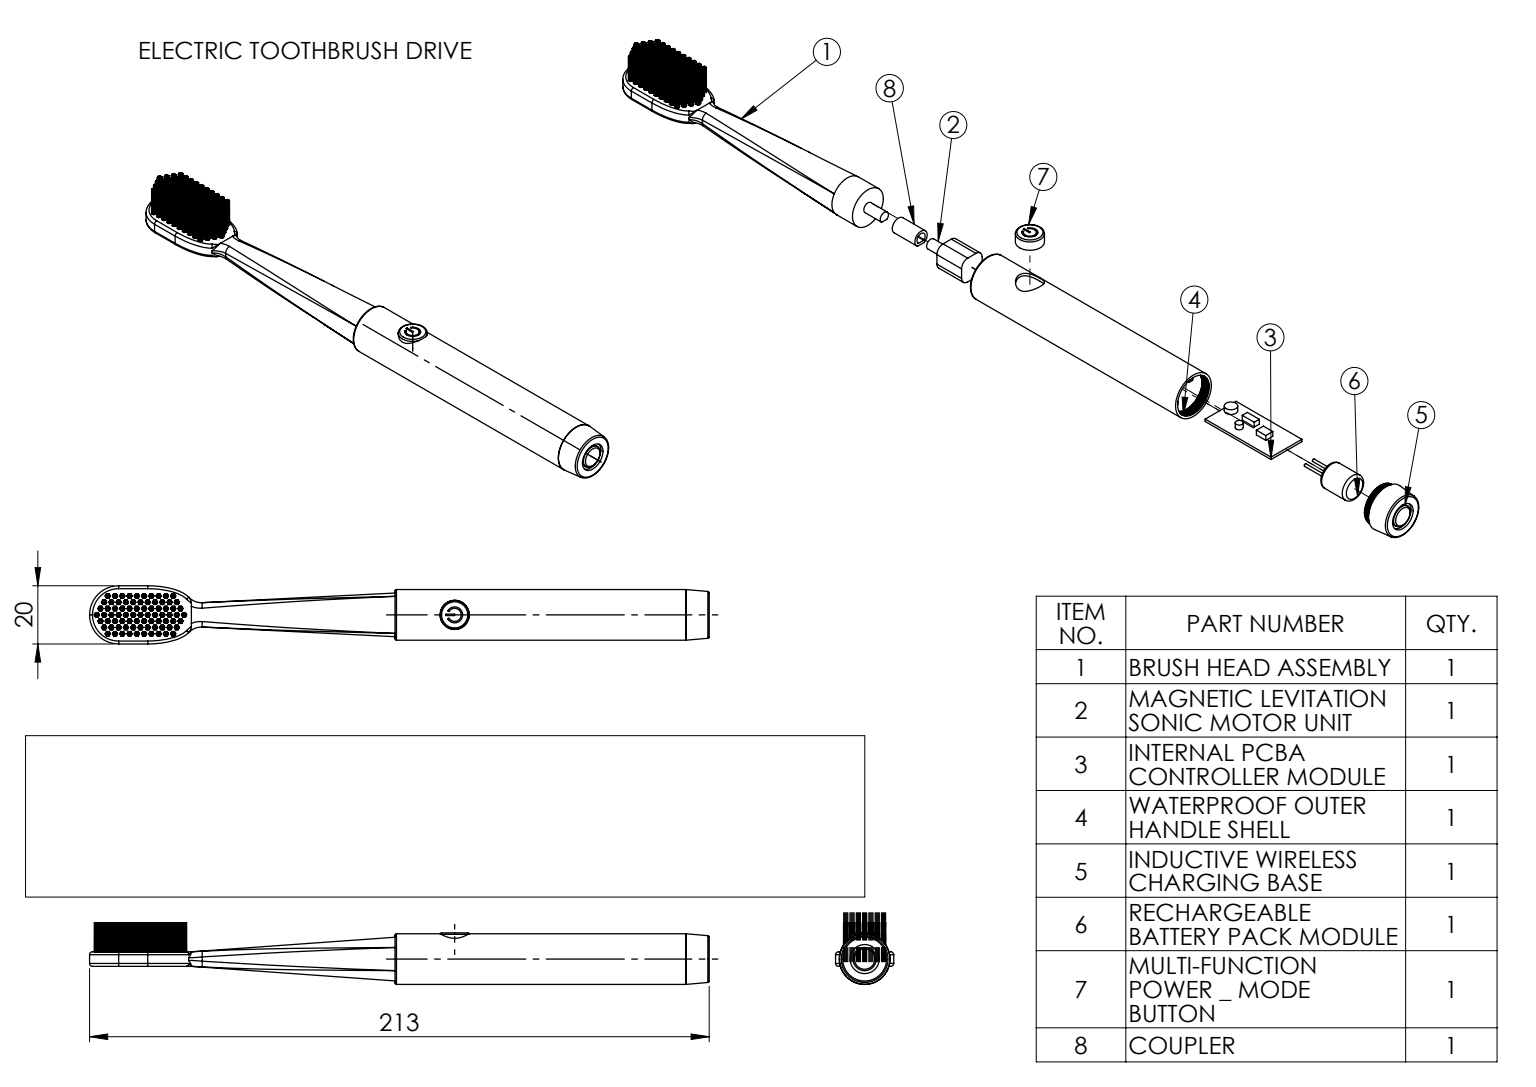
ISO-10303-21;
HEADER;
FILE_DESCRIPTION (('STEP AP214'),
    '1' );
FILE_NAME ('BR-831',
    '2026-10-02T09:26:43',
    ( '' ),
    ( '' ),
    'SwSTEP 2.0',
    'SolidWorks 2026',
    '' );
FILE_SCHEMA (( 'AUTOMOTIVE_DESIGN' ));
ENDSEC;

DATA;
#1 = ORIENTED_EDGE ( 'NONE', *, *, #111289, .F. ) ;
#2 = FACE_OUTER_BOUND ( 'NONE', #57861, .T. ) ;
#3 = DIRECTION ( 'NONE',  ( 0.000000000000000000, -0.000000000000000000, 1.000000000000000000 ) ) ;
#4 = EDGE_CURVE ( 'NONE', #10582, #102432, #129340, .T. ) ;
#5 = DIRECTION ( 'NONE',  ( -1.000000000000000000, -0.000000000000000000, -0.000000000000000000 ) ) ;
#6 = CIRCLE ( 'NONE', #73182, 0.09999999999999982514 ) ;
#7 = CARTESIAN_POINT ( 'NONE',  ( -5.200000000000025935, 12.50000000000000000, -3.983716857408426293 ) ) ;
#8 = ADVANCED_FACE ( 'NONE', ( #9369 ), #58491, .T. ) ;
#9 = ORIENTED_EDGE ( 'NONE', *, *, #43622, .T. ) ;
#10 = DIRECTION ( 'NONE',  ( -0.000000000000000000, 1.000000000000000000, -0.000000000000000000 ) ) ;
#12 = AXIS2_PLACEMENT_3D ( 'NONE', #43008, #33796, #72443 ) ;
#11 = AXIS2_PLACEMENT_3D ( 'NONE', #114880, #25207, #65127 ) ;
#13 = DIRECTION ( 'NONE',  ( 0.000000000000000000, 1.000000000000000000, 0.000000000000000000 ) ) ;
#14 = DIRECTION ( 'NONE',  ( 0.000000000000000000, 1.000000000000000000, 0.000000000000000000 ) ) ;
#15 = DIRECTION ( 'NONE',  ( 0.000000000000000000, 0.000000000000000000, 1.000000000000000000 ) ) ;
#16 = ORIENTED_EDGE ( 'NONE', *, *, #85327, .F. ) ;
#17 = ADVANCED_FACE ( 'NONE', ( #79412 ), #68276, .T. ) ;
#18 = ORIENTED_EDGE ( 'NONE', *, *, #72941, .T. ) ;
#19 = EDGE_CURVE ( 'NONE', #47255, #7520, #102130, .T. ) ;
#20 = LINE ( 'NONE', #41902, #103658 ) ;
#21 = ORIENTED_EDGE ( 'NONE', *, *, #108659, .T. ) ;
#22 = DIRECTION ( 'NONE',  ( 0.000000000000000000, -0.000000000000000000, 1.000000000000000000 ) ) ;
#25 = CARTESIAN_POINT ( 'NONE',  ( 17.50000000000000000, -2.499999999999999556, 2.333333333333337478 ) ) ;
#24 = CIRCLE ( 'NONE', #104488, 0.1000000000000002554 ) ;
#23 = AXIS2_PLACEMENT_3D ( 'NONE', #13282, #3477, #97012 ) ;
#26 = DIRECTION ( 'NONE',  ( -0.000000000000000000, -1.000000000000000000, -0.000000000000000000 ) ) ;
#27 = VERTEX_POINT ( 'NONE', #38865 ) ;
#28 = EDGE_CURVE ( 'NONE', #7615, #17965, #5955, .T. ) ;
#29 = CARTESIAN_POINT ( 'NONE',  ( -3.350000000000028511, 2.500000000000000000, -1.472243186433550122 ) ) ;
#30 = CARTESIAN_POINT ( 'NONE',  ( 4.549999999999939426, 2.500000000000000000, -6.495190528383302464 ) ) ;
#31 = DIRECTION ( 'NONE',  ( 0.000000000000000000, 0.000000000000000000, 1.000000000000000000 ) ) ;
#32 = DIRECTION ( 'NONE',  ( 0.000000000000000000, 0.000000000000000000, -1.000000000000000000 ) ) ;
#33 = DIRECTION ( 'NONE',  ( 0.000000000000000000, -0.000000000000000000, 1.000000000000000000 ) ) ;
#34 = EDGE_CURVE ( 'NONE', #123793, #101138, #123060, .T. ) ;
#35 = DIRECTION ( 'NONE',  ( 0.000000000000000000, 0.000000000000000000, 1.000000000000000000 ) ) ;
#36 = EDGE_LOOP ( 'NONE', ( #12557, #1627 ) ) ;
#37 = ORIENTED_EDGE ( 'NONE', *, *, #25424, .T. ) ;
#38 = CARTESIAN_POINT ( 'NONE',  ( -12.09999999999999609, 12.50000000000000000, -3.637306695894647390 ) ) ;
#39 = ORIENTED_EDGE ( 'NONE', *, *, #32172, .F. ) ;
#40 = DIRECTION ( 'NONE',  ( -0.000000000000000000, 1.000000000000000000, -0.000000000000000000 ) ) ;
#42 = ORIENTED_EDGE ( 'NONE', *, *, #56795, .T. ) ;
#41 = ORIENTED_EDGE ( 'NONE', *, *, #63489, .F. ) ;
#43 = ORIENTED_EDGE ( 'NONE', *, *, #113565, .F. ) ;
#44 = CARTESIAN_POINT ( 'NONE',  ( 87.49999999999998579, 2.781865847474100040, -7.000342182495692178 ) ) ;
#45 = CIRCLE ( 'NONE', #54416, 0.09999999999999982514 ) ;
#46 = CARTESIAN_POINT ( 'NONE',  ( -4.150000000000027889, 12.50000000000000000, -7.253104124594891289 ) ) ;
#47 = AXIS2_PLACEMENT_3D ( 'NONE', #50299, #49672, #91507 ) ;
#48 = CARTESIAN_POINT ( 'NONE',  ( 10.44999999999991047, 2.500000000000000000, 2.065063509461097624 ) ) ;
#49 = CARTESIAN_POINT ( 'NONE',  ( -7.300000000000018474, 12.50000000000000000, 0.3464101615137735735 ) ) ;
#50 = DIRECTION ( 'NONE',  ( 0.000000000000000000, -1.000000000000000000, 0.000000000000000000 ) ) ;
#51 = DIRECTION ( 'NONE',  ( 0.000000000000000000, 1.000000000000000000, 0.000000000000000000 ) ) ;
#52 = CARTESIAN_POINT ( 'NONE',  ( 5.649999999999932854, 2.500000000000000000, 1.918653347947321564 ) ) ;
#53 = DIRECTION ( 'NONE',  ( 0.000000000000000000, 0.000000000000000000, 1.000000000000000000 ) ) ;
#55 = AXIS2_PLACEMENT_3D ( 'NONE', #102666, #47947, #87846 ) ;
#54 = FACE_OUTER_BOUND ( 'NONE', #43393, .T. ) ;
#56 = ORIENTED_EDGE ( 'NONE', *, *, #30639, .F. ) ;
#57 = ORIENTED_EDGE ( 'NONE', *, *, #57612, .F. ) ;
#58 = DIRECTION ( 'NONE',  ( 0.000000000000000000, 0.000000000000000000, -1.000000000000000000 ) ) ;
#59 = EDGE_LOOP ( 'NONE', ( #8980, #73677, #9720, #73966 ) ) ;
#60 = EDGE_LOOP ( 'NONE', ( #125831, #14201 ) ) ;
#61 = CARTESIAN_POINT ( 'NONE',  ( 139.9358549477330200, 0.5000000000000000000, -1.098523788719517169 ) ) ;
#62 = CIRCLE ( 'NONE', #54353, 0.09999999999999982514 ) ;
#63 = EDGE_CURVE ( 'NONE', #31481, #67997, #18539, .T. ) ;
#64 = AXIS2_PLACEMENT_3D ( 'NONE', #6513, #46469, #75933 ) ;
#65 = DIRECTION ( 'NONE',  ( 1.000000000000000000, -0.000000000000000000, -0.000000000000000000 ) ) ;
#66 = CIRCLE ( 'NONE', #71172, 0.09999999999999982514 ) ;
#67 = DIRECTION ( 'NONE',  ( -4.274815082592931898E-19, -0.9999939076577903929, -0.003490651415223739937 ) ) ;
#68 = PLANE ( 'NONE',  #922 ) ;
#69 = ADVANCED_FACE ( 'NONE', ( #17890 ), #95870, .T. ) ;
#70 = DIRECTION ( 'NONE',  ( 0.000000000000000000, -0.9999939076577903929, 0.003490651415223739937 ) ) ;
#71 = ORIENTED_EDGE ( 'NONE', *, *, #16257, .F. ) ;
#72 = EDGE_CURVE ( 'NONE', #118132, #124753, #125105, .T. ) ;
#73 = EDGE_CURVE ( 'NONE', #114203, #127721, #49320, .T. ) ;
#75 = ADVANCED_FACE ( 'NONE', ( #29656 ), #54076, .T. ) ;
#74 = AXIS2_PLACEMENT_3D ( 'NONE', #92885, #52954, #31387 ) ;
#76 = VERTEX_POINT ( 'NONE', #89217 ) ;
#77 = PLANE ( 'NONE',  #104864 ) ;
#78 = EDGE_LOOP ( 'NONE', ( #93082, #10412 ) ) ;
#79 = CARTESIAN_POINT ( 'NONE',  ( 3.549999999999941203, 2.500000000000000000, 6.248780366869521430 ) ) ;
#80 = EDGE_CURVE ( 'NONE', #111625, #116591, #38188, .T. ) ;
#81 = AXIS2_PLACEMENT_3D ( 'NONE', #66786, #108010, #119130 ) ;
#82 = ORIENTED_EDGE ( 'NONE', *, *, #37576, .T. ) ;
#83 = ORIENTED_EDGE ( 'NONE', *, *, #49852, .F. ) ;
#84 = DIRECTION ( 'NONE',  ( -0.000000000000000000, 1.000000000000000000, -0.000000000000000000 ) ) ;
#85 = CARTESIAN_POINT ( 'NONE',  ( -7.100000000000017408, 2.500000000000000000, -4.922947341949753586 ) ) ;
#86 = EDGE_CURVE ( 'NONE', #7115, #38409, #127252, .T. ) ;
#87 = ADVANCED_FACE ( 'NONE', ( #57833 ), #118026, .T. ) ;
#88 = CARTESIAN_POINT ( 'NONE',  ( 13.34999999999990017, 2.500000000000000000, 1.572243186433545548 ) ) ;
#89 = DIRECTION ( 'NONE',  ( 0.000000000000000000, 0.000000000000000000, 1.000000000000000000 ) ) ;
#90 = CARTESIAN_POINT ( 'NONE',  ( 17.50000000000000000, -2.083333333333333925, 4.000000000000001776 ) ) ;
#91 = ORIENTED_EDGE ( 'NONE', *, *, #128566, .T. ) ;
#92 =( BOUNDED_CURVE ( )  B_SPLINE_CURVE ( 2, ( #80530, #51076, #39332, #70696, #90980, #28848, #108684 ),
 .UNSPECIFIED., .F., .F. ) 
 B_SPLINE_CURVE_WITH_KNOTS ( ( 3, 2, 2, 3 ),
 ( 0.7142857142857148567, 0.7380952380952386926, 0.7619047619047624176, 0.7857142857142862535 ),
 .UNSPECIFIED. ) 
 CURVE ( )  GEOMETRIC_REPRESENTATION_ITEM ( )  RATIONAL_B_SPLINE_CURVE ( ( 0.9999999999999968914, 0.8660254037844418162, 1.000000000000000000, 0.8660254037844387076, 1.000000000000000000, 0.8660254037844355990, 1.000000000000003109 ) ) 
 REPRESENTATION_ITEM ( '' )  );
#93 = DIRECTION ( 'NONE',  ( -0.000000000000000000, 1.000000000000000000, -0.000000000000000000 ) ) ;
#94 = DIRECTION ( 'NONE',  ( -4.274815082592931898E-19, -0.9999939076577903929, -0.003490651415223739937 ) ) ;
#95 = CARTESIAN_POINT ( 'NONE',  ( -2.050000000000033129, 2.500000000000000000, 2.165063509461097713 ) ) ;
#96 = CARTESIAN_POINT ( 'NONE',  ( -2.950000000000029932, 2.500000000000000000, -2.165063509461101710 ) ) ;
#97 = FACE_OUTER_BOUND ( 'NONE', #13668, .T. ) ;
#98 = EDGE_LOOP ( 'NONE', ( #5007, #26491, #107521, #16284 ) ) ;
#99 = ORIENTED_EDGE ( 'NONE', *, *, #48484, .T. ) ;
#100 = CIRCLE ( 'NONE', #16803, 0.06509327318403745899 ) ;
#101 = DIRECTION ( 'NONE',  ( 0.000000000000000000, -0.000000000000000000, 1.000000000000000000 ) ) ;
#102 = AXIS2_PLACEMENT_3D ( 'NONE', #59335, #77010, #59983 ) ;
#103 = ORIENTED_EDGE ( 'NONE', *, *, #8467, .T. ) ;
#104 = CARTESIAN_POINT ( 'NONE',  ( 17.41716098457700923, -1.872967139268051806, 4.643356076170615410 ) ) ;
#105 = LINE ( 'NONE', #118591, #98263 ) ;
#106 = AXIS2_PLACEMENT_3D ( 'NONE', #112814, #42811, #102353 ) ;
#107 = VERTEX_POINT ( 'NONE', #106909 ) ;
#108 = DIRECTION ( 'NONE',  ( 0.000000000000000000, 1.000000000000000000, 0.000000000000000000 ) ) ;
#109 = CARTESIAN_POINT ( 'NONE',  ( -6.650000000000019007, 2.500000000000000000, -5.802370205355749988 ) ) ;
#110 = CARTESIAN_POINT ( 'NONE',  ( 10.39999999999991509, 12.50000000000000000, -0.6928203230275542523 ) ) ;
#111 = CARTESIAN_POINT ( 'NONE',  ( 133.2169897921533845, 2.500000000000000000, -4.655597831175330548 ) ) ;
#112 = FACE_OUTER_BOUND ( 'NONE', #22375, .T. ) ;
#113 = VERTEX_POINT ( 'NONE', #17219 ) ;
#114 = DIRECTION ( 'NONE',  ( 0.000000000000000000, -0.9999939076577903929, 0.003490651415223739937 ) ) ;
#115 = DIRECTION ( 'NONE',  ( 0.000000000000000000, 0.000000000000000000, 1.000000000000000000 ) ) ;
#116 = CARTESIAN_POINT ( 'NONE',  ( -5.200000000000022382, 12.50000000000000000, 0.2813168883297361700 ) ) ;
#117 = ADVANCED_FACE ( 'NONE', ( #57173 ), #7419, .T. ) ;
#118 = VERTEX_POINT ( 'NONE', #50574 ) ;
#119 = DIRECTION ( 'NONE',  ( -0.000000000000000000, 1.000000000000000000, -0.000000000000000000 ) ) ;
#120 = EDGE_LOOP ( 'NONE', ( #58165, #15953, #18369, #114695 ) ) ;
#121 = CARTESIAN_POINT ( 'NONE',  ( -3.000000000000000000, 3.673940397442059868E-16, -5.000000000000004441 ) ) ;
#122 = DIRECTION ( 'NONE',  ( 0.000000000000000000, -0.000000000000000000, 1.000000000000000000 ) ) ;
#123 = DIRECTION ( 'NONE',  ( -4.274815082592931898E-19, -0.9999939076577903929, -0.003490651415223739937 ) ) ;
#124 = VERTEX_POINT ( 'NONE', #122556 ) ;
#125 = VECTOR ( 'NONE', #104094, 1000.000000000000000 ) ;
#126 = CARTESIAN_POINT ( 'NONE',  ( 2.099999999999950351, 12.50000000000000000, -5.022947341949754119 ) ) ;
#127 = CONICAL_SURFACE ( 'NONE', #108793, 0.1000000000000000472, 0.003490658503988666988 ) ;
#128 = CARTESIAN_POINT ( 'NONE',  ( 1.449999999999951328, 12.50000000000000000, -1.883746621131363597 ) ) ;
#129 = EDGE_LOOP ( 'NONE', ( #126937, #8373, #2231, #124616 ) ) ;
#130 = CARTESIAN_POINT ( 'NONE',  ( 8.749999999999957367, 2.500000000000000000, -6.595190528383302109 ) ) ;
#131 = EDGE_LOOP ( 'NONE', ( #50533, #103161, #4898, #53969 ) ) ;
#132 = CONICAL_SURFACE ( 'NONE', #108799, 0.1000000000000002554, 0.003490658503988666988 ) ;
#133 = FACE_OUTER_BOUND ( 'NONE', #40974, .T. ) ;
#134 = ORIENTED_EDGE ( 'NONE', *, *, #111458, .F. ) ;
#135 = DIRECTION ( 'NONE',  ( 0.000000000000000000, 0.000000000000000000, 1.000000000000000000 ) ) ;
#136 = CARTESIAN_POINT ( 'NONE',  ( -5.000000000000023093, 2.500000000000000000, 5.022947341949748790 ) ) ;
#137 = VERTEX_POINT ( 'NONE', #41429 ) ;
#138 = ORIENTED_EDGE ( 'NONE', *, *, #94725, .F. ) ;
#139 = DIRECTION ( 'NONE',  ( -0.000000000000000000, 1.000000000000000000, -0.000000000000000000 ) ) ;
#140 = FACE_OUTER_BOUND ( 'NONE', #29426, .T. ) ;
#141 = ORIENTED_EDGE ( 'NONE', *, *, #10108, .F. ) ;
#143 = FACE_OUTER_BOUND ( 'NONE', #8076, .T. ) ;
#142 = AXIS2_PLACEMENT_3D ( 'NONE', #9136, #110553, #47778 ) ;
#144 = CARTESIAN_POINT ( 'NONE',  ( 187.0677083336747160, -4.367472073101514418, -7.564683531250002702 ) ) ;
#145 = AXIS2_PLACEMENT_3D ( 'NONE', #45558, #95932, #15417 ) ;
#146 = DIRECTION ( 'NONE',  ( 0.000000000000000000, 0.000000000000000000, 1.000000000000000000 ) ) ;
#147 = CARTESIAN_POINT ( 'NONE',  ( -13.94999999999998685, 12.50000000000000000, -2.576566944158912964 ) ) ;
#148 = CARTESIAN_POINT ( 'NONE',  ( -8.300000000000009592, 12.50000000000000000, 4.395220292106234439 ) ) ;
#149 = DIRECTION ( 'NONE',  ( 0.000000000000000000, 0.000000000000000000, -1.000000000000000000 ) ) ;
#150 = CARTESIAN_POINT ( 'NONE',  ( -0.6500000000000394351, 2.500000000000000000, 6.941600689897073018 ) ) ;
#151 = CONICAL_SURFACE ( 'NONE', #75377, 0.09999999999999982514, 0.003490658503988666988 ) ;
#152 = EDGE_CURVE ( 'NONE', #35689, #125708, #77064, .T. ) ;
#153 = ORIENTED_EDGE ( 'NONE', *, *, #4789, .F. ) ;
#154 = ORIENTED_EDGE ( 'NONE', *, *, #109368, .T. ) ;
#155 = ORIENTED_EDGE ( 'NONE', *, *, #127999, .F. ) ;
#156 = AXIS2_PLACEMENT_3D ( 'NONE', #115565, #16713, #35116 ) ;
#157 = CARTESIAN_POINT ( 'NONE',  ( -6.249999999999981348, 12.50000000000000000, 2.165063509461097713 ) ) ;
#158 = DIRECTION ( 'NONE',  ( -0.000000000000000000, 1.000000000000000000, -0.000000000000000000 ) ) ;
#159 = DIRECTION ( 'NONE',  ( 0.000000000000000000, 0.000000000000000000, 1.000000000000000000 ) ) ;
#160 = EDGE_LOOP ( 'NONE', ( #92531, #41100 ) ) ;
#161 = EDGE_CURVE ( 'NONE', #53677, #62914, #60358, .T. ) ;
#162 = FACE_BOUND ( 'NONE', #99510, .T. ) ;
#163 = ORIENTED_EDGE ( 'NONE', *, *, #63007, .F. ) ;
#164 = EDGE_CURVE ( 'NONE', #64447, #41921, #37367, .T. ) ;
#165 = CARTESIAN_POINT ( 'NONE',  ( -7.900000000000014566, 12.50000000000000000, 0.6277270498435120194 ) ) ;
#166 = CARTESIAN_POINT ( 'NONE',  ( 7.899999999999924860, 2.500000000000000000, 5.022947341949748790 ) ) ;
#167 = LINE ( 'NONE', #110140, #49263 ) ;
#168 = FACE_OUTER_BOUND ( 'NONE', #42884, .T. ) ;
#169 = DIRECTION ( 'NONE',  ( -0.000000000000000000, 1.000000000000000000, -0.000000000000000000 ) ) ;
#170 = EDGE_CURVE ( 'NONE', #109777, #63696, #31113, .T. ) ;
#171 = DIRECTION ( 'NONE',  ( 0.000000000000000000, 1.000000000000000000, 0.000000000000000000 ) ) ;
#172 = EDGE_CURVE ( 'NONE', #110736, #16781, #3893, .T. ) ;
#173 = DIRECTION ( 'NONE',  ( 0.000000000000000000, 0.000000000000000000, -1.000000000000000000 ) ) ;
#174 = EDGE_CURVE ( 'NONE', #53227, #49994, #90490, .T. ) ;
#175 = CARTESIAN_POINT ( 'NONE',  ( 11.84999999999990727, 2.500000000000000000, 6.841600689897072485 ) ) ;
#176 = ADVANCED_FACE ( 'NONE', ( #101629 ), #14347, .T. ) ;
#177 = FACE_OUTER_BOUND ( 'NONE', #72478, .T. ) ;
#178 = ORIENTED_EDGE ( 'NONE', *, *, #7339, .F. ) ;
#179 = VERTEX_POINT ( 'NONE', #111417 ) ;
#180 = VERTEX_POINT ( 'NONE', #20488 ) ;
#181 = VERTEX_POINT ( 'NONE', #62977 ) ;
#182 = DIRECTION ( 'NONE',  ( 0.000000000000000000, 1.000000000000000000, 0.000000000000000000 ) ) ;
#183 = CIRCLE ( 'NONE', #48229, 0.06509327318403741736 ) ;
#184 = LINE ( 'NONE', #92445, #36085 ) ;
#185 = AXIS2_PLACEMENT_3D ( 'NONE', #74145, #15849, #15191 ) ;
#186 = AXIS2_PLACEMENT_3D ( 'NONE', #87460, #107759, #127405 ) ;
#188 = ORIENTED_EDGE ( 'NONE', *, *, #84597, .T. ) ;
#187 = EDGE_LOOP ( 'NONE', ( #105520, #67716, #77716, #43576 ) ) ;
#189 = EDGE_CURVE ( 'NONE', #19176, #5233, #120978, .T. ) ;
#190 = ORIENTED_EDGE ( 'NONE', *, *, #82832, .T. ) ;
#191 = AXIS2_PLACEMENT_3D ( 'NONE', #50501, #49243, #90414 ) ;
#192 = DIRECTION ( 'NONE',  ( -0.000000000000000000, -1.000000000000000000, -0.000000000000000000 ) ) ;
#193 = DIRECTION ( 'NONE',  ( 0.000000000000000000, -0.000000000000000000, 1.000000000000000000 ) ) ;
#194 = DIRECTION ( 'NONE',  ( -0.000000000000000000, -1.000000000000000000, -0.000000000000000000 ) ) ;
#195 = DIRECTION ( 'NONE',  ( 0.000000000000000000, 0.000000000000000000, -1.000000000000000000 ) ) ;
#196 = CARTESIAN_POINT ( 'NONE',  ( -8.950000000000004619, 12.50000000000000000, 6.148780366869520897 ) ) ;
#197 = CONICAL_SURFACE ( 'NONE', #119337, 0.1000000000000000056, 0.003490658503988666988 ) ;
#198 = DIRECTION ( 'NONE',  ( 0.000000000000000000, -0.000000000000000000, 1.000000000000000000 ) ) ;
#199 = ORIENTED_EDGE ( 'NONE', *, *, #119327, .F. ) ;
#200 = DIRECTION ( 'NONE',  ( 0.000000000000000000, -0.9999939076577903929, 0.003490651415223739937 ) ) ;
#201 = ORIENTED_EDGE ( 'NONE', *, *, #13341, .F. ) ;
#202 = ORIENTED_EDGE ( 'NONE', *, *, #70316, .F. ) ;
#203 = ORIENTED_EDGE ( 'NONE', *, *, #126845, .T. ) ;
#204 = DIRECTION ( 'NONE',  ( -0.000000000000000000, -1.000000000000000000, -0.000000000000000000 ) ) ;
#205 = EDGE_CURVE ( 'NONE', #70284, #50485, #21114, .T. ) ;
#206 = ORIENTED_EDGE ( 'NONE', *, *, #92160, .F. ) ;
#207 = ORIENTED_EDGE ( 'NONE', *, *, #83833, .F. ) ;
#208 = FILL_AREA_STYLE ('',( #102307 ) ) ;
#209 = AXIS2_PLACEMENT_3D ( 'NONE', #67296, #8398, #18868 ) ;
#210 = CARTESIAN_POINT ( 'NONE',  ( 9.399999999999915090, 2.500000000000000000, 3.983716857408420964 ) ) ;
#211 = CARTESIAN_POINT ( 'NONE',  ( 14.14999999999989377, 2.500000000000000000, -2.857883832488653741 ) ) ;
#212 = DIRECTION ( 'NONE',  ( -0.000000000000000000, 1.000000000000000000, -0.000000000000000000 ) ) ;
#213 = ADVANCED_FACE ( 'NONE', ( #70872 ), #100964, .T. ) ;
#214 = DIRECTION ( 'NONE',  ( -0.000000000000000000, 1.000000000000000000, -0.000000000000000000 ) ) ;
#215 = EDGE_CURVE ( 'NONE', #14404, #106677, #98609, .T. ) ;
#216 = ORIENTED_EDGE ( 'NONE', *, *, #25647, .T. ) ;
#217 = EDGE_CURVE ( 'NONE', #101886, #26135, #31742, .T. ) ;
#218 = DIRECTION ( 'NONE',  ( 0.000000000000000000, 1.000000000000000000, 0.000000000000000000 ) ) ;
#219 = CONICAL_SURFACE ( 'NONE', #115215, 0.1000000000000000472, 0.003490658503988666988 ) ;
#220 = CIRCLE ( 'NONE', #73386, 0.06509327318403745899 ) ;
#221 = ORIENTED_EDGE ( 'NONE', *, *, #31291, .F. ) ;
#223 = EDGE_CURVE ( 'NONE', #51195, #50358, #69379, .T. ) ;
#222 = DIRECTION ( 'NONE',  ( 0.000000000000000000, 0.000000000000000000, 1.000000000000000000 ) ) ;
#224 = VERTEX_POINT ( 'NONE', #112735 ) ;
#225 = DIRECTION ( 'NONE',  ( -0.000000000000000000, 1.000000000000000000, -0.000000000000000000 ) ) ;
#226 = CARTESIAN_POINT ( 'NONE',  ( 21.24754738303297330, 0.7337760880902002292, -4.182111650399407132 ) ) ;
#228 = ORIENTED_EDGE ( 'NONE', *, *, #115605, .T. ) ;
#227 = ADVANCED_FACE ( 'NONE', ( #89853 ), #30320, .T. ) ;
#229 = CARTESIAN_POINT ( 'NONE',  ( 5.599999999999931255, 12.50000000000000000, 3.918623584224382839 ) ) ;
#230 = EDGE_CURVE ( 'NONE', #34015, #92739, #32256, .T. ) ;
#231 = DIRECTION ( 'NONE',  ( 0.000000000000000000, 0.000000000000000000, -1.000000000000000000 ) ) ;
#232 = EDGE_LOOP ( 'NONE', ( #14783, #39929, #121308, #33112 ) ) ;
#233 = CONICAL_SURFACE ( 'NONE', #8535, 0.1000000000000002554, 0.003490658503988666988 ) ;
#234 = EDGE_CURVE ( 'NONE', #45310, #78495, #22435, .T. ) ;
#235 = AXIS2_PLACEMENT_3D ( 'NONE', #117904, #58371, #98266 ) ;
#236 = EDGE_CURVE ( 'NONE', #86441, #35274, #92360, .T. ) ;
#237 = EDGE_CURVE ( 'NONE', #3662, #62906, #43359, .T. ) ;
#238 = CARTESIAN_POINT ( 'NONE',  ( 10.64999999999990976, 12.50000000000000000, 1.753560074763284016 ) ) ;
#239 = ORIENTED_EDGE ( 'NONE', *, *, #20618, .F. ) ;
#240 = VERTEX_POINT ( 'NONE', #115266 ) ;
#241 = DIRECTION ( 'NONE',  ( 0.000000000000000000, 0.000000000000000000, 1.000000000000000000 ) ) ;
#242 = FACE_OUTER_BOUND ( 'NONE', #74937, .T. ) ;
#243 = LINE ( 'NONE', #68992, #50135 ) ;
#244 = DIRECTION ( 'NONE',  ( 0.000000000000000000, 0.000000000000000000, 1.000000000000000000 ) ) ;
#245 = EDGE_CURVE ( 'NONE', #43167, #39233, #13868, .T. ) ;
#246 = AXIS2_PLACEMENT_3D ( 'NONE', #45056, #45692, #64672 ) ;
#247 = CIRCLE ( 'NONE', #62948, 0.1000000000000000472 ) ;
#248 = CARTESIAN_POINT ( 'NONE',  ( 6.049999999999935874, 2.500000000000000000, -6.941600689897077459 ) ) ;
#249 = VERTEX_POINT ( 'NONE', #105488 ) ;
#250 = DIRECTION ( 'NONE',  ( -0.000000000000000000, -1.000000000000000000, -0.000000000000000000 ) ) ;
#251 = VERTEX_POINT ( 'NONE', #124483 ) ;
#252 = CARTESIAN_POINT ( 'NONE',  ( -1.450000000000035483, 12.50000000000000000, 1.883746621131358934 ) ) ;
#253 = CARTESIAN_POINT ( 'NONE',  ( 8.099999999999921485, 2.500000000000000000, 0.2464101615137735679 ) ) ;
#254 = AXIS2_PLACEMENT_3D ( 'NONE', #24478, #34962, #47347 ) ;
#255 = AXIS2_PLACEMENT_3D ( 'NONE', #22150, #12292, #81057 ) ;
#256 = CARTESIAN_POINT ( 'NONE',  ( 186.4218750003414016, 0.000000000000000000, 7.564683531250000925 ) ) ;
#257 = PLANE ( 'NONE',  #99050 ) ;
#258 = DIRECTION ( 'NONE',  ( 0.000000000000000000, -0.9999939076577903929, 0.003490651415223739937 ) ) ;
#259 = DIRECTION ( 'NONE',  ( 0.000000000000000000, 0.000000000000000000, 1.000000000000000000 ) ) ;
#260 = CARTESIAN_POINT ( 'NONE',  ( -11.89999999999999680, 2.500000000000000000, -4.576537180435975571 ) ) ;
#261 = ORIENTED_EDGE ( 'NONE', *, *, #25908, .F. ) ;
#262 = DIRECTION ( 'NONE',  ( 0.000000000000000000, -0.9999939076577903929, 0.003490651415223739937 ) ) ;
#263 = DIRECTION ( 'NONE',  ( -0.000000000000000000, 1.000000000000000000, -0.000000000000000000 ) ) ;
#264 = CARTESIAN_POINT ( 'NONE',  ( 13.14999999999989733, 2.500000000000000000, -2.511473670974877948 ) ) ;
#265 = ORIENTED_EDGE ( 'NONE', *, *, #80354, .F. ) ;
#266 = CARTESIAN_POINT ( 'NONE',  ( -11.44999999999999929, 2.500000000000000000, -1.718653347947322052 ) ) ;
#267 = EDGE_CURVE ( 'NONE', #13125, #47712, #71425, .T. ) ;
#268 = EDGE_LOOP ( 'NONE', ( #106768, #28625 ) ) ;
#269 = VERTEX_POINT ( 'NONE', #123201 ) ;
#270 = DIRECTION ( 'NONE',  ( 0.000000000000000000, 0.000000000000000000, 1.000000000000000000 ) ) ;
#271 = AXIS2_PLACEMENT_3D ( 'NONE', #106645, #15669, #35977 ) ;
#272 = AXIS2_PLACEMENT_3D ( 'NONE', #94108, #74472, #114381 ) ;
#273 = AXIS2_PLACEMENT_3D ( 'NONE', #118714, #118066, #68969 ) ;
#274 = EDGE_LOOP ( 'NONE', ( #97297, #118927 ) ) ;
#275 = DIRECTION ( 'NONE',  ( 0.000000000000000000, 0.000000000000000000, 1.000000000000000000 ) ) ;
#276 = CARTESIAN_POINT ( 'NONE',  ( 5.799999999999931433, 12.50000000000000000, 4.395220292106234439 ) ) ;
#277 = ORIENTED_EDGE ( 'NONE', *, *, #87516, .F. ) ;
#279 = LINE ( 'NONE', #110252, #23714 ) ;
#278 = VECTOR ( 'NONE', #38628, 1000.000000000000000 ) ;
#280 = CIRCLE ( 'NONE', #81853, 0.06509327318403741736 ) ;
#281 = DIRECTION ( 'NONE',  ( 0.000000000000000000, -0.9999939076577903929, 0.003490651415223739937 ) ) ;
#282 = DIRECTION ( 'NONE',  ( 0.000000000000000000, 0.000000000000000000, 1.000000000000000000 ) ) ;
#283 = ADVANCED_FACE ( 'NONE', ( #24987 ), #65155, .T. ) ;
#284 = ORIENTED_EDGE ( 'NONE', *, *, #126777, .T. ) ;
#285 = ORIENTED_EDGE ( 'NONE', *, *, #2427, .F. ) ;
#286 = ORIENTED_EDGE ( 'NONE', *, *, #35114, .F. ) ;
#287 = DIRECTION ( 'NONE',  ( -0.000000000000000000, -1.000000000000000000, -0.000000000000000000 ) ) ;
#288 = DIRECTION ( 'NONE',  ( 0.000000000000000000, 0.000000000000000000, 1.000000000000000000 ) ) ;
#289 = DIRECTION ( 'NONE',  ( -0.000000000000000000, 1.000000000000000000, -0.000000000000000000 ) ) ;
#290 = FACE_BOUND ( 'NONE', #126554, .T. ) ;
#291 = ORIENTED_EDGE ( 'NONE', *, *, #83216, .F. ) ;
#292 = DIRECTION ( 'NONE',  ( 0.000000000000000000, 0.000000000000000000, 1.000000000000000000 ) ) ;
#293 = DIRECTION ( 'NONE',  ( 0.000000000000000000, -0.000000000000000000, 1.000000000000000000 ) ) ;
#294 = ORIENTED_EDGE ( 'NONE', *, *, #21313, .F. ) ;
#295 = DIRECTION ( 'NONE',  ( 0.000000000000000000, 0.000000000000000000, -1.000000000000000000 ) ) ;
#296 = CARTESIAN_POINT ( 'NONE',  ( -11.04999999999999893, 2.500000000000000000, 1.818653347947321475 ) ) ;
#297 = DIRECTION ( 'NONE',  ( -0.000000000000000000, -1.000000000000000000, -0.000000000000000000 ) ) ;
#298 = DIRECTION ( 'NONE',  ( 0.000000000000000000, -0.9999939076577903929, 0.003490651415223739937 ) ) ;
#299 = CARTESIAN_POINT ( 'NONE',  ( 2.049999999999950084, 2.500000000000000000, 2.165063509461097713 ) ) ;
#300 = DIRECTION ( 'NONE',  ( 0.000000000000000000, 1.000000000000000000, 0.000000000000000000 ) ) ;
#301 = LINE ( 'NONE', #128666, #48207 ) ;
#302 = CIRCLE ( 'NONE', #73475, 0.1000000000000000472 ) ;
#303 = EDGE_CURVE ( 'NONE', #26935, #23200, #114647, .T. ) ;
#304 = ORIENTED_EDGE ( 'NONE', *, *, #29474, .T. ) ;
#305 = ORIENTED_EDGE ( 'NONE', *, *, #98641, .F. ) ;
#306 = ORIENTED_EDGE ( 'NONE', *, *, #68939, .F. ) ;
#307 = EDGE_LOOP ( 'NONE', ( #81864, #53697, #107603, #18782 ) ) ;
#308 = DIRECTION ( 'NONE',  ( 0.000000000000000000, -0.9999939076577903929, 0.003490651415223739937 ) ) ;
#309 = CARTESIAN_POINT ( 'NONE',  ( 13.74999999999993072, 2.500000000000000000, -2.165063509461101710 ) ) ;
#310 = EDGE_LOOP ( 'NONE', ( #57715, #102459 ) ) ;
#311 = FACE_BOUND ( 'NONE', #39121, .T. ) ;
#312 = ADVANCED_FACE ( 'NONE', ( #15798 ), #25451, .T. ) ;
#313 = LINE ( 'NONE', #12086, #37510 ) ;
#314 = VECTOR ( 'NONE', #88274, 1000.000000000000000 ) ;
#315 = CIRCLE ( 'NONE', #10772, 0.09999999999999982514 ) ;
#316 = DIRECTION ( 'NONE',  ( 0.000000000000000000, 0.000000000000000000, 1.000000000000000000 ) ) ;
#317 = CARTESIAN_POINT ( 'NONE',  ( 2.949999999999943334, 12.50000000000000000, 6.495190528383297135 ) ) ;
#318 = ADVANCED_FACE ( 'NONE', ( #4048 ), #118462, .T. ) ;
#319 = FACE_OUTER_BOUND ( 'NONE', #53920, .T. ) ;
#320 = EDGE_CURVE ( 'NONE', #39409, #2500, #55733, .T. ) ;
#321 = DIRECTION ( 'NONE',  ( 0.000000000000000000, 0.000000000000000000, 1.000000000000000000 ) ) ;
#322 = EDGE_CURVE ( 'NONE', #118758, #53470, #49534, .T. ) ;
#323 = CARTESIAN_POINT ( 'NONE',  ( -1.050000000000038680, 2.500000000000000000, 6.741600689897071952 ) ) ;
#324 = EDGE_CURVE ( 'NONE', #23588, #89858, #112217, .T. ) ;
#325 = EDGE_LOOP ( 'NONE', ( #61905, #50116, #33161, #106060 ) ) ;
#326 = EDGE_CURVE ( 'NONE', #98580, #67678, #66234, .T. ) ;
#327 = AXIS2_PLACEMENT_3D ( 'NONE', #75611, #34437, #106376 ) ;
#328 = ORIENTED_EDGE ( 'NONE', *, *, #89775, .T. ) ;
#329 = CIRCLE ( 'NONE', #90217, 0.06509327318403745899 ) ;
#330 = ORIENTED_EDGE ( 'NONE', *, *, #80772, .F. ) ;
#331 = VERTEX_POINT ( 'NONE', #113362 ) ;
#332 = ORIENTED_EDGE ( 'NONE', *, *, #4672, .F. ) ;
#333 = ORIENTED_EDGE ( 'NONE', *, *, #89472, .T. ) ;
#334 = VECTOR ( 'NONE', #40375, 1000.000000000000000 ) ;
#335 = DIRECTION ( 'NONE',  ( 0.000000000000000000, 1.000000000000000000, 0.000000000000000000 ) ) ;
#336 = DIRECTION ( 'NONE',  ( 0.000000000000000000, 1.000000000000000000, 0.000000000000000000 ) ) ;
#337 = ORIENTED_EDGE ( 'NONE', *, *, #87514, .F. ) ;
#338 = ADVANCED_FACE ( 'NONE', ( #43998 ), #105950, .T. ) ;
#339 = CARTESIAN_POINT ( 'NONE',  ( 11.24999999999990585, 12.50000000000000000, -5.802370205355749988 ) ) ;
#340 = AXIS2_PLACEMENT_3D ( 'NONE', #87388, #97223, #127343 ) ;
#341 = EDGE_CURVE ( 'NONE', #29920, #106540, #93098, .T. ) ;
#342 = EDGE_CURVE ( 'NONE', #41239, #126826, #74090, .T. ) ;
#343 = CARTESIAN_POINT ( 'NONE',  ( 7.049999999999928768, 2.500000000000000000, -2.165063509461101710 ) ) ;
#344 = CIRCLE ( 'NONE', #48391, 0.06509327318403745899 ) ;
#345 = CIRCLE ( 'NONE', #4533, 0.06509327318403745899 ) ;
#346 = CARTESIAN_POINT ( 'NONE',  ( 184.9427083336747160, -6.551208109652278289, 3.782341765624995134 ) ) ;
#347 = DIRECTION ( 'NONE',  ( 0.000000000000000000, 0.000000000000000000, 1.000000000000000000 ) ) ;
#348 = DIRECTION ( 'NONE',  ( 0.000000000000000000, 1.000000000000000000, 0.000000000000000000 ) ) ;
#349 = ORIENTED_EDGE ( 'NONE', *, *, #95079, .T. ) ;
#350 = FACE_OUTER_BOUND ( 'NONE', #62832, .T. ) ;
#351 = ORIENTED_EDGE ( 'NONE', *, *, #55703, .F. ) ;
#352 = ORIENTED_EDGE ( 'NONE', *, *, #90036, .T. ) ;
#353 = PLANE ( 'NONE',  #42636 ) ;
#354 = CARTESIAN_POINT ( 'NONE',  ( 185.5000000000000000, 0.000000000000000000, 7.700000000000000178 ) ) ;
#355 = DIRECTION ( 'NONE',  ( 0.000000000000000000, 0.000000000000000000, -1.000000000000000000 ) ) ;
#356 = VERTEX_POINT ( 'NONE', #26287 ) ;
#357 = ORIENTED_EDGE ( 'NONE', *, *, #4257, .F. ) ;
#358 = PLANE ( 'NONE',  #73574 ) ;
#359 = DIRECTION ( 'NONE',  ( 0.000000000000000000, -0.9999939076577903929, 0.003490651415223739937 ) ) ;
#360 = CARTESIAN_POINT ( 'NONE',  ( -9.350000000000004974, 2.500000000000000000, 6.148780366869520897 ) ) ;
#362 = DIRECTION ( 'NONE',  ( 0.000000000000000000, 0.000000000000000000, -1.000000000000000000 ) ) ;
#361 = VECTOR ( 'NONE', #77259, 1000.000000000000000 ) ;
#363 = EDGE_LOOP ( 'NONE', ( #37581, #94874, #128100, #15237 ) ) ;
#364 = CONICAL_SURFACE ( 'NONE', #12877, 0.1000000000000002554, 0.003490658503988666988 ) ;
#365 = VECTOR ( 'NONE', #93137, 1000.000000000000000 ) ;
#366 = CARTESIAN_POINT ( 'NONE',  ( -0.8500000000000395017, 2.500000000000000000, 2.065063509461097624 ) ) ;
#367 = EDGE_LOOP ( 'NONE', ( #100670, #104053, #13822, #112020 ) ) ;
#368 = LINE ( 'NONE', #39705, #26989 ) ;
#369 = AXIS2_PLACEMENT_3D ( 'NONE', #120392, #31376, #29436 ) ;
#370 = ORIENTED_EDGE ( 'NONE', *, *, #75435, .F. ) ;
#371 = FACE_OUTER_BOUND ( 'NONE', #86248, .T. ) ;
#372 = AXIS2_PLACEMENT_3D ( 'NONE', #42902, #31772, #111612 ) ;
#373 = CARTESIAN_POINT ( 'NONE',  ( 76.44221964357954846, -3.905139022502750024, 5.869652876108133910 ) ) ;
#374 = CARTESIAN_POINT ( 'NONE',  ( 0.3999999999999628852, 2.500000000000000000, 0.6928203230275518099 ) ) ;
#375 = AXIS2_PLACEMENT_3D ( 'NONE', #56457, #126503, #46017 ) ;
#376 = ADVANCED_FACE ( 'NONE', ( #83896 ), #32815, .T. ) ;
#377 = CARTESIAN_POINT ( 'NONE',  ( -6.900000000000019007, 2.500000000000000000, -0.2464101615137783419 ) ) ;
#378 = VERTEX_POINT ( 'NONE', #53172 ) ;
#379 = VECTOR ( 'NONE', #86112, 1000.000000000000000 ) ;
#380 = ADVANCED_FACE ( 'NONE', ( #3414 ), #82983, .T. ) ;
#381 = DIRECTION ( 'NONE',  ( 0.000000000000000000, 0.000000000000000000, -1.000000000000000000 ) ) ;
#382 = EDGE_CURVE ( 'NONE', #121670, #96705, #103561, .T. ) ;
#383 = CARTESIAN_POINT ( 'NONE',  ( -10.84999999999999964, 2.500000000000000000, 7.188010851410848723 ) ) ;
#384 = VERTEX_POINT ( 'NONE', #98874 ) ;
#385 = ORIENTED_EDGE ( 'NONE', *, *, #77434, .T. ) ;
#386 = ORIENTED_EDGE ( 'NONE', *, *, #106988, .T. ) ;
#387 = DIRECTION ( 'NONE',  ( 0.000000000000000000, -0.000000000000000000, 1.000000000000000000 ) ) ;
#388 = DIRECTION ( 'NONE',  ( 0.000000000000000000, 0.000000000000000000, 1.000000000000000000 ) ) ;
#389 = DIRECTION ( 'NONE',  ( 0.000000000000000000, -0.000000000000000000, 1.000000000000000000 ) ) ;
#390 = CARTESIAN_POINT ( 'NONE',  ( -13.29999999999999005, 2.500000000000000000, -4.330127018922198978 ) ) ;
#391 = DIRECTION ( 'NONE',  ( 0.000000000000000000, 1.000000000000000000, 0.000000000000000000 ) ) ;
#392 = ADVANCED_FACE ( 'NONE', ( #7261 ), #95484, .T. ) ;
#393 = DIRECTION ( 'NONE',  ( -0.000000000000000000, 1.000000000000000000, -0.000000000000000000 ) ) ;
#394 = DIRECTION ( 'NONE',  ( 0.000000000000000000, 1.000000000000000000, 0.000000000000000000 ) ) ;
#395 = CARTESIAN_POINT ( 'NONE',  ( -3.750000000000026201, 2.500000000000000000, 5.802370205355744659 ) ) ;
#396 = PLANE ( 'NONE',  #56788 ) ;
#397 = AXIS2_PLACEMENT_3D ( 'NONE', #46964, #58707, #116961 ) ;
#398 = AXIS2_PLACEMENT_3D ( 'NONE', #61758, #101673, #11989 ) ;
#399 = ORIENTED_EDGE ( 'NONE', *, *, #91207, .T. ) ;
#400 = DIRECTION ( 'NONE',  ( -0.000000000000000000, -1.000000000000000000, -0.000000000000000000 ) ) ;
#401 = CARTESIAN_POINT ( 'NONE',  ( -14.14999999999998614, 12.50000000000000000, 1.472243186433549456 ) ) ;
#402 = CARTESIAN_POINT ( 'NONE',  ( -12.49999999999999289, 12.50000000000000000, -0.6928203230275500335 ) ) ;
#403 = ADVANCED_FACE ( 'NONE', ( #66826 ), #37652, .T. ) ;
#404 = DIRECTION ( 'NONE',  ( 0.000000000000000000, 0.000000000000000000, 1.000000000000000000 ) ) ;
#405 = CARTESIAN_POINT ( 'NONE',  ( 7.049999999999928768, 2.500000000000000000, 6.495190528383297135 ) ) ;
#406 = CIRCLE ( 'NONE', #33873, 0.06509327318403745899 ) ;
#407 = AXIS2_PLACEMENT_3D ( 'NONE', #20032, #59980, #99882 ) ;
#408 = VERTEX_POINT ( 'NONE', #17726 ) ;
#409 = CARTESIAN_POINT ( 'NONE',  ( -7.050000000000013145, 2.500000000000000000, 6.595190528383296780 ) ) ;
#410 = CIRCLE ( 'NONE', #42297, 0.06509327318403743123 ) ;
#411 = CIRCLE ( 'NONE', #58928, 0.06509327318403745899 ) ;
#412 = DIRECTION ( 'NONE',  ( -0.000000000000000000, 1.000000000000000000, -0.000000000000000000 ) ) ;
#414 = ORIENTED_EDGE ( 'NONE', *, *, #38047, .F. ) ;
#413 = DIRECTION ( 'NONE',  ( 0.000000000000000000, -0.9999939076577903929, 0.003490651415223739937 ) ) ;
#415 = EDGE_LOOP ( 'NONE', ( #59433, #27224 ) ) ;
#417 = CIRCLE ( 'NONE', #107031, 0.06509327318403745899 ) ;
#416 = CARTESIAN_POINT ( 'NONE',  ( -12.29999999999999716, 2.500000000000000000, 0.4464101615137776591 ) ) ;
#418 = EDGE_CURVE ( 'NONE', #72177, #71951, #50185, .T. ) ;
#419 = ORIENTED_EDGE ( 'NONE', *, *, #57235, .T. ) ;
#420 = VECTOR ( 'NONE', #30289, 1000.000000000000000 ) ;
#422 = ORIENTED_EDGE ( 'NONE', *, *, #20340, .F. ) ;
#421 = AXIS2_PLACEMENT_3D ( 'NONE', #24378, #102927, #93129 ) ;
#423 = CIRCLE ( 'NONE', #100772, 0.06509327318403745899 ) ;
#424 = FACE_OUTER_BOUND ( 'NONE', #6671, .T. ) ;
#425 = AXIS2_PLACEMENT_3D ( 'NONE', #127655, #7217, #37985 ) ;
#426 = DIRECTION ( 'NONE',  ( 0.000000000000000000, 0.000000000000000000, 1.000000000000000000 ) ) ;
#427 = DIRECTION ( 'NONE',  ( -0.000000000000000000, 1.000000000000000000, -0.000000000000000000 ) ) ;
#428 = CARTESIAN_POINT ( 'NONE',  ( 0.1999999999999627909, 12.50000000000000000, 0.2813168883297384459 ) ) ;
#429 = ORIENTED_EDGE ( 'NONE', *, *, #31666, .F. ) ;
#430 = CIRCLE ( 'NONE', #77706, 0.06509327318403745899 ) ;
#431 = FACE_OUTER_BOUND ( 'NONE', #54831, .T. ) ;
#432 = ORIENTED_EDGE ( 'NONE', *, *, #72222, .F. ) ;
#433 = DIRECTION ( 'NONE',  ( -0.000000000000000000, 1.000000000000000000, -0.000000000000000000 ) ) ;
#434 = FACE_OUTER_BOUND ( 'NONE', #53931, .T. ) ;
#435 = ADVANCED_FACE ( 'NONE', ( #9210 ), #17059, .T. ) ;
#436 = DIRECTION ( 'NONE',  ( -4.274815082592931898E-19, -0.9999939076577903929, -0.003490651415223739937 ) ) ;
#437 = ORIENTED_EDGE ( 'NONE', *, *, #120658, .F. ) ;
#438 = ORIENTED_EDGE ( 'NONE', *, *, #126436, .T. ) ;
#439 = ORIENTED_EDGE ( 'NONE', *, *, #64645, .T. ) ;
#440 = EDGE_LOOP ( 'NONE', ( #14150, #118505 ) ) ;
#441 = EDGE_LOOP ( 'NONE', ( #46577, #104696, #83589, #8113 ) ) ;
#442 = CARTESIAN_POINT ( 'NONE',  ( 12.09999999999990550, 2.500000000000000000, -3.637306695894650055 ) ) ;
#443 = CARTESIAN_POINT ( 'NONE',  ( 10.06913504587783947, 2.500000000000000888, 8.158951466337887481 ) ) ;
#444 = FACE_OUTER_BOUND ( 'NONE', #25643, .T. ) ;
#445 = FACE_BOUND ( 'NONE', #8268, .T. ) ;
#446 = CARTESIAN_POINT ( 'NONE',  ( 1.249999999999988454, 12.50000000000000000, -2.165063509461101710 ) ) ;
#447 = CARTESIAN_POINT ( 'NONE',  ( 186.9479166673494603, -6.668395609140176816, -3.850000000000003642 ) ) ;
#448 = FACE_OUTER_BOUND ( 'NONE', #12746, .T. ) ;
#449 = DIRECTION ( 'NONE',  ( -4.274815082592931898E-19, -0.9999939076577903929, -0.003490651415223739937 ) ) ;
#450 = CIRCLE ( 'NONE', #88369, 2.000000000000000000 ) ;
#452 = AXIS2_PLACEMENT_3D ( 'NONE', #51765, #22319, #31478 ) ;
#451 = DIRECTION ( 'NONE',  ( 0.000000000000000000, -0.000000000000000000, 1.000000000000000000 ) ) ;
#453 = DIRECTION ( 'NONE',  ( 0.000000000000000000, 1.000000000000000000, 0.000000000000000000 ) ) ;
#454 = CARTESIAN_POINT ( 'NONE',  ( 12.49999999999993605, 2.500000000000000000, 0.09999999999999772959 ) ) ;
#455 = VECTOR ( 'NONE', #15572, 1000.000000000000000 ) ;
#457 = LINE ( 'NONE', #62637, #1297 ) ;
#456 = CIRCLE ( 'NONE', #19547, 0.06509327318403745899 ) ;
#459 = EDGE_CURVE ( 'NONE', #71750, #12146, #88396, .T. ) ;
#458 = CIRCLE ( 'NONE', #33938, 0.06509327318403741736 ) ;
#460 = VERTEX_POINT ( 'NONE', #57679 ) ;
#461 = EDGE_LOOP ( 'NONE', ( #33703, #45194, #92447, #104543 ) ) ;
#462 = EDGE_LOOP ( 'NONE', ( #129077, #120773 ) ) ;
#463 = ORIENTED_EDGE ( 'NONE', *, *, #84900, .F. ) ;
#464 = AXIS2_PLACEMENT_3D ( 'NONE', #93258, #125292, #35627 ) ;
#465 = DIRECTION ( 'NONE',  ( 0.000000000000000000, 0.000000000000000000, 1.000000000000000000 ) ) ;
#466 = AXIS2_PLACEMENT_3D ( 'NONE', #7124, #114506, #105988 ) ;
#467 = FACE_OUTER_BOUND ( 'NONE', #87408, .T. ) ;
#468 = FACE_BOUND ( 'NONE', #114889, .T. ) ;
#469 = CONICAL_SURFACE ( 'NONE', #29740, 0.1000000000000002554, 0.003490658503988666988 ) ;
#470 = CARTESIAN_POINT ( 'NONE',  ( -10.65000000000000391, 2.500000000000000000, -6.841600689897075149 ) ) ;
#471 = EDGE_CURVE ( 'NONE', #91134, #38338, #8544, .T. ) ;
#472 = ORIENTED_EDGE ( 'NONE', *, *, #70105, .F. ) ;
#473 = ADVANCED_FACE ( 'NONE', ( #48493 ), #54362, .T. ) ;
#474 = DIRECTION ( 'NONE',  ( 0.000000000000000000, 0.000000000000000000, 1.000000000000000000 ) ) ;
#475 = CARTESIAN_POINT ( 'NONE',  ( -3.150000000000029221, 12.50000000000000000, -1.753560074763288679 ) ) ;
#476 = EDGE_CURVE ( 'NONE', #72177, #24862, #37399, .T. ) ;
#477 = DIRECTION ( 'NONE',  ( -0.000000000000000000, -1.000000000000000000, -0.000000000000000000 ) ) ;
#478 = ADVANCED_FACE ( 'NONE', ( #128368 ), #106587, .T. ) ;
#479 = CARTESIAN_POINT ( 'NONE',  ( 10.64999999999991331, 12.50000000000000000, 6.906693963081109722 ) ) ;
#480 = EDGE_CURVE ( 'NONE', #103573, #99701, #89867, .T. ) ;
#481 = ORIENTED_EDGE ( 'NONE', *, *, #101011, .F. ) ;
#482 = DIRECTION ( 'NONE',  ( 0.000000000000000000, 0.000000000000000000, 1.000000000000000000 ) ) ;
#483 = ORIENTED_EDGE ( 'NONE', *, *, #114599, .F. ) ;
#484 = ADVANCED_FACE ( 'NONE', ( #29503 ), #71094, .T. ) ;
#485 = ORIENTED_EDGE ( 'NONE', *, *, #39680, .F. ) ;
#486 = CARTESIAN_POINT ( 'NONE',  ( 5.399999999999932854, 12.50000000000000000, 3.637306695894644726 ) ) ;
#487 = EDGE_CURVE ( 'NONE', #113497, #31016, #117032, .T. ) ;
#488 = DIRECTION ( 'NONE',  ( 1.000000000000000000, 0.000000000000000000, 0.000000000000000000 ) ) ;
#489 = ORIENTED_EDGE ( 'NONE', *, *, #128216, .F. ) ;
#490 = EDGE_CURVE ( 'NONE', #118039, #58176, #68770, .T. ) ;
#491 = VECTOR ( 'NONE', #65782, 1000.000000000000000 ) ;
#492 = EDGE_CURVE ( 'NONE', #2276, #21005, #49161, .T. ) ;
#494 = CARTESIAN_POINT ( 'NONE',  ( 1.449999999999952660, 2.500000000000000000, -6.841600689897078702 ) ) ;
#493 = CIRCLE ( 'NONE', #53038, 0.1000000000000000472 ) ;
#495 = EDGE_CURVE ( 'NONE', #48344, #7845, #16425, .T. ) ;
#496 = DIRECTION ( 'NONE',  ( 0.000000000000000000, -0.000000000000000000, 1.000000000000000000 ) ) ;
#497 = CARTESIAN_POINT ( 'NONE',  ( 11.24999999999990941, 2.500000000000000000, -1.472243186433550122 ) ) ;
#498 = EDGE_LOOP ( 'NONE', ( #49269, #78172, #39117, #88604 ) ) ;
#499 = CARTESIAN_POINT ( 'NONE',  ( -15.59999999999998010, 2.500000000000000000, -0.3464101615137759604 ) ) ;
#501 = EDGE_CURVE ( 'NONE', #82957, #8340, #106126, .T. ) ;
#500 = VECTOR ( 'NONE', #4290, 1000.000000000000000 ) ;
#502 = ORIENTED_EDGE ( 'NONE', *, *, #7892, .F. ) ;
#503 = FACE_OUTER_BOUND ( 'NONE', #69667, .T. ) ;
#504 = PRESENTATION_LAYER_ASSIGNMENT (  '', '', ( #56927 ) ) ;
#505 = CIRCLE ( 'NONE', #65349, 0.06509327318403745899 ) ;
#506 = ORIENTED_EDGE ( 'NONE', *, *, #31543, .F. ) ;
#507 = CARTESIAN_POINT ( 'NONE',  ( 108.8430433244084554, 5.913955341756470752, 4.931228954127792719 ) ) ;
#508 = ORIENTED_EDGE ( 'NONE', *, *, #3141, .T. ) ;
#509 = CARTESIAN_POINT ( 'NONE',  ( 9.999999999999912959, 2.500000000000000000, 3.637306695894644726 ) ) ;
#510 = CARTESIAN_POINT ( 'NONE',  ( 0.000000000000000000, 0.000000000000000000, 6.000000000000005329 ) ) ;
#511 = FACE_OUTER_BOUND ( 'NONE', #69854, .T. ) ;
#512 = DIRECTION ( 'NONE',  ( -0.000000000000000000, -1.000000000000000000, -0.000000000000000000 ) ) ;
#513 = DIRECTION ( 'NONE',  ( 0.000000000000000000, -0.9999939076577903929, 0.003490651415223739937 ) ) ;
#514 = CONICAL_SURFACE ( 'NONE', #100868, 0.09999999999999982514, 0.003490658503988666988 ) ;
#515 = VERTEX_POINT ( 'NONE', #96290 ) ;
#516 = ORIENTED_EDGE ( 'NONE', *, *, #84359, .T. ) ;
#517 = AXIS2_PLACEMENT_3D ( 'NONE', #98837, #49774, #89033 ) ;
#518 = ORIENTED_EDGE ( 'NONE', *, *, #80415, .T. ) ;
#519 = DIRECTION ( 'NONE',  ( -0.000000000000000000, -1.000000000000000000, -0.000000000000000000 ) ) ;
#521 = AXIS2_PLACEMENT_3D ( 'NONE', #75882, #85700, #76540 ) ;
#520 = CARTESIAN_POINT ( 'NONE',  ( -13.74999999999995381, 12.50000000000000000, 2.230156782645138946 ) ) ;
#522 = CONICAL_SURFACE ( 'NONE', #17231, 0.09999999999999982514, 0.003490658503988666988 ) ;
#523 = AXIS2_PLACEMENT_3D ( 'NONE', #65391, #34012, #73934 ) ;
#524 = DIRECTION ( 'NONE',  ( 0.000000000000000000, 0.000000000000000000, -1.000000000000000000 ) ) ;
#526 = EDGE_LOOP ( 'NONE', ( #35854, #44819 ) ) ;
#525 = EDGE_LOOP ( 'NONE', ( #12117, #1575, #54740, #85468 ) ) ;
#527 = VERTEX_POINT ( 'NONE', #76672 ) ;
#528 = CARTESIAN_POINT ( 'NONE',  ( -3.550000000000028244, 2.500000000000000000, -1.818653347947326138 ) ) ;
#529 = AXIS2_PLACEMENT_3D ( 'NONE', #111892, #21574, #91601 ) ;
#530 = EDGE_LOOP ( 'NONE', ( #10589, #38123, #90498, #108405 ) ) ;
#531 = CARTESIAN_POINT ( 'NONE',  ( -7.950000000000012612, 2.500000000000000000, -2.165063509461101710 ) ) ;
#532 = CARTESIAN_POINT ( 'NONE',  ( 5.649999999999934630, 12.50000000000000000, -1.753560074763288457 ) ) ;
#533 = CIRCLE ( 'NONE', #113419, 0.06509327318403745899 ) ;
#534 = DIRECTION ( 'NONE',  ( 0.000000000000000000, 1.000000000000000000, 0.000000000000000000 ) ) ;
#535 = CARTESIAN_POINT ( 'NONE',  ( 0.6499999999999561684, 2.500000000000000000, 1.718653347947321386 ) ) ;
#536 = DIRECTION ( 'NONE',  ( -4.274815082592931898E-19, -0.9999939076577903929, -0.003490651415223739937 ) ) ;
#537 = DIRECTION ( 'NONE',  ( -0.000000000000000000, 1.000000000000000000, -0.000000000000000000 ) ) ;
#538 = CARTESIAN_POINT ( 'NONE',  ( -9.600000000000008527, 2.500000000000000000, 4.230127018922196669 ) ) ;
#539 = ORIENTED_EDGE ( 'NONE', *, *, #28756, .T. ) ;
#540 = ORIENTED_EDGE ( 'NONE', *, *, #107770, .T. ) ;
#541 = EDGE_CURVE ( 'NONE', #80023, #53300, #26922, .T. ) ;
#542 = LINE ( 'NONE', #78496, #27793 ) ;
#544 = EDGE_CURVE ( 'NONE', #16388, #101658, #70695, .T. ) ;
#543 = DIRECTION ( 'NONE',  ( 0.000000000000000000, 0.000000000000000000, 1.000000000000000000 ) ) ;
#545 = ORIENTED_EDGE ( 'NONE', *, *, #127066, .T. ) ;
#546 = EDGE_LOOP ( 'NONE', ( #77383, #87063, #10085, #77863 ) ) ;
#547 = AXIS2_PLACEMENT_3D ( 'NONE', #38764, #76725, #29556 ) ;
#548 = CARTESIAN_POINT ( 'NONE',  ( 186.6927083336747160, 6.551208109652275624, -3.782341765624998686 ) ) ;
#549 = CARTESIAN_POINT ( 'NONE',  ( 195.0435778713738557, 0.000000000000000000, 0.000000000000000000 ) ) ;
#550 = CARTESIAN_POINT ( 'NONE',  ( 1.649999999999951061, 2.500000000000000000, -6.595190528383302109 ) ) ;
#551 = EDGE_CURVE ( 'NONE', #109098, #46879, #47726, .T. ) ;
#552 = CARTESIAN_POINT ( 'NONE',  ( -7.100000000000017408, 12.50000000000000000, -3.572213422710612374 ) ) ;
#553 = CARTESIAN_POINT ( 'NONE',  ( 3.549999999999941203, 2.500000000000000000, 6.048780366869521252 ) ) ;
#554 = VECTOR ( 'NONE', #28502, 1000.000000000000000 ) ;
#555 = CARTESIAN_POINT ( 'NONE',  ( 8.349999999999923261, 2.500000000000000000, 2.265063509461097357 ) ) ;
#556 = DIRECTION ( 'NONE',  ( 0.000000000000000000, 1.000000000000000000, 0.000000000000000000 ) ) ;
#557 = AXIS2_PLACEMENT_3D ( 'NONE', #16943, #117096, #120184 ) ;
#558 = DIRECTION ( 'NONE',  ( 0.000000000000000000, -0.9999939076577903929, 0.003490651415223739937 ) ) ;
#559 = ORIENTED_EDGE ( 'NONE', *, *, #67369, .F. ) ;
#560 = ORIENTED_EDGE ( 'NONE', *, *, #7625, .F. ) ;
#561 = CONICAL_SURFACE ( 'NONE', #117524, 0.1000000000000002554, 0.003490658503988666988 ) ;
#562 = AXIS2_PLACEMENT_3D ( 'NONE', #123402, #33740, #23937 ) ;
#563 = ORIENTED_EDGE ( 'NONE', *, *, #110440, .T. ) ;
#564 = CONICAL_SURFACE ( 'NONE', #107172, 0.1000000000000002554, 0.003490658503988666988 ) ;
#565 = CIRCLE ( 'NONE', #115578, 0.1000000000000002554 ) ;
#566 = CIRCLE ( 'NONE', #103280, 0.1000000000000002554 ) ;
#567 = ORIENTED_EDGE ( 'NONE', *, *, #110310, .T. ) ;
#568 = ORIENTED_EDGE ( 'NONE', *, *, #26797, .F. ) ;
#569 = DIRECTION ( 'NONE',  ( -0.000000000000000000, -1.000000000000000000, -0.000000000000000000 ) ) ;
#570 = PLANE ( 'NONE',  #77163 ) ;
#571 = VECTOR ( 'NONE', #102481, 1000.000000000000000 ) ;
#572 = EDGE_LOOP ( 'NONE', ( #97489, #4579, #90813, #4596 ) ) ;
#573 = CARTESIAN_POINT ( 'NONE',  ( -12.29999999999999538, 2.500000000000000000, -0.2464101615137742063 ) ) ;
#574 = CARTESIAN_POINT ( 'NONE',  ( -13.74999999999998934, 2.500000000000000000, -1.372243186433547812 ) ) ;
#575 = DIRECTION ( 'NONE',  ( -0.000000000000000000, -1.000000000000000000, -0.000000000000000000 ) ) ;
#577 = ORIENTED_EDGE ( 'NONE', *, *, #61831, .F. ) ;
#576 = DIRECTION ( 'NONE',  ( -4.274815082592931898E-19, -0.9999939076577903929, -0.003490651415223739937 ) ) ;
#578 = DIRECTION ( 'NONE',  ( 0.000000000000000000, -0.9999939076577903929, 0.003490651415223739937 ) ) ;
#580 = FACE_OUTER_BOUND ( 'NONE', #16545, .T. ) ;
#579 = AXIS2_PLACEMENT_3D ( 'NONE', #38296, #98473, #105739 ) ;
#581 = EDGE_CURVE ( 'NONE', #39745, #108669, #22276, .T. ) ;
#582 = ORIENTED_EDGE ( 'NONE', *, *, #51786, .F. ) ;
#583 = ORIENTED_EDGE ( 'NONE', *, *, #90235, .F. ) ;
#584 = EDGE_LOOP ( 'NONE', ( #71109, #123158, #88532, #32934 ) ) ;
#585 = VERTEX_POINT ( 'NONE', #121096 ) ;
#586 = DIRECTION ( 'NONE',  ( 0.000000000000000000, 0.000000000000000000, 1.000000000000000000 ) ) ;
#588 = CONICAL_SURFACE ( 'NONE', #11049, 0.1000000000000000472, 0.003490658503988666988 ) ;
#587 = DIRECTION ( 'NONE',  ( 0.000000000000000000, 0.000000000000000000, 1.000000000000000000 ) ) ;
#589 = CARTESIAN_POINT ( 'NONE',  ( -5.200000000000020606, 12.50000000000000000, 3.918623584224383727 ) ) ;
#590 = AXIS2_PLACEMENT_3D ( 'NONE', #80178, #48142, #48793 ) ;
#591 = AXIS2_PLACEMENT_3D ( 'NONE', #92415, #42040, #13849 ) ;
#592 = LINE ( 'NONE', #80479, #106664 ) ;
#594 = VERTEX_POINT ( 'NONE', #32094 ) ;
#593 = ADVANCED_FACE ( 'NONE', ( #82479 ), #81179, .T. ) ;
#595 = CARTESIAN_POINT ( 'NONE',  ( -9.150000000000009237, 12.50000000000000000, -7.253104124594885960 ) ) ;
#596 = CARTESIAN_POINT ( 'NONE',  ( 3.299999999999944755, 2.500000000000000000, -2.385244779468109755E-15 ) ) ;
#597 = CARTESIAN_POINT ( 'NONE',  ( -5.200000000000024158, 2.500000000000000000, -4.676537180435977881 ) ) ;
#598 = DIRECTION ( 'NONE',  ( 0.000000000000000000, 0.000000000000000000, -1.000000000000000000 ) ) ;
#599 = EDGE_CURVE ( 'NONE', #33748, #24092, #120865, .T. ) ;
#600 = AXIS2_PLACEMENT_3D ( 'NONE', #87066, #7861, #117807 ) ;
#601 =( GEOMETRIC_REPRESENTATION_CONTEXT ( 3 ) GLOBAL_UNCERTAINTY_ASSIGNED_CONTEXT ( ( #63820 ) ) GLOBAL_UNIT_ASSIGNED_CONTEXT ( ( #82675, #124525, #32940 ) ) REPRESENTATION_CONTEXT ( 'NONE', 'WORKASPACE' ) );
#602 = AXIS2_PLACEMENT_3D ( 'NONE', #96287, #75361, #105484 ) ;
#603 = EDGE_LOOP ( 'NONE', ( #56647, #48064, #112160, #118008 ) ) ;
#604 = CARTESIAN_POINT ( 'NONE',  ( 1.249999999999950262, 2.500000000000000000, 7.188010851410848723 ) ) ;
#605 = AXIS2_PLACEMENT_3D ( 'NONE', #47938, #87833, #127770 ) ;
#606 = EDGE_LOOP ( 'NONE', ( #3129, #48280, #81066, #21095 ) ) ;
#607 = ORIENTED_EDGE ( 'NONE', *, *, #84163, .F. ) ;
#608 = DIRECTION ( 'NONE',  ( 0.000000000000000000, -0.9999939076577903929, 0.003490651415223739937 ) ) ;
#609 = ADVANCED_FACE ( 'NONE', ( #72012 ), #41486, .T. ) ;
#610 = DIRECTION ( 'NONE',  ( -0.000000000000000000, -1.000000000000000000, -0.000000000000000000 ) ) ;
#611 = FACE_BOUND ( 'NONE', #8184, .T. ) ;
#612 = PLANE ( 'NONE',  #122458 ) ;
#614 = DIRECTION ( 'NONE',  ( 0.000000000000000000, 0.000000000000000000, -1.000000000000000000 ) ) ;
#613 = CIRCLE ( 'NONE', #32042, 0.1000000000000002554 ) ;
#615 = CARTESIAN_POINT ( 'NONE',  ( 3.749999999999940492, 12.50000000000000000, 2.857883832488649301 ) ) ;
#616 = CIRCLE ( 'NONE', #6853, 0.1000000000000002554 ) ;
#617 = AXIS2_PLACEMENT_3D ( 'NONE', #75891, #115817, #26158 ) ;
#618 = CIRCLE ( 'NONE', #50816, 0.09999999999999999167 ) ;
#619 = DIRECTION ( 'NONE',  ( 0.000000000000000000, 1.000000000000000000, 0.000000000000000000 ) ) ;
#620 = DIRECTION ( 'NONE',  ( 1.000000000000000000, -0.000000000000000000, -0.000000000000000000 ) ) ;
#621 = CARTESIAN_POINT ( 'NONE',  ( -5.200000000000020606, 12.50000000000000000, 4.048810130592458201 ) ) ;
#622 = AXIS2_PLACEMENT_3D ( 'NONE', #18184, #128829, #30615 ) ;
#623 = DIRECTION ( 'NONE',  ( 0.000000000000000000, 0.000000000000000000, 1.000000000000000000 ) ) ;
#624 = EDGE_LOOP ( 'NONE', ( #73642, #85487, #52293, #4197 ) ) ;
#625 = DIRECTION ( 'NONE',  ( -0.000000000000000000, 1.000000000000000000, -0.000000000000000000 ) ) ;
#626 = CARTESIAN_POINT ( 'NONE',  ( -2.900000000000029221, 2.500000000000000000, -4.330127018922201643 ) ) ;
#627 = AXIS2_PLACEMENT_3D ( 'NONE', #127527, #86948, #126885 ) ;
#628 = ORIENTED_EDGE ( 'NONE', *, *, #14488, .T. ) ;
#629 = ORIENTED_EDGE ( 'NONE', *, *, #82184, .F. ) ;
#630 = CARTESIAN_POINT ( 'NONE',  ( -7.100000000000014744, 2.500000000000000000, 4.330127018922196314 ) ) ;
#631 = DIRECTION ( 'NONE',  ( 0.000000000000000000, 0.000000000000000000, 1.000000000000000000 ) ) ;
#632 = FACE_BOUND ( 'NONE', #122788, .T. ) ;
#633 = CARTESIAN_POINT ( 'NONE',  ( 4.549999999999939426, 12.50000000000000000, -6.430097255199264339 ) ) ;
#634 = EDGE_CURVE ( 'NONE', #85204, #14536, #31021, .T. ) ;
#635 = CARTESIAN_POINT ( 'NONE',  ( -4.350000000000023626, 2.500000000000000000, 1.818653347947321475 ) ) ;
#636 = ORIENTED_EDGE ( 'NONE', *, *, #72588, .T. ) ;
#638 = CIRCLE ( 'NONE', #100889, 0.06509327318403745899 ) ;
#637 = CARTESIAN_POINT ( 'NONE',  ( 184.5000000000000000, 9.429780353434619030E-16, 7.699999999999999289 ) ) ;
#639 = EDGE_CURVE ( 'NONE', #69112, #15707, #102108, .T. ) ;
#640 = FACE_OUTER_BOUND ( 'NONE', #19508, .T. ) ;
#641 = ADVANCED_FACE ( 'NONE', ( #70070 ), #118814, .T. ) ;
#642 = ORIENTED_EDGE ( 'NONE', *, *, #2599, .T. ) ;
#643 = PLANE ( 'NONE',  #15595 ) ;
#644 = CARTESIAN_POINT ( 'NONE',  ( 186.5312500006828031, 9.429780353434619030E-16, -7.700000000000000178 ) ) ;
#645 = CIRCLE ( 'NONE', #119784, 0.06509327318403745899 ) ;
#646 = EDGE_CURVE ( 'NONE', #35702, #96407, #102093, .T. ) ;
#647 = CIRCLE ( 'NONE', #82144, 0.1000000000000002554 ) ;
#648 = EDGE_CURVE ( 'NONE', #68126, #33200, #14251, .T. ) ;
#649 = CARTESIAN_POINT ( 'NONE',  ( -9.150000000000009237, 12.50000000000000000, -7.122917578226811486 ) ) ;
#650 = EDGE_CURVE ( 'NONE', #29270, #9679, #104147, .T. ) ;
#651 = CARTESIAN_POINT ( 'NONE',  ( 12.69999999999989804, 12.50000000000000000, 0.3464101615137735735 ) ) ;
#652 = AXIS2_PLACEMENT_3D ( 'NONE', #68658, #36645, #49043 ) ;
#654 = ORIENTED_EDGE ( 'NONE', *, *, #100999, .T. ) ;
#653 = VECTOR ( 'NONE', #20079, 1000.000000000000000 ) ;
#655 = AXIS2_PLACEMENT_3D ( 'NONE', #129245, #87973, #78193 ) ;
#656 = CARTESIAN_POINT ( 'NONE',  ( -12.69999999999999218, 2.500000000000000000, -4.676537180435975216 ) ) ;
#657 = ADVANCED_FACE ( 'NONE', ( #109342 ), #64432, .T. ) ;
#658 = DIRECTION ( 'NONE',  ( 0.000000000000000000, 0.000000000000000000, 1.000000000000000000 ) ) ;
#659 = PLANE ( 'NONE',  #63936 ) ;
#660 = AXIS2_PLACEMENT_3D ( 'NONE', #121579, #43705, #10965 ) ;
#662 = ORIENTED_EDGE ( 'NONE', *, *, #127719, .F. ) ;
#661 = AXIS2_PLACEMENT_3D ( 'NONE', #47904, #18431, #106796 ) ;
#663 = EDGE_LOOP ( 'NONE', ( #88729, #95449 ) ) ;
#664 = DIRECTION ( 'NONE',  ( -0.000000000000000000, 1.000000000000000000, -0.000000000000000000 ) ) ;
#665 = ADVANCED_FACE ( 'NONE', ( #41271 ), #71337, .T. ) ;
#666 = CONICAL_SURFACE ( 'NONE', #11119, 0.1000000000000002554, 0.003490658503988666988 ) ;
#667 = ORIENTED_EDGE ( 'NONE', *, *, #63347, .F. ) ;
#668 = DIRECTION ( 'NONE',  ( 0.000000000000000000, 0.000000000000000000, -1.000000000000000000 ) ) ;
#669 = FACE_OUTER_BOUND ( 'NONE', #29516, .T. ) ;
#670 = LINE ( 'NONE', #50417, #27795 ) ;
#671 = ORIENTED_EDGE ( 'NONE', *, *, #14169, .F. ) ;
#672 = DIRECTION ( 'NONE',  ( 0.000000000000000000, -0.9999939076577903929, 0.003490651415223739937 ) ) ;
#673 = CARTESIAN_POINT ( 'NONE',  ( 10.84999999999991260, 2.500000000000000000, -2.165063509461101710 ) ) ;
#674 = DIRECTION ( 'NONE',  ( 0.000000000000000000, 0.000000000000000000, 1.000000000000000000 ) ) ;
#675 = PLANE ( 'NONE',  #37128 ) ;
#676 = CARTESIAN_POINT ( 'NONE',  ( 11.89999999999990798, 12.50000000000000000, 4.676537180435972552 ) ) ;
#677 = DIRECTION ( 'NONE',  ( 0.000000000000000000, 1.000000000000000000, 0.000000000000000000 ) ) ;
#678 = CIRCLE ( 'NONE', #52921, 0.09999999999999982514 ) ;
#679 = EDGE_LOOP ( 'NONE', ( #46494, #123936 ) ) ;
#680 = EDGE_LOOP ( 'NONE', ( #77072, #102505 ) ) ;
#681 = FACE_OUTER_BOUND ( 'NONE', #89916, .T. ) ;
#682 = EDGE_LOOP ( 'NONE', ( #37408, #91161 ) ) ;
#683 = DIRECTION ( 'NONE',  ( -0.000000000000000000, -1.000000000000000000, -0.000000000000000000 ) ) ;
#685 = ORIENTED_EDGE ( 'NONE', *, *, #2709, .T. ) ;
#684 = ORIENTED_EDGE ( 'NONE', *, *, #99808, .F. ) ;
#686 = EDGE_LOOP ( 'NONE', ( #115705, #18829, #20205, #100093, #70594, #129048 ) ) ;
#687 = PLANE ( 'NONE',  #43815 ) ;
#688 = AXIS2_PLACEMENT_3D ( 'NONE', #1248, #41199, #81111 ) ;
#689 = AXIS2_PLACEMENT_3D ( 'NONE', #46058, #103692, #13992 ) ;
#690 = DIRECTION ( 'NONE',  ( 0.000000000000000000, -0.9999939076577903929, 0.003490651415223739937 ) ) ;
#691 = AXIS2_PLACEMENT_3D ( 'NONE', #109981, #91413, #73068 ) ;
#692 = DIRECTION ( 'NONE',  ( 0.000000000000000000, 1.000000000000000000, 0.000000000000000000 ) ) ;
#693 = DIRECTION ( 'NONE',  ( 0.000000000000000000, 0.000000000000000000, 1.000000000000000000 ) ) ;
#694 = DIRECTION ( 'NONE',  ( 0.000000000000000000, 0.000000000000000000, 1.000000000000000000 ) ) ;
#695 = CARTESIAN_POINT ( 'NONE',  ( 185.9583333333333144, 4.445597072760159030, 7.699999999999928235 ) ) ;
#696 = CARTESIAN_POINT ( 'NONE',  ( -0.4000000000000404898, 2.500000000000000000, 5.022947341949748790 ) ) ;
#697 = DIRECTION ( 'NONE',  ( -0.000000000000000000, -1.000000000000000000, -0.000000000000000000 ) ) ;
#698 = CIRCLE ( 'NONE', #115711, 0.1000000000000002554 ) ;
#699 = CONICAL_SURFACE ( 'NONE', #23694, 0.1000000000000002554, 0.003490658503988666988 ) ;
#700 = PLANE ( 'NONE',  #114607 ) ;
#701 = CIRCLE ( 'NONE', #124037, 0.06509327318403745899 ) ;
#702 = VERTEX_POINT ( 'NONE', #42561 ) ;
#703 = AXIS2_PLACEMENT_3D ( 'NONE', #90090, #21364, #80944 ) ;
#704 = EDGE_CURVE ( 'NONE', #22628, #35194, #74910, .T. ) ;
#705 = FACE_OUTER_BOUND ( 'NONE', #8845, .T. ) ;
#706 = ORIENTED_EDGE ( 'NONE', *, *, #56081, .F. ) ;
#707 = EDGE_LOOP ( 'NONE', ( #52225, #86557 ) ) ;
#708 = CARTESIAN_POINT ( 'NONE',  ( -9.350000000000004974, 2.500000000000000000, 6.841600689897072485 ) ) ;
#709 = AXIS2_PLACEMENT_3D ( 'NONE', #109330, #19668, #66810 ) ;
#710 = PLANE ( 'NONE',  #109123 ) ;
#711 = ADVANCED_FACE ( 'NONE', ( #60886 ), #91621, .T. ) ;
#712 = CARTESIAN_POINT ( 'NONE',  ( 186.8229166673494603, -4.445597072760107515, 7.700000000000023270 ) ) ;
#713 = CARTESIAN_POINT ( 'NONE',  ( 4.549999999999939426, 12.50000000000000000, -2.230156782645139391 ) ) ;
#714 = AXIS2_PLACEMENT_3D ( 'NONE', #88680, #120083, #118780 ) ;
#715 = DIRECTION ( 'NONE',  ( 0.000000000000000000, 1.000000000000000000, 0.000000000000000000 ) ) ;
#716 = CIRCLE ( 'NONE', #2872, 0.06509327318403745899 ) ;
#717 = CARTESIAN_POINT ( 'NONE',  ( -13.94999999999998685, 2.500000000000000000, 1.918653347947325338 ) ) ;
#718 = ORIENTED_EDGE ( 'NONE', *, *, #25746, .T. ) ;
#719 = AXIS2_PLACEMENT_3D ( 'NONE', #63117, #13369, #50723 ) ;
#720 = ORIENTED_EDGE ( 'NONE', *, *, #108181, .T. ) ;
#721 = CARTESIAN_POINT ( 'NONE',  ( 3.349999999999945466, 2.500000000000000000, -7.188010851410854052 ) ) ;
#722 = ORIENTED_EDGE ( 'NONE', *, *, #47754, .T. ) ;
#723 = DIRECTION ( 'NONE',  ( -0.000000000000000000, -1.000000000000000000, -0.000000000000000000 ) ) ;
#724 = ORIENTED_EDGE ( 'NONE', *, *, #22817, .T. ) ;
#725 = ORIENTED_EDGE ( 'NONE', *, *, #32189, .T. ) ;
#726 = FACE_OUTER_BOUND ( 'NONE', #107954, .T. ) ;
#727 = CARTESIAN_POINT ( 'NONE',  ( 21.23528140090950700, -2.699413673072311948, -2.293764360948876480 ) ) ;
#728 = CARTESIAN_POINT ( 'NONE',  ( 11.04999999999991012, 12.50000000000000000, -1.753560074763288679 ) ) ;
#729 = DIRECTION ( 'NONE',  ( 0.000000000000000000, 1.000000000000000000, 0.000000000000000000 ) ) ;
#730 = CARTESIAN_POINT ( 'NONE',  ( 17.50000000000000000, 2.083333333333332593, 4.000000000000000000 ) ) ;
#731 = ORIENTED_EDGE ( 'NONE', *, *, #47779, .F. ) ;
#732 = DIRECTION ( 'NONE',  ( 0.000000000000000000, -0.9999939076577903929, 0.003490651415223739937 ) ) ;
#734 = AXIS2_PLACEMENT_3D ( 'NONE', #117084, #126934, #27414 ) ;
#733 = DIRECTION ( 'NONE',  ( 0.000000000000000000, -0.9999939076577903929, 0.003490651415223739937 ) ) ;
#735 = AXIS2_PLACEMENT_3D ( 'NONE', #18059, #116896, #17403 ) ;
#736 = DIRECTION ( 'NONE',  ( 0.000000000000000000, 0.000000000000000000, 1.000000000000000000 ) ) ;
#737 = LINE ( 'NONE', #40701, #109967 ) ;
#738 = DIRECTION ( 'NONE',  ( 0.000000000000000000, -0.9999939076577903929, 0.003490651415223739937 ) ) ;
#739 = EDGE_CURVE ( 'NONE', #98477, #23899, #10067, .T. ) ;
#740 = VERTEX_POINT ( 'NONE', #49801 ) ;
#741 = CONICAL_SURFACE ( 'NONE', #119881, 0.1000000000000002554, 0.003490658503988666988 ) ;
#742 = ORIENTED_EDGE ( 'NONE', *, *, #43010, .F. ) ;
#743 = AXIS2_PLACEMENT_3D ( 'NONE', #53506, #3744, #21453 ) ;
#744 = VECTOR ( 'NONE', #21845, 1000.000000000000000 ) ;
#745 = CARTESIAN_POINT ( 'NONE',  ( 12.29999999999990656, 2.500000000000000000, 4.083716857408421497 ) ) ;
#746 = ORIENTED_EDGE ( 'NONE', *, *, #80621, .T. ) ;
#747 = CARTESIAN_POINT ( 'NONE',  ( 1.049999999999952971, 2.500000000000000000, 6.148780366869520897 ) ) ;
#749 = EDGE_CURVE ( 'NONE', #15903, #100174, #108344, .T. ) ;
#748 = DIRECTION ( 'NONE',  ( 0.000000000000000000, 0.000000000000000000, 1.000000000000000000 ) ) ;
#750 = CIRCLE ( 'NONE', #90638, 0.09999999999999982514 ) ;
#751 = CONICAL_SURFACE ( 'NONE', #73913, 0.09999999999999999167, 0.003490658503988666988 ) ;
#752 = CIRCLE ( 'NONE', #82443, 0.09999999999999982514 ) ;
#753 = AXIS2_PLACEMENT_3D ( 'NONE', #109386, #92317, #2000 ) ;
#755 = EDGE_LOOP ( 'NONE', ( #13923, #69922 ) ) ;
#754 = ADVANCED_FACE ( 'NONE', ( #62828 ), #122939, .T. ) ;
#756 = DIRECTION ( 'NONE',  ( -0.000000000000000000, 1.000000000000000000, -0.000000000000000000 ) ) ;
#757 = FACE_OUTER_BOUND ( 'NONE', #96203, .T. ) ;
#758 = FACE_OUTER_BOUND ( 'NONE', #31325, .T. ) ;
#759 = ADVANCED_FACE ( 'NONE', ( #5814 ), #45670, .T. ) ;
#760 = DIRECTION ( 'NONE',  ( 0.000000000000000000, 0.000000000000000000, 1.000000000000000000 ) ) ;
#761 = FACE_OUTER_BOUND ( 'NONE', #38545, .T. ) ;
#762 = EDGE_CURVE ( 'NONE', #24428, #9737, #115114, .T. ) ;
#763 = ORIENTED_EDGE ( 'NONE', *, *, #42656, .T. ) ;
#764 = EDGE_CURVE ( 'NONE', #127196, #103587, #43532, .T. ) ;
#765 = CARTESIAN_POINT ( 'NONE',  ( -1.650000000000034772, 2.500000000000000000, 6.395190528383296602 ) ) ;
#766 = FACE_OUTER_BOUND ( 'NONE', #35567, .T. ) ;
#767 = CARTESIAN_POINT ( 'NONE',  ( -13.09999999999999254, 2.500000000000000000, -4.083716857408424161 ) ) ;
#768 = AXIS2_PLACEMENT_3D ( 'NONE', #63578, #93039, #112031 ) ;
#769 = CARTESIAN_POINT ( 'NONE',  ( -4.550000000000022915, 12.50000000000000000, 6.430097255199259010 ) ) ;
#770 = EDGE_LOOP ( 'NONE', ( #91474, #18313 ) ) ;
#771 = EDGE_LOOP ( 'NONE', ( #4054, #86586, #92861, #126394 ) ) ;
#772 = FACE_OUTER_BOUND ( 'NONE', #113605, .T. ) ;
#773 = CARTESIAN_POINT ( 'NONE',  ( -1.250000000000001110, 12.50000000000000000, -2.230156782645139391 ) ) ;
#774 = LINE ( 'NONE', #119915, #1580 ) ;
#775 = AXIS2_PLACEMENT_3D ( 'NONE', #126173, #107164, #7020 ) ;
#776 = VERTEX_POINT ( 'NONE', #34676 ) ;
#777 = VECTOR ( 'NONE', #12550, 1000.000000000000000 ) ;
#778 = CIRCLE ( 'NONE', #90671, 0.1000000000000002554 ) ;
#779 = DIRECTION ( 'NONE',  ( -0.000000000000000000, 1.000000000000000000, -0.000000000000000000 ) ) ;
#780 = CARTESIAN_POINT ( 'NONE',  ( 4.999999999999938716, 2.500000000000000000, -5.022947341949754119 ) ) ;
#781 = VERTEX_POINT ( 'NONE', #43204 ) ;
#782 = CARTESIAN_POINT ( 'NONE',  ( -9.150000000000009237, 12.50000000000000000, -1.407149913249512663 ) ) ;
#783 = VECTOR ( 'NONE', #10300, 1000.000000000000000 ) ;
#784 = ORIENTED_EDGE ( 'NONE', *, *, #22311, .F. ) ;
#785 = AXIS2_PLACEMENT_3D ( 'NONE', #25187, #6184, #3623 ) ;
#786 = CARTESIAN_POINT ( 'NONE',  ( 8.099999999999923261, 2.500000000000000000, -4.676537180435978769 ) ) ;
#787 = VECTOR ( 'NONE', #9613, 1000.000000000000000 ) ;
#788 = ADVANCED_FACE ( 'NONE', ( #54924 ), #83121, .T. ) ;
#789 = ORIENTED_EDGE ( 'NONE', *, *, #47381, .F. ) ;
#790 = DIRECTION ( 'NONE',  ( -0.000000000000000000, -1.000000000000000000, -0.000000000000000000 ) ) ;
#791 = CARTESIAN_POINT ( 'NONE',  ( 3.677964504776914723, 2.499999999999999112, -8.999999999999996447 ) ) ;
#792 = ORIENTED_EDGE ( 'NONE', *, *, #103180, .T. ) ;
#793 = ORIENTED_EDGE ( 'NONE', *, *, #120546, .F. ) ;
#794 = EDGE_CURVE ( 'NONE', #29548, #67957, #37265, .T. ) ;
#795 = VECTOR ( 'NONE', #27229, 1000.000000000000000 ) ;
#796 = CARTESIAN_POINT ( 'NONE',  ( 3.949999999999938005, 2.500000000000000000, 6.841600689897072485 ) ) ;
#797 = DIRECTION ( 'NONE',  ( 0.000000000000000000, -1.000000000000000000, 0.000000000000000000 ) ) ;
#798 = ORIENTED_EDGE ( 'NONE', *, *, #111103, .F. ) ;
#799 = EDGE_CURVE ( 'NONE', #50587, #11702, #35310, .T. ) ;
#800 = CARTESIAN_POINT ( 'NONE',  ( 185.5833333333333144, -6.668395609140180369, 3.849999999999994760 ) ) ;
#801 = CARTESIAN_POINT ( 'NONE',  ( 10.64999999999990976, 2.500000000000000000, -6.841600689897077814 ) ) ;
#802 = CIRCLE ( 'NONE', #73974, 0.06509327318403745899 ) ;
#803 = DIRECTION ( 'NONE',  ( 0.000000000000000000, 0.000000000000000000, 1.000000000000000000 ) ) ;
#804 = CONICAL_SURFACE ( 'NONE', #21660, 0.1000000000000000472, 0.003490658503988666988 ) ;
#805 = CARTESIAN_POINT ( 'NONE',  ( 103.6746308345937422, 8.329113074144254725, -2.529173134518388544 ) ) ;
#806 = CARTESIAN_POINT ( 'NONE',  ( -12.09999999999999609, 12.50000000000000000, -0.6928203230275501445 ) ) ;
#807 = EDGE_CURVE ( 'NONE', #38593, #8229, #116661, .T. ) ;
#808 = CARTESIAN_POINT ( 'NONE',  ( 7.899999999999924860, 2.500000000000000000, 4.330127018922196314 ) ) ;
#809 = AXIS2_PLACEMENT_3D ( 'NONE', #65694, #5470, #6118 ) ;
#810 = FACE_OUTER_BOUND ( 'NONE', #5290, .T. ) ;
#811 = EDGE_CURVE ( 'NONE', #122569, #115231, #52448, .T. ) ;
#812 = EDGE_CURVE ( 'NONE', #65686, #2207, #23202, .T. ) ;
#813 = CIRCLE ( 'NONE', #90706, 0.1000000000000002554 ) ;
#814 = ORIENTED_EDGE ( 'NONE', *, *, #96816, .F. ) ;
#815 = ORIENTED_EDGE ( 'NONE', *, *, #44054, .T. ) ;
#816 = EDGE_CURVE ( 'NONE', #96927, #17385, #73280, .T. ) ;
#817 = ORIENTED_EDGE ( 'NONE', *, *, #54697, .T. ) ;
#818 = DIRECTION ( 'NONE',  ( 0.000000000000000000, 0.000000000000000000, 1.000000000000000000 ) ) ;
#819 = PLANE ( 'NONE',  #11518 ) ;
#820 = DIRECTION ( 'NONE',  ( 0.000000000000000000, 1.000000000000000000, 0.000000000000000000 ) ) ;
#822 = ORIENTED_EDGE ( 'NONE', *, *, #76466, .F. ) ;
#821 = ORIENTED_EDGE ( 'NONE', *, *, #89628, .T. ) ;
#823 = FACE_BOUND ( 'NONE', #115451, .T. ) ;
#824 = ORIENTED_EDGE ( 'NONE', *, *, #54300, .F. ) ;
#825 = DIRECTION ( 'NONE',  ( -0.000000000000000000, 1.000000000000000000, -0.000000000000000000 ) ) ;
#826 = DIRECTION ( 'NONE',  ( 0.000000000000000000, 0.000000000000000000, -1.000000000000000000 ) ) ;
#827 = EDGE_CURVE ( 'NONE', #45964, #73617, #113863, .T. ) ;
#828 = CARTESIAN_POINT ( 'NONE',  ( -7.500000000000015099, 12.50000000000000000, -5.022947341949754119 ) ) ;
#830 = EDGE_CURVE ( 'NONE', #63242, #121356, #72655, .T. ) ;
#829 = DIRECTION ( 'NONE',  ( 0.000000000000000000, 0.000000000000000000, 1.000000000000000000 ) ) ;
#831 = CARTESIAN_POINT ( 'NONE',  ( 6.849999999999929479, 2.500000000000000000, 6.841600689897072485 ) ) ;
#832 = DIRECTION ( 'NONE',  ( -0.000000000000000000, 1.000000000000000000, -0.000000000000000000 ) ) ;
#833 = FACE_OUTER_BOUND ( 'NONE', #13489, .T. ) ;
#834 = CARTESIAN_POINT ( 'NONE',  ( 11.44999999999990870, 2.500000000000000000, 6.741600689897071952 ) ) ;
#835 = AXIS2_PLACEMENT_3D ( 'NONE', #53529, #43086, #101340 ) ;
#836 = CIRCLE ( 'NONE', #2896, 0.06509327318403745899 ) ;
#837 = CARTESIAN_POINT ( 'NONE',  ( -10.85000000000000142, 2.500000000000000000, 6.495190528383297135 ) ) ;
#838 = CARTESIAN_POINT ( 'NONE',  ( 0.8499999999999557909, 2.500000000000000000, -7.088010851410853519 ) ) ;
#839 = CIRCLE ( 'NONE', #38428, 0.1000000000000002554 ) ;
#840 = EDGE_LOOP ( 'NONE', ( #98615, #3304 ) ) ;
#841 = EDGE_LOOP ( 'NONE', ( #59112, #57960 ) ) ;
#842 = ORIENTED_EDGE ( 'NONE', *, *, #93315, .F. ) ;
#843 = AXIS2_PLACEMENT_3D ( 'NONE', #119388, #6837, #18621 ) ;
#844 = VERTEX_POINT ( 'NONE', #113198 ) ;
#846 = CIRCLE ( 'NONE', #74008, 0.1000000000000002554 ) ;
#845 = DIRECTION ( 'NONE',  ( 0.000000000000000000, -0.9999939076577903929, 0.003490651415223739937 ) ) ;
#847 = DIRECTION ( 'NONE',  ( 0.000000000000000000, -0.000000000000000000, 1.000000000000000000 ) ) ;
#849 = ORIENTED_EDGE ( 'NONE', *, *, #54920, .F. ) ;
#848 = EDGE_LOOP ( 'NONE', ( #80324, #87937, #52019, #60747 ) ) ;
#850 = VERTEX_POINT ( 'NONE', #54290 ) ;
#851 = DIRECTION ( 'NONE',  ( 0.000000000000000000, 0.000000000000000000, -1.000000000000000000 ) ) ;
#852 = CIRCLE ( 'NONE', #28042, 0.06509327318403745899 ) ;
#853 = AXIS2_PLACEMENT_3D ( 'NONE', #56388, #105508, #86495 ) ;
#854 = VECTOR ( 'NONE', #29476, 1000.000000000000000 ) ;
#855 = DIRECTION ( 'NONE',  ( 0.000000000000000000, 0.000000000000000000, -1.000000000000000000 ) ) ;
#856 = CARTESIAN_POINT ( 'NONE',  ( 6.449999999999931788, 2.500000000000000000, -2.411473670974877859 ) ) ;
#857 = LINE ( 'NONE', #20508, #66802 ) ;
#858 = DIRECTION ( 'NONE',  ( -0.000000000000000000, 1.000000000000000000, -0.000000000000000000 ) ) ;
#859 = DIRECTION ( 'NONE',  ( 0.000000000000000000, 0.000000000000000000, -1.000000000000000000 ) ) ;
#860 = AXIS2_PLACEMENT_3D ( 'NONE', #49692, #9095, #71903 ) ;
#861 = CARTESIAN_POINT ( 'NONE',  ( -6.650000000000014566, 2.500000000000000000, 1.372243186433545370 ) ) ;
#862 = EDGE_CURVE ( 'NONE', #68242, #18421, #106821, .T. ) ;
#863 = ORIENTED_EDGE ( 'NONE', *, *, #58832, .F. ) ;
#864 = FACE_OUTER_BOUND ( 'NONE', #76237, .T. ) ;
#865 = ORIENTED_EDGE ( 'NONE', *, *, #82965, .F. ) ;
#866 = ORIENTED_EDGE ( 'NONE', *, *, #8700, .T. ) ;
#867 = EDGE_CURVE ( 'NONE', #70717, #56812, #94301, .T. ) ;
#868 = VERTEX_POINT ( 'NONE', #103399 ) ;
#869 = CONICAL_SURFACE ( 'NONE', #90748, 0.1000000000000002554, 0.003490658503988666988 ) ;
#870 = FACE_OUTER_BOUND ( 'NONE', #102181, .T. ) ;
#871 =( BOUNDED_CURVE ( )  B_SPLINE_CURVE ( 2, ( #122989, #65333, #24143, #44418, #5760, #82436, #64062, #74530, #103993, #54246, #62787, #122352, #72603, #114441, #14300, #84347, #124279, #24787, #64699, #104620, #14922, #13000, #92895, #54872, #98660, #115730, #8351, #126205, #117004, #47654, #97383, #18820, #27336, #35892, #108489, #98027, #46344, #118313, #127501, #26719, #106553, #75801, #26080, #58758, #86258, #87556, #37194, #65989, #16856, #16225, #45722, #48292, #68564, #85630, #37824, #125549, #105924, #58122, #56160, #28661, #36556, #96095, #6393, #56790, #78416, #28006, #76467, #67243, #77727, #116371, #86913, #107199, #77108, #66628, #117642, #96726, #7054, #47014, #67923, #38495, #126857, #17525, #107850, #57473, #7702 ),
 .UNSPECIFIED., .F., .F. ) 
 B_SPLINE_CURVE_WITH_KNOTS ( ( 3, 2, 2, 2, 2, 2, 2, 2, 2, 2, 2, 2, 2, 2, 2, 2, 2, 2, 2, 2, 2, 2, 2, 2, 2, 2, 2, 2, 2, 2, 2, 2, 2, 2, 2, 2, 2, 2, 2, 2, 2, 2, 3 ),
 ( 0.000000000000000000, 0.02380952380952380820, 0.04761904761904761640, 0.07142857142857142461, 0.09523809523809523281, 0.1190476190476190410, 0.1428571428571428492, 0.1666666666666666574, 0.1904761904761904656, 0.2142857142857142738, 0.2380952380952380820, 0.2619047619047619180, 0.2857142857142856984, 0.3095238095238095344, 0.3333333333333333148, 0.3571428571428571508, 0.3809523809523809312, 0.4047619047619047672, 0.4285714285714285476, 0.4523809523809523836, 0.4761904761904761640, 0.5000000000000000000, 0.5238095238095238360, 0.5476190476190476719, 0.5714285714285713969, 0.5952380952380952328, 0.6190476190476190688, 0.6428571428571429047, 0.6666666666666666297, 0.6904761904761904656, 0.7142857142857143016, 0.7380952380952381375, 0.7619047619047618625, 0.7857142857142856984, 0.8095238095238095344, 0.8333333333333333703, 0.8571428571428570953, 0.8809523809523809312, 0.9047619047619047672, 0.9285714285714286031, 0.9523809523809523281, 0.9761904761904761640, 1.000000000000000000 ),
 .UNSPECIFIED. ) 
 CURVE ( )  GEOMETRIC_REPRESENTATION_ITEM ( )  RATIONAL_B_SPLINE_CURVE ( ( 1.000000000000000000, 0.8660254037844387076, 1.000000000000000000, 0.8660254037844387076, 1.000000000000000000, 0.8660254037844387076, 1.000000000000000000, 0.8660254037844387076, 1.000000000000000000, 0.8660254037844387076, 1.000000000000000000, 0.8660254037844387076, 1.000000000000000000, 0.8660254037844387076, 1.000000000000000000, 0.8660254037844387076, 1.000000000000000000, 0.8660254037844387076, 1.000000000000000000, 0.8660254037844387076, 1.000000000000000000, 0.8660254037844387076, 1.000000000000000000, 0.8660254037844387076, 1.000000000000000000, 0.8660254037844387076, 1.000000000000000000, 0.8660254037844387076, 1.000000000000000000, 0.8660254037844387076, 1.000000000000000000, 0.8660254037844387076, 1.000000000000000000, 0.8660254037844387076, 1.000000000000000000, 0.8660254037844387076, 1.000000000000000000, 0.8660254037844387076, 1.000000000000000000, 0.8660254037844387076, 1.000000000000000000, 0.8660254037844387076, 1.000000000000000000, 0.8660254037844387076, 1.000000000000000000, 0.8660254037844387076, 1.000000000000000000, 0.8660254037844387076, 1.000000000000000000, 0.8660254037844387076, 1.000000000000000000, 0.8660254037844387076, 1.000000000000000000, 0.8660254037844387076, 1.000000000000000000, 0.8660254037844387076, 1.000000000000000000, 0.8660254037844387076, 1.000000000000000000, 0.8660254037844387076, 1.000000000000000000, 0.8660254037844387076, 1.000000000000000000, 0.8660254037844387076, 1.000000000000000000, 0.8660254037844387076, 1.000000000000000000, 0.8660254037844387076, 1.000000000000000000, 0.8660254037844387076, 1.000000000000000000, 0.8660254037844387076, 1.000000000000000000, 0.8660254037844387076, 1.000000000000000000, 0.8660254037844387076, 1.000000000000000000, 0.8660254037844387076, 1.000000000000000000, 0.8660254037844387076, 1.000000000000000000, 0.8660254037844387076, 1.000000000000000000, 0.8660254037844387076, 1.000000000000000000 ) ) 
 REPRESENTATION_ITEM ( '' )  );
#872 = ORIENTED_EDGE ( 'NONE', *, *, #43821, .T. ) ;
#873 = EDGE_LOOP ( 'NONE', ( #111150, #114806, #127248, #113031 ) ) ;
#874 = ORIENTED_EDGE ( 'NONE', *, *, #56407, .T. ) ;
#875 = AXIS2_PLACEMENT_3D ( 'NONE', #27933, #16153, #45657 ) ;
#876 = CARTESIAN_POINT ( 'NONE',  ( 4.349999999999940137, 2.500000000000000000, -6.741600689897078169 ) ) ;
#877 = EDGE_CURVE ( 'NONE', #50948, #78678, #39949, .T. ) ;
#878 = DIRECTION ( 'NONE',  ( -0.000000000000000000, -1.000000000000000000, -0.000000000000000000 ) ) ;
#879 = DIRECTION ( 'NONE',  ( -4.274815082592931898E-19, -0.9999939076577903929, -0.003490651415223739937 ) ) ;
#880 = CARTESIAN_POINT ( 'NONE',  ( 12.49999999999993960, 2.500000000000000000, -4.330127018922201643 ) ) ;
#881 = DIRECTION ( 'NONE',  ( -0.000000000000000000, -1.000000000000000000, -0.000000000000000000 ) ) ;
#882 = DIRECTION ( 'NONE',  ( 0.000000000000000000, 0.000000000000000000, 1.000000000000000000 ) ) ;
#883 = DIRECTION ( 'NONE',  ( 0.000000000000000000, 0.000000000000000000, -1.000000000000000000 ) ) ;
#884 = CIRCLE ( 'NONE', #4973, 0.09999999999999982514 ) ;
#885 = VERTEX_POINT ( 'NONE', #22909 ) ;
#886 = CARTESIAN_POINT ( 'NONE',  ( -2.100000000000033396, 12.50000000000000000, 0.7579135962115869374 ) ) ;
#887 = ORIENTED_EDGE ( 'NONE', *, *, #7825, .F. ) ;
#888 = CARTESIAN_POINT ( 'NONE',  ( 111.9626685488627942, 8.146665828590855085, 3.066327037116900023 ) ) ;
#889 = CARTESIAN_POINT ( 'NONE',  ( 6.249999999999930722, 2.500000000000000000, 7.088010851410848190 ) ) ;
#890 = VERTEX_POINT ( 'NONE', #3895 ) ;
#891 = CARTESIAN_POINT ( 'NONE',  ( 13.29999999999990301, 2.500000000000000000, 4.230127018922196669 ) ) ;
#892 = DIRECTION ( 'NONE',  ( 0.000000000000000000, 0.000000000000000000, -1.000000000000000000 ) ) ;
#893 = ORIENTED_EDGE ( 'NONE', *, *, #26645, .T. ) ;
#894 = AXIS2_PLACEMENT_3D ( 'NONE', #69015, #31684, #11389 ) ;
#895 = DIRECTION ( 'NONE',  ( -0.000000000000000000, -1.000000000000000000, -0.000000000000000000 ) ) ;
#896 = VERTEX_POINT ( 'NONE', #13049 ) ;
#897 = ORIENTED_EDGE ( 'NONE', *, *, #96445, .F. ) ;
#898 = DIRECTION ( 'NONE',  ( 0.000000000000000000, 0.000000000000000000, -1.000000000000000000 ) ) ;
#899 = CARTESIAN_POINT ( 'NONE',  ( -9.150000000000005684, 12.50000000000000000, 5.737276932171707422 ) ) ;
#900 = CARTESIAN_POINT ( 'NONE',  ( -6.850000000000013856, 2.500000000000000000, 2.411473670974873862 ) ) ;
#901 = DIRECTION ( 'NONE',  ( 0.000000000000000000, -0.9999939076577903929, 0.003490651415223739937 ) ) ;
#902 = CARTESIAN_POINT ( 'NONE',  ( -12.29999999999999361, 2.500000000000000000, 4.083716857408420609 ) ) ;
#903 = ORIENTED_EDGE ( 'NONE', *, *, #37923, .T. ) ;
#904 = AXIS2_PLACEMENT_3D ( 'NONE', #50770, #39687, #101161 ) ;
#905 = CARTESIAN_POINT ( 'NONE',  ( -7.100000000000017408, 2.500000000000000000, -3.537306695894649966 ) ) ;
#906 = VECTOR ( 'NONE', #123801, 1000.000000000000000 ) ;
#907 = VERTEX_POINT ( 'NONE', #43851 ) ;
#908 = AXIS2_PLACEMENT_3D ( 'NONE', #39778, #99970, #59420 ) ;
#909 = CARTESIAN_POINT ( 'NONE',  ( -2.300000000000033573, 12.50000000000000000, 0.3464101615137735735 ) ) ;
#911 = EDGE_CURVE ( 'NONE', #33867, #20692, #45126, .T. ) ;
#910 = CARTESIAN_POINT ( 'NONE',  ( -12.89999999999999147, 12.50000000000000000, -4.330127018922198978 ) ) ;
#912 = EDGE_CURVE ( 'NONE', #19872, #5682, #21151, .T. ) ;
#913 = EDGE_CURVE ( 'NONE', #12403, #70927, #57523, .T. ) ;
#914 = DIRECTION ( 'NONE',  ( -0.000000000000000000, -1.000000000000000000, -0.000000000000000000 ) ) ;
#915 = DIRECTION ( 'NONE',  ( 0.000000000000000000, 0.000000000000000000, 1.000000000000000000 ) ) ;
#916 = CARTESIAN_POINT ( 'NONE',  ( 9.149999999999920419, 12.50000000000000000, -7.188010851410854052 ) ) ;
#917 = CYLINDRICAL_SURFACE ( 'NONE', #50212, 0.5000000000000000000 ) ;
#918 = ADVANCED_FACE ( 'NONE', ( #56211 ), #90091, .T. ) ;
#919 = DIRECTION ( 'NONE',  ( -0.000000000000000000, 1.000000000000000000, -0.000000000000000000 ) ) ;
#920 = ORIENTED_EDGE ( 'NONE', *, *, #122375, .T. ) ;
#921 = CARTESIAN_POINT ( 'NONE',  ( 184.2916666666666856, 4.445597072760049784, -7.700000000000123634 ) ) ;
#923 = DIRECTION ( 'NONE',  ( -0.000000000000000000, 1.000000000000000000, -0.000000000000000000 ) ) ;
#922 = AXIS2_PLACEMENT_3D ( 'NONE', #51766, #120500, #81225 ) ;
#924 = DIRECTION ( 'NONE',  ( 0.000000000000000000, 0.000000000000000000, 1.000000000000000000 ) ) ;
#925 = ADVANCED_FACE ( 'NONE', ( #77779 ), #67090, .T. ) ;
#926 = VECTOR ( 'NONE', #84922, 1000.000000000000000 ) ;
#927 = EDGE_CURVE ( 'NONE', #8077, #54326, #77574, .T. ) ;
#928 = CONICAL_SURFACE ( 'NONE', #59441, 0.1000000000000002554, 0.003490658503988666988 ) ;
#929 = CIRCLE ( 'NONE', #99137, 0.1000000000000002554 ) ;
#930 = ADVANCED_FACE ( 'NONE', ( #36609 ), #113094, .T. ) ;
#931 = EDGE_LOOP ( 'NONE', ( #99662, #13541, #5965, #64093 ) ) ;
#932 = CARTESIAN_POINT ( 'NONE',  ( -1.050000000000038680, 2.500000000000000000, 6.841600689897072485 ) ) ;
#933 = AXIS2_PLACEMENT_3D ( 'NONE', #28967, #119255, #53600 ) ;
#934 = AXIS2_PLACEMENT_3D ( 'NONE', #92141, #51598, #2459 ) ;
#935 = VERTEX_POINT ( 'NONE', #86970 ) ;
#936 = AXIS2_PLACEMENT_3D ( 'NONE', #25174, #95863, #96481 ) ;
#937 = ORIENTED_EDGE ( 'NONE', *, *, #15718, .T. ) ;
#938 = CARTESIAN_POINT ( 'NONE',  ( -5.400000000000019895, 2.500000000000000000, -0.1000000000000022815 ) ) ;
#939 = ORIENTED_EDGE ( 'NONE', *, *, #27834, .T. ) ;
#940 = DIRECTION ( 'NONE',  ( -0.000000000000000000, -1.000000000000000000, -0.000000000000000000 ) ) ;
#941 = DIRECTION ( 'NONE',  ( -0.000000000000000000, 1.000000000000000000, -0.000000000000000000 ) ) ;
#942 = VERTEX_POINT ( 'NONE', #107897 ) ;
#943 = CIRCLE ( 'NONE', #59460, 0.06509327318403745899 ) ;
#944 = AXIS2_PLACEMENT_3D ( 'NONE', #66648, #73902, #113841 ) ;
#945 = DIRECTION ( 'NONE',  ( 0.000000000000000000, 0.000000000000000000, 1.000000000000000000 ) ) ;
#946 = DIRECTION ( 'NONE',  ( 0.000000000000000000, 0.000000000000000000, 1.000000000000000000 ) ) ;
#947 = CARTESIAN_POINT ( 'NONE',  ( 6.649999999999930189, 2.500000000000000000, 7.188010851410848723 ) ) ;
#948 = VERTEX_POINT ( 'NONE', #118360 ) ;
#949 = VERTEX_POINT ( 'NONE', #77156 ) ;
#950 = ORIENTED_EDGE ( 'NONE', *, *, #128216, .T. ) ;
#951 = FACE_OUTER_BOUND ( 'NONE', #103034, .T. ) ;
#952 = FACE_OUTER_BOUND ( 'NONE', #45269, .T. ) ;
#953 = FACE_BOUND ( 'NONE', #20794, .T. ) ;
#954 = ORIENTED_EDGE ( 'NONE', *, *, #127003, .F. ) ;
#955 = DIRECTION ( 'NONE',  ( 0.000000000000000000, 1.000000000000000000, 0.000000000000000000 ) ) ;
#956 = LINE ( 'NONE', #120732, #100379 ) ;
#957 = AXIS2_PLACEMENT_3D ( 'NONE', #47353, #106264, #5468 ) ;
#958 = ORIENTED_EDGE ( 'NONE', *, *, #56440, .F. ) ;
#959 = DIRECTION ( 'NONE',  ( -0.000000000000000000, 1.000000000000000000, -0.000000000000000000 ) ) ;
#960 = DIRECTION ( 'NONE',  ( -0.000000000000000000, 1.000000000000000000, -0.000000000000000000 ) ) ;
#962 = ADVANCED_FACE ( 'NONE', ( #75850 ), #18220, .T. ) ;
#961 = FACE_OUTER_BOUND ( 'NONE', #54640, .T. ) ;
#963 = CARTESIAN_POINT ( 'NONE',  ( -12.49999999999999289, 2.500000000000000000, -5.022947341949751454 ) ) ;
#964 = CARTESIAN_POINT ( 'NONE',  ( 6.249999999999930722, 2.500000000000000000, -1.472243186433550122 ) ) ;
#965 = ADVANCED_FACE ( 'NONE', ( #27385 ), #66674, .T. ) ;
#966 = DIRECTION ( 'NONE',  ( -4.274815082592931898E-19, -0.9999939076577903929, -0.003490651415223739937 ) ) ;
#967 = DIRECTION ( 'NONE',  ( -0.000000000000000000, 1.000000000000000000, -0.000000000000000000 ) ) ;
#968 = EDGE_CURVE ( 'NONE', #31124, #37879, #75433, .T. ) ;
#969 = AXIS2_PLACEMENT_3D ( 'NONE', #101280, #111743, #11603 ) ;
#970 = AXIS2_PLACEMENT_3D ( 'NONE', #65992, #45725, #47657 ) ;
#971 = ORIENTED_EDGE ( 'NONE', *, *, #117601, .T. ) ;
#972 = ORIENTED_EDGE ( 'NONE', *, *, #67206, .F. ) ;
#974 = ORIENTED_EDGE ( 'NONE', *, *, #58775, .T. ) ;
#973 = EDGE_CURVE ( 'NONE', #55129, #47060, #16904, .T. ) ;
#975 = ORIENTED_EDGE ( 'NONE', *, *, #76084, .F. ) ;
#976 = CARTESIAN_POINT ( 'NONE',  ( -1.650000000000035660, 12.50000000000000000, 7.188010851410848723 ) ) ;
#977 = EDGE_CURVE ( 'NONE', #39788, #14289, #44141, .T. ) ;
#978 = DIRECTION ( 'NONE',  ( -0.000000000000000000, 1.000000000000000000, -0.000000000000000000 ) ) ;
#979 = ORIENTED_EDGE ( 'NONE', *, *, #25487, .F. ) ;
#980 = FACE_BOUND ( 'NONE', #85138, .T. ) ;
#981 = DIRECTION ( 'NONE',  ( 0.000000000000000000, 0.000000000000000000, 1.000000000000000000 ) ) ;
#982 = EDGE_CURVE ( 'NONE', #98740, #31546, #87607, .T. ) ;
#983 = AXIS2_PLACEMENT_3D ( 'NONE', #115362, #85915, #18479 ) ;
#984 = DIRECTION ( 'NONE',  ( 0.000000000000000000, -0.9999939076577903929, 0.003490651415223739937 ) ) ;
#985 = EDGE_CURVE ( 'NONE', #72823, #32164, #4398, .T. ) ;
#986 = DIRECTION ( 'NONE',  ( 0.000000000000000000, -0.9999939076577903929, 0.003490651415223739937 ) ) ;
#987 = AXIS2_PLACEMENT_3D ( 'NONE', #18990, #69386, #100156 ) ;
#988 = CARTESIAN_POINT ( 'NONE',  ( 12.89999999999990266, 2.500000000000000000, -5.022947341949754119 ) ) ;
#989 = DIRECTION ( 'NONE',  ( 0.000000000000000000, 1.000000000000000000, 0.000000000000000000 ) ) ;
#990 = DIRECTION ( 'NONE',  ( 0.000000000000000000, -0.000000000000000000, 1.000000000000000000 ) ) ;
#991 = DIRECTION ( 'NONE',  ( 0.000000000000000000, 0.000000000000000000, 1.000000000000000000 ) ) ;
#992 = DIRECTION ( 'NONE',  ( 0.000000000000000000, 0.000000000000000000, 1.000000000000000000 ) ) ;
#993 = ORIENTED_EDGE ( 'NONE', *, *, #126584, .F. ) ;
#994 = EDGE_CURVE ( 'NONE', #52844, #31178, #17573, .T. ) ;
#995 = ORIENTED_EDGE ( 'NONE', *, *, #125991, .T. ) ;
#996 = VECTOR ( 'NONE', #128972, 1000.000000000000000 ) ;
#997 = VERTEX_POINT ( 'NONE', #98709 ) ;
#998 = EDGE_LOOP ( 'NONE', ( #19854, #122613 ) ) ;
#999 = VECTOR ( 'NONE', #84850, 1000.000000000000000 ) ;
#1000 = VERTEX_POINT ( 'NONE', #9044 ) ;
#1001 = EDGE_LOOP ( 'NONE', ( #92741, #66939, #84110, #76480 ) ) ;
#1002 = FACE_OUTER_BOUND ( 'NONE', #2724, .T. ) ;
#1003 = AXIS2_PLACEMENT_3D ( 'NONE', #62666, #82305, #12880 ) ;
#1004 = VERTEX_POINT ( 'NONE', #49002 ) ;
#1005 = CIRCLE ( 'NONE', #90886, 0.09999999999999999167 ) ;
#1006 = CARTESIAN_POINT ( 'NONE',  ( 12.49999999999993960, 2.500000000000000000, -4.430127018922202176 ) ) ;
#1007 = CARTESIAN_POINT ( 'NONE',  ( 183.9843750003414016, -8.734944146203032389, -1.604583208406768146E-15 ) ) ;
#1008 = PLANE ( 'NONE',  #81316 ) ;
#1009 = DIRECTION ( 'NONE',  ( 0.000000000000000000, 0.000000000000000000, -1.000000000000000000 ) ) ;
#1010 = VERTEX_POINT ( 'NONE', #35940 ) ;
#1011 = CARTESIAN_POINT ( 'NONE',  ( -4.350000000000023626, 2.500000000000000000, -2.511473670974877948 ) ) ;
#1012 = EDGE_LOOP ( 'NONE', ( #21519, #20729 ) ) ;
#1014 = ORIENTED_EDGE ( 'NONE', *, *, #70820, .T. ) ;
#1013 = CONICAL_SURFACE ( 'NONE', #32441, 0.09999999999999982514, 0.003490658503988666988 ) ;
#1015 = CARTESIAN_POINT ( 'NONE',  ( -6.650000000000019007, 2.500000000000000000, -5.902370205355750521 ) ) ;
#1016 = VECTOR ( 'NONE', #53390, 1000.000000000000000 ) ;
#1017 = AXIS2_PLACEMENT_3D ( 'NONE', #89269, #99100, #28425 ) ;
#1018 = CARTESIAN_POINT ( 'NONE',  ( -1.650000000000035660, 2.500000000000000000, 7.088010851410848190 ) ) ;
#1019 = CARTESIAN_POINT ( 'NONE',  ( -5.850000000000022737, 2.500000000000000000, -6.495190528383302464 ) ) ;
#1020 = VERTEX_POINT ( 'NONE', #96143 ) ;
#1021 = ORIENTED_EDGE ( 'NONE', *, *, #102730, .F. ) ;
#1022 = FACE_OUTER_BOUND ( 'NONE', #57191, .T. ) ;
#1023 = CONICAL_SURFACE ( 'NONE', #97171, 0.1000000000000002554, 0.003490658503988666988 ) ;
#1024 = EDGE_CURVE ( 'NONE', #126709, #55928, #16911, .T. ) ;
#1025 = VECTOR ( 'NONE', #26482, 1000.000000000000000 ) ;
#1026 = CARTESIAN_POINT ( 'NONE',  ( 5.399999999999934630, 2.500000000000000000, 0.6928203230275494784 ) ) ;
#1027 = DIRECTION ( 'NONE',  ( -4.274815082592931898E-19, -0.9999939076577903929, -0.003490651415223739937 ) ) ;
#1028 = DIRECTION ( 'NONE',  ( 0.000000000000000000, 0.000000000000000000, 1.000000000000000000 ) ) ;
#1029 = VERTEX_POINT ( 'NONE', #105968 ) ;
#1030 = CIRCLE ( 'NONE', #103446, 0.06509327318403745899 ) ;
#1031 = DIRECTION ( 'NONE',  ( -0.000000000000000000, 1.000000000000000000, -0.000000000000000000 ) ) ;
#1032 = ORIENTED_EDGE ( 'NONE', *, *, #41319, .T. ) ;
#1033 = CARTESIAN_POINT ( 'NONE',  ( 12.89999999999989733, 2.500000000000000000, -2.385244779468109755E-15 ) ) ;
#1034 = AXIS2_PLACEMENT_3D ( 'NONE', #123543, #109047, #126132 ) ;
#1035 = CIRCLE ( 'NONE', #74199, 0.1000000000000000472 ) ;
#1036 = EDGE_LOOP ( 'NONE', ( #81475, #129207 ) ) ;
#1037 = CARTESIAN_POINT ( 'NONE',  ( 17.50000000000000000, 2.500000000000000000, 3.666666666666666963 ) ) ;
#1038 = CARTESIAN_POINT ( 'NONE',  ( 9.149999999999918643, 2.500000000000000000, 2.165063509461097713 ) ) ;
#1039 = DIRECTION ( 'NONE',  ( 0.000000000000000000, -0.000000000000000000, 1.000000000000000000 ) ) ;
#1040 = CIRCLE ( 'NONE', #78431, 0.1000000000000002554 ) ;
#1041 = FACE_OUTER_BOUND ( 'NONE', #46553, .T. ) ;
#1042 = EDGE_LOOP ( 'NONE', ( #1365, #8512, #87614, #90230 ) ) ;
#1043 = CARTESIAN_POINT ( 'NONE',  ( -13.74999999999995381, 2.500000000000000000, 2.165063509461101265 ) ) ;
#1044 = CARTESIAN_POINT ( 'NONE',  ( 8.549999999999924327, 2.500000000000000000, -6.841600689897077814 ) ) ;
#1045 = ORIENTED_EDGE ( 'NONE', *, *, #38814, .T. ) ;
#1046 = VERTEX_POINT ( 'NONE', #51574 ) ;
#1047 = ORIENTED_EDGE ( 'NONE', *, *, #124636, .T. ) ;
#1048 = CARTESIAN_POINT ( 'NONE',  ( 2.500000000000002220, -0.9166666666666694052, 10.00000000000000178 ) ) ;
#1049 = DIRECTION ( 'NONE',  ( 0.000000000000000000, 0.000000000000000000, 1.000000000000000000 ) ) ;
#1050 = CARTESIAN_POINT ( 'NONE',  ( -9.600000000000006750, 12.50000000000000000, 3.637306695894644726 ) ) ;
#1051 = CARTESIAN_POINT ( 'NONE',  ( 4.399999999999937295, 2.500000000000000000, 4.083716857408421497 ) ) ;
#1052 = AXIS2_PLACEMENT_3D ( 'NONE', #24332, #114006, #43982 ) ;
#1053 = CARTESIAN_POINT ( 'NONE',  ( -3.350000000000029399, 2.500000000000000000, 6.495190528383297135 ) ) ;
#1054 = FACE_OUTER_BOUND ( 'NONE', #2883, .T. ) ;
#1055 = DIRECTION ( 'NONE',  ( 0.000000000000000000, 0.000000000000000000, 1.000000000000000000 ) ) ;
#1056 = CARTESIAN_POINT ( 'NONE',  ( -10.00000000000000533, 2.500000000000000000, 5.022947341949748790 ) ) ;
#1057 = DIRECTION ( 'NONE',  ( 0.000000000000000000, -0.9999939076577903929, 0.003490651415223739937 ) ) ;
#1058 = CONICAL_SURFACE ( 'NONE', #15714, 0.1000000000000002554, 0.003490658503988666988 ) ;
#1059 = CIRCLE ( 'NONE', #74226, 0.1000000000000002554 ) ;
#1060 = EDGE_CURVE ( 'NONE', #35393, #66105, #46193, .T. ) ;
#1061 = VERTEX_POINT ( 'NONE', #71193 ) ;
#1062 = DIRECTION ( 'NONE',  ( -1.000000000000000000, 0.000000000000000000, 1.445602896647339656E-16 ) ) ;
#1063 = ADVANCED_FACE ( 'NONE', ( #50928 ), #6447, .T. ) ;
#1064 = DIRECTION ( 'NONE',  ( 0.000000000000000000, 1.000000000000000000, 0.000000000000000000 ) ) ;
#1065 = CARTESIAN_POINT ( 'NONE',  ( 1.249999999999954259, 2.500000000000000000, -7.288010851410854585 ) ) ;
#1066 = DIRECTION ( 'NONE',  ( -0.000000000000000000, -1.000000000000000000, -0.000000000000000000 ) ) ;
#1067 = ADVANCED_FACE ( 'NONE', ( #50277 ), #60866, .T. ) ;
#1068 = EDGE_LOOP ( 'NONE', ( #104380, #90932, #57767, #56448 ) ) ;
#1069 = DIRECTION ( 'NONE',  ( -0.000000000000000000, 1.000000000000000000, -0.000000000000000000 ) ) ;
#1070 = AXIS2_PLACEMENT_3D ( 'NONE', #62806, #33363, #52331 ) ;
#1071 = CARTESIAN_POINT ( 'NONE',  ( 0.3999999999999555023, 12.50000000000000000, 4.330127018922196314 ) ) ;
#1073 = ORIENTED_EDGE ( 'NONE', *, *, #100282, .F. ) ;
#1072 = LINE ( 'NONE', #3653, #31661 ) ;
#1074 = EDGE_CURVE ( 'NONE', #58319, #8778, #109867, .T. ) ;
#1075 = EDGE_CURVE ( 'NONE', #24109, #85332, #128671, .T. ) ;
#1076 = ADVANCED_FACE ( 'NONE', ( #110478 ), #13694, .T. ) ;
#1077 = ADVANCED_FACE ( 'NONE', ( #100643 ), #63884, .T. ) ;
#1078 = EDGE_CURVE ( 'NONE', #3798, #21836, #99406, .T. ) ;
#1079 = EDGE_LOOP ( 'NONE', ( #32587, #83909 ) ) ;
#1080 = CARTESIAN_POINT ( 'NONE',  ( 2.499999999999947153, 2.500000000000000000, 0.6928203230275494784 ) ) ;
#1081 = AXIS2_PLACEMENT_3D ( 'NONE', #63126, #90652, #80846 ) ;
#1082 = ORIENTED_EDGE ( 'NONE', *, *, #3024, .T. ) ;
#1083 = EDGE_LOOP ( 'NONE', ( #127551, #120321, #103737, #57132 ) ) ;
#1084 = FACE_OUTER_BOUND ( 'NONE', #30197, .T. ) ;
#1085 = EDGE_CURVE ( 'NONE', #94776, #42733, #101315, .T. ) ;
#1086 = CARTESIAN_POINT ( 'NONE',  ( 21.24754738303297330, 0.7337760880902505223, -4.182111650399365388 ) ) ;
#1087 = CARTESIAN_POINT ( 'NONE',  ( 11.04999999999991012, 2.500000000000000000, 6.841600689897072485 ) ) ;
#1088 = DIRECTION ( 'NONE',  ( 0.000000000000000000, 0.000000000000000000, 1.000000000000000000 ) ) ;
#1090 = ORIENTED_EDGE ( 'NONE', *, *, #103759, .F. ) ;
#1089 = EDGE_CURVE ( 'NONE', #123569, #92739, #5286, .T. ) ;
#1091 = FACE_OUTER_BOUND ( 'NONE', #74753, .T. ) ;
#1092 = ORIENTED_EDGE ( 'NONE', *, *, #21775, .T. ) ;
#1093 = CARTESIAN_POINT ( 'NONE',  ( -5.400000000000019895, 2.500000000000000000, -0.7928203230275542301 ) ) ;
#1094 = SHAPE_REPRESENTATION ( 'Brush Head Assembly', ( #108296 ), #79070 ) ;
#1095 = DIRECTION ( 'NONE',  ( 0.000000000000000000, 1.000000000000000000, 0.000000000000000000 ) ) ;
#1096 = VECTOR ( 'NONE', #95538, 1000.000000000000000 ) ;
#1097 = ORIENTED_EDGE ( 'NONE', *, *, #54469, .T. ) ;
#1098 = ORIENTED_EDGE ( 'NONE', *, *, #72625, .T. ) ;
#1099 = CIRCLE ( 'NONE', #95207, 0.09999999999999982514 ) ;
#1100 = ORIENTED_EDGE ( 'NONE', *, *, #118125, .F. ) ;
#1101 = ORIENTED_EDGE ( 'NONE', *, *, #20054, .T. ) ;
#1102 = FACE_OUTER_BOUND ( 'NONE', #310, .T. ) ;
#1103 = CARTESIAN_POINT ( 'NONE',  ( 10.30524027341048843, 2.500000000000255795, 9.130939513283916398 ) ) ;
#1104 = AXIS2_PLACEMENT_3D ( 'NONE', #80551, #17737, #87765 ) ;
#1105 = PLANE ( 'NONE',  #100600 ) ;
#1106 = FACE_BOUND ( 'NONE', #107447, .T. ) ;
#1107 = DIRECTION ( 'NONE',  ( 0.000000000000000000, 0.000000000000000000, -1.000000000000000000 ) ) ;
#1108 = CARTESIAN_POINT ( 'NONE',  ( 185.4062500006828316, -8.891194145520236347, -1.633285867636356693E-15 ) ) ;
#1109 = DIRECTION ( 'NONE',  ( 0.000000000000000000, 0.000000000000000000, 1.000000000000000000 ) ) ;
#1110 = DIRECTION ( 'NONE',  ( 0.000000000000000000, 0.000000000000000000, -1.000000000000000000 ) ) ;
#1111 = AXIS2_PLACEMENT_3D ( 'NONE', #4715, #13259, #63021 ) ;
#1112 = AXIS2_PLACEMENT_3D ( 'NONE', #31334, #127742, #46602 ) ;
#1113 = FACE_OUTER_BOUND ( 'NONE', #44992, .T. ) ;
#1114 = AXIS2_PLACEMENT_3D ( 'NONE', #95902, #65786, #78208 ) ;
#1115 = LINE ( 'NONE', #3693, #7032 ) ;
#1116 = ADVANCED_FACE ( 'NONE', ( #41119 ), #32516, .T. ) ;
#1117 = CARTESIAN_POINT ( 'NONE',  ( 187.5000000000000000, 0.000000000000000000, 0.000000000000000000 ) ) ;
#1118 = EDGE_CURVE ( 'NONE', #65792, #60753, #101952, .T. ) ;
#1119 = AXIS2_PLACEMENT_3D ( 'NONE', #101193, #111660, #90723 ) ;
#1120 = CONICAL_SURFACE ( 'NONE', #78516, 0.1000000000000002554, 0.003490658503988666988 ) ;
#1121 = DIRECTION ( 'NONE',  ( 0.000000000000000000, 0.000000000000000000, 1.000000000000000000 ) ) ;
#1122 = EDGE_CURVE ( 'NONE', #21908, #57789, #128863, .T. ) ;
#1123 = ORIENTED_EDGE ( 'NONE', *, *, #105248, .F. ) ;
#1124 = VERTEX_POINT ( 'NONE', #39191 ) ;
#1125 = VERTEX_POINT ( 'NONE', #1800 ) ;
#1126 = EDGE_LOOP ( 'NONE', ( #75811, #97863 ) ) ;
#1127 = AXIS2_PLACEMENT_3D ( 'NONE', #59022, #38766, #108112 ) ;
#1128 = ORIENTED_EDGE ( 'NONE', *, *, #63191, .F. ) ;
#1129 = DIRECTION ( 'NONE',  ( 0.000000000000000000, 1.000000000000000000, 0.000000000000000000 ) ) ;
#1130 = DIRECTION ( 'NONE',  ( -0.000000000000000000, -1.000000000000000000, -0.000000000000000000 ) ) ;
#1132 = EDGE_CURVE ( 'NONE', #88013, #108519, #103610, .T. ) ;
#1131 = EDGE_LOOP ( 'NONE', ( #25952, #97783 ) ) ;
#1133 = FACE_BOUND ( 'NONE', #57001, .T. ) ;
#1134 = DIRECTION ( 'NONE',  ( 0.000000000000000000, 0.000000000000000000, 1.000000000000000000 ) ) ;
#1135 = ADVANCED_FACE ( 'NONE', ( #121576 ), #88934, .T. ) ;
#1136 = ADVANCED_FACE ( 'NONE', ( #79104 ), #62037, .T. ) ;
#1137 = ORIENTED_EDGE ( 'NONE', *, *, #42942, .T. ) ;
#1138 = DIRECTION ( 'NONE',  ( -0.000000000000000000, -1.000000000000000000, -0.000000000000000000 ) ) ;
#1139 = DIRECTION ( 'NONE',  ( 0.000000000000000000, 1.000000000000000000, 0.000000000000000000 ) ) ;
#1140 = CARTESIAN_POINT ( 'NONE',  ( 8.749999999999953815, 2.500000000000000000, 6.595190528383296780 ) ) ;
#1141 = CARTESIAN_POINT ( 'NONE',  ( -8.950000000000006395, 12.50000000000000000, 6.841600689897072485 ) ) ;
#1143 = ORIENTED_EDGE ( 'NONE', *, *, #102989, .F. ) ;
#1142 = AXIS2_PLACEMENT_3D ( 'NONE', #35448, #115249, #27529 ) ;
#1144 = DIRECTION ( 'NONE',  ( 0.000000000000000000, 1.000000000000000000, 0.000000000000000000 ) ) ;
#1145 = ADVANCED_FACE ( 'NONE', ( #59478 ), #36711, .T. ) ;
#1146 = EDGE_LOOP ( 'NONE', ( #88682, #16117 ) ) ;
#1147 = ORIENTED_EDGE ( 'NONE', *, *, #35573, .F. ) ;
#1148 = CARTESIAN_POINT ( 'NONE',  ( -5.600000000000020073, 12.50000000000000000, 4.676537180435972552 ) ) ;
#1149 = CARTESIAN_POINT ( 'NONE',  ( -1.250000000000036193, 2.500000000000000000, 5.802370205355744659 ) ) ;
#1150 = AXIS2_PLACEMENT_3D ( 'NONE', #42717, #70863, #110771 ) ;
#1151 = ORIENTED_EDGE ( 'NONE', *, *, #63327, .F. ) ;
#1152 = DIRECTION ( 'NONE',  ( 0.000000000000000000, 0.000000000000000000, 1.000000000000000000 ) ) ;
#1153 = AXIS2_PLACEMENT_3D ( 'NONE', #77461, #118027, #89218 ) ;
#1154 = AXIS2_PLACEMENT_3D ( 'NONE', #37682, #78907, #89983 ) ;
#1155 = FACE_OUTER_BOUND ( 'NONE', #34928, .T. ) ;
#1156 = DIRECTION ( 'NONE',  ( 0.000000000000000000, 0.000000000000000000, 1.000000000000000000 ) ) ;
#1157 = CARTESIAN_POINT ( 'NONE',  ( -6.650000000000018119, 12.50000000000000000, -2.857883832488653741 ) ) ;
#1158 = EDGE_LOOP ( 'NONE', ( #77071, #69585 ) ) ;
#1159 = FACE_OUTER_BOUND ( 'NONE', #85226, .T. ) ;
#1160 = EDGE_CURVE ( 'NONE', #14447, #93919, #13555, .T. ) ;
#1161 = ORIENTED_EDGE ( 'NONE', *, *, #44076, .T. ) ;
#1162 = DIRECTION ( 'NONE',  ( 1.000000000000000000, 0.000000000000000000, 0.000000000000000000 ) ) ;
#1163 = CIRCLE ( 'NONE', #26314, 0.06509327318403745899 ) ;
#1164 = ORIENTED_EDGE ( 'NONE', *, *, #15453, .F. ) ;
#1166 = FACE_OUTER_BOUND ( 'NONE', #110008, .T. ) ;
#1165 = AXIS2_PLACEMENT_3D ( 'NONE', #71829, #42368, #100001 ) ;
#1167 = ORIENTED_EDGE ( 'NONE', *, *, #16843, .F. ) ;
#1168 = CARTESIAN_POINT ( 'NONE',  ( -6.650000000000018119, 2.500000000000000000, -7.188010851410854052 ) ) ;
#1169 = DIRECTION ( 'NONE',  ( 0.000000000000000000, 0.000000000000000000, -1.000000000000000000 ) ) ;
#1170 = DIRECTION ( 'NONE',  ( 0.000000000000000000, -0.000000000000000000, 1.000000000000000000 ) ) ;
#1171 = DIRECTION ( 'NONE',  ( 0.000000000000000000, 0.000000000000000000, 1.000000000000000000 ) ) ;
#1172 = LINE ( 'NONE', #41123, #72590 ) ;
#1173 = ORIENTED_EDGE ( 'NONE', *, *, #88308, .T. ) ;
#1174 = ORIENTED_EDGE ( 'NONE', *, *, #19, .F. ) ;
#1175 = ORIENTED_EDGE ( 'NONE', *, *, #113846, .T. ) ;
#1176 = CARTESIAN_POINT ( 'NONE',  ( -2.900000000000029665, 2.500000000000000000, 4.330127018922196314 ) ) ;
#1177 = AXIS2_PLACEMENT_3D ( 'NONE', #78084, #89190, #49287 ) ;
#1178 = CIRCLE ( 'NONE', #17897, 0.1000000000000002554 ) ;
#1179 = EDGE_CURVE ( 'NONE', #106389, #62016, #63962, .T. ) ;
#1180 = CARTESIAN_POINT ( 'NONE',  ( 9.149999999999920419, 2.500000000000000000, -7.188010851410854052 ) ) ;
#1181 = CARTESIAN_POINT ( 'NONE',  ( -4.076600168545496672E-14, 2.500000000000000000, -5.022947341949754119 ) ) ;
#1183 = VERTEX_POINT ( 'NONE', #84228 ) ;
#1182 = ORIENTED_EDGE ( 'NONE', *, *, #89891, .T. ) ;
#1184 = VERTEX_POINT ( 'NONE', #73137 ) ;
#1185 = DIRECTION ( 'NONE',  ( -0.000000000000000000, -1.000000000000000000, -0.000000000000000000 ) ) ;
#1186 = EDGE_LOOP ( 'NONE', ( #60111, #65298, #25080, #7290 ) ) ;
#1187 = FACE_OUTER_BOUND ( 'NONE', #64228, .T. ) ;
#1188 = DIRECTION ( 'NONE',  ( 0.000000000000000000, 0.000000000000000000, 1.000000000000000000 ) ) ;
#1189 = LINE ( 'NONE', #41141, #11390 ) ;
#1190 = FACE_OUTER_BOUND ( 'NONE', #75353, .T. ) ;
#1191 = CARTESIAN_POINT ( 'NONE',  ( -3.100000000000028955, 2.500000000000000000, 3.983716857408420964 ) ) ;
#1192 = DIRECTION ( 'NONE',  ( -0.000000000000000000, 1.000000000000000000, -0.000000000000000000 ) ) ;
#1193 = DIRECTION ( 'NONE',  ( 0.000000000000000000, 0.000000000000000000, 1.000000000000000000 ) ) ;
#1194 = ADVANCED_FACE ( 'NONE', ( #12897 ), #72503, .T. ) ;
#1195 = AXIS2_PLACEMENT_3D ( 'NONE', #81684, #121600, #69941 ) ;
#1196 = CARTESIAN_POINT ( 'NONE',  ( 8.149999999999923972, 12.50000000000000000, -6.083687093685488989 ) ) ;
#1197 = VERTEX_POINT ( 'NONE', #32595 ) ;
#1198 = CARTESIAN_POINT ( 'NONE',  ( -10.40000000000000213, 2.500000000000000000, -0.6928203230275541413 ) ) ;
#1199 = AXIS2_PLACEMENT_3D ( 'NONE', #76823, #58489, #116728 ) ;
#1200 = CIRCLE ( 'NONE', #17920, 0.06509327318403745899 ) ;
#1201 = FACE_OUTER_BOUND ( 'NONE', #56405, .T. ) ;
#1202 = ORIENTED_EDGE ( 'NONE', *, *, #126692, .T. ) ;
#1203 = ORIENTED_EDGE ( 'NONE', *, *, #12560, .T. ) ;
#1204 = CARTESIAN_POINT ( 'NONE',  ( 184.8593750003413732, 0.000000000000000000, 7.564683531250000925 ) ) ;
#1205 = DIRECTION ( 'NONE',  ( 0.000000000000000000, 0.000000000000000000, -1.000000000000000000 ) ) ;
#1206 = DIRECTION ( 'NONE',  ( 0.000000000000000000, 0.000000000000000000, 1.000000000000000000 ) ) ;
#1207 = DIRECTION ( 'NONE',  ( -1.000000000000000000, -0.000000000000000000, -0.000000000000000000 ) ) ;
#1208 = AXIS2_PLACEMENT_3D ( 'NONE', #111977, #40014, #51132 ) ;
#1209 = FACE_OUTER_BOUND ( 'NONE', #113304, .T. ) ;
#1210 = CARTESIAN_POINT ( 'NONE',  ( -4.800000000000022915, 2.500000000000000000, -0.3464101615137783474 ) ) ;
#1211 = CARTESIAN_POINT ( 'NONE',  ( 5.849999999999935696, 2.500000000000000000, -7.088010851410853519 ) ) ;
#1212 = CARTESIAN_POINT ( 'NONE',  ( 4.399999999999939071, 2.500000000000000000, -0.4464101615137782142 ) ) ;
#1213 = CIRCLE ( 'NONE', #68098, 0.06509327318403745899 ) ;
#1214 = CARTESIAN_POINT ( 'NONE',  ( -1.250000000000036193, 2.500000000000000000, 1.472243186433545459 ) ) ;
#1215 = VECTOR ( 'NONE', #47434, 1000.000000000000000 ) ;
#1216 = CONICAL_SURFACE ( 'NONE', #40959, 0.09999999999999982514, 0.003490658503988666988 ) ;
#1217 = ORIENTED_EDGE ( 'NONE', *, *, #56795, .F. ) ;
#1218 = ORIENTED_EDGE ( 'NONE', *, *, #101381, .T. ) ;
#1220 = ADVANCED_FACE ( 'NONE', ( #43062 ), #45026, .T. ) ;
#1219 = VECTOR ( 'NONE', #63000, 1000.000000000000000 ) ;
#1221 = ORIENTED_EDGE ( 'NONE', *, *, #45182, .T. ) ;
#1222 = ORIENTED_EDGE ( 'NONE', *, *, #15384, .T. ) ;
#1223 = ORIENTED_EDGE ( 'NONE', *, *, #53101, .F. ) ;
#1224 = PLANE ( 'NONE',  #42103 ) ;
#1225 = FACE_OUTER_BOUND ( 'NONE', #37159, .T. ) ;
#1226 = ADVANCED_FACE ( 'NONE', ( #124820 ), #52852, .F. ) ;
#1227 = ORIENTED_EDGE ( 'NONE', *, *, #26923, .T. ) ;
#1228 = DIRECTION ( 'NONE',  ( 0.000000000000000000, 1.000000000000000000, 0.000000000000000000 ) ) ;
#1229 = DIRECTION ( 'NONE',  ( 0.000000000000000000, 1.000000000000000000, 0.000000000000000000 ) ) ;
#1230 = CARTESIAN_POINT ( 'NONE',  ( 10.84999999999991260, 2.500000000000000000, 5.802370205355744659 ) ) ;
#1232 = EDGE_LOOP ( 'NONE', ( #95732, #16124 ) ) ;
#1231 = DIRECTION ( 'NONE',  ( 0.000000000000000000, 0.000000000000000000, 1.000000000000000000 ) ) ;
#1233 = EDGE_CURVE ( 'NONE', #62826, #110935, #84883, .T. ) ;
#1234 = ADVANCED_FACE ( 'NONE', ( #52209 ), #65230, .T. ) ;
#1235 = EDGE_CURVE ( 'NONE', #53159, #69354, #47167, .T. ) ;
#1236 = CARTESIAN_POINT ( 'NONE',  ( 8.099999999999923261, 2.500000000000000000, -4.776537180435978414 ) ) ;
#1237 = EDGE_CURVE ( 'NONE', #120782, #8397, #7439, .T. ) ;
#1238 = CIRCLE ( 'NONE', #126639, 0.06509327318403745899 ) ;
#1239 = FACE_OUTER_BOUND ( 'NONE', #8734, .T. ) ;
#1240 = ORIENTED_EDGE ( 'NONE', *, *, #56224, .T. ) ;
#1241 = ADVANCED_FACE ( 'NONE', ( #35162 ), #95192, .T. ) ;
#1242 = ORIENTED_EDGE ( 'NONE', *, *, #51274, .F. ) ;
#1243 = EDGE_LOOP ( 'NONE', ( #124951, #37318 ) ) ;
#1244 = ORIENTED_EDGE ( 'NONE', *, *, #100146, .F. ) ;
#1245 = DIRECTION ( 'NONE',  ( 0.000000000000000000, 0.000000000000000000, 1.000000000000000000 ) ) ;
#1246 = EDGE_CURVE ( 'NONE', #105517, #83506, #22043, .T. ) ;
#1247 = VECTOR ( 'NONE', #117999, 1000.000000000000000 ) ;
#1248 = CARTESIAN_POINT ( 'NONE',  ( 4.799999999999935874, 2.500000000000000000, 0.3464101615137735735 ) ) ;
#1249 = CARTESIAN_POINT ( 'NONE',  ( 2.500000000000002220, -2.500000000000000000, -9.261799387799147354 ) ) ;
#1250 = AXIS2_PLACEMENT_3D ( 'NONE', #108337, #88029, #118162 ) ;
#1251 = EDGE_CURVE ( 'NONE', #4623, #7925, #55483, .T. ) ;
#1252 = ADVANCED_FACE ( 'NONE', ( #44974 ), #23568, .T. ) ;
#1253 = CIRCLE ( 'NONE', #74415, 0.06509327318403745899 ) ;
#1254 = CARTESIAN_POINT ( 'NONE',  ( 115.5000000000000000, 5.000000000000000000, -4.999999999999997335 ) ) ;
#1255 = VERTEX_POINT ( 'NONE', #54770 ) ;
#1256 = CARTESIAN_POINT ( 'NONE',  ( 13.74999999999989875, 12.50000000000000000, 1.472243186433545459 ) ) ;
#1257 = LINE ( 'NONE', #41204, #120746 ) ;
#1258 = CARTESIAN_POINT ( 'NONE',  ( -7.700000000000010836, 12.50000000000000000, 3.983716857408420964 ) ) ;
#1259 = CARTESIAN_POINT ( 'NONE',  ( 9.199999999999915801, 2.500000000000000000, -4.330127018922201643 ) ) ;
#1260 = EDGE_CURVE ( 'NONE', #129522, #47326, #73726, .T. ) ;
#1261 = CIRCLE ( 'NONE', #68150, 0.06509327318403745899 ) ;
#1262 = VERTEX_POINT ( 'NONE', #122886 ) ;
#1263 = VECTOR ( 'NONE', #94221, 1000.000000000000000 ) ;
#1264 = ORIENTED_EDGE ( 'NONE', *, *, #70825, .F. ) ;
#1265 = VERTEX_POINT ( 'NONE', #25298 ) ;
#1266 = DIRECTION ( 'NONE',  ( 0.000000000000000000, -0.000000000000000000, 1.000000000000000000 ) ) ;
#1267 = LINE ( 'NONE', #3840, #114989 ) ;
#1268 = FACE_BOUND ( 'NONE', #43258, .T. ) ;
#1269 = DIRECTION ( 'NONE',  ( -0.000000000000000000, 1.000000000000000000, -0.000000000000000000 ) ) ;
#1270 = CARTESIAN_POINT ( 'NONE',  ( -7.050000000000016698, 2.500000000000000000, -2.165063509461101710 ) ) ;
#1271 = FACE_OUTER_BOUND ( 'NONE', #75762, .T. ) ;
#1272 = AXIS2_PLACEMENT_3D ( 'NONE', #26918, #47859, #17054 ) ;
#1273 = DIRECTION ( 'NONE',  ( 0.000000000000000000, 1.000000000000000000, 0.000000000000000000 ) ) ;
#1274 = CARTESIAN_POINT ( 'NONE',  ( -12.69999999999999218, 12.50000000000000000, 4.676537180435972552 ) ) ;
#1275 = FACE_OUTER_BOUND ( 'NONE', #100380, .T. ) ;
#1276 = ORIENTED_EDGE ( 'NONE', *, *, #2567, .T. ) ;
#1277 = FACE_OUTER_BOUND ( 'NONE', #39005, .T. ) ;
#1278 = CARTESIAN_POINT ( 'NONE',  ( 6.849999999999930367, 12.50000000000000000, -6.776507416713040577 ) ) ;
#1279 = ORIENTED_EDGE ( 'NONE', *, *, #7307, .T. ) ;
#1280 = EDGE_LOOP ( 'NONE', ( #1759, #3092, #98830, #88037 ) ) ;
#1281 = DIRECTION ( 'NONE',  ( 0.000000000000000000, 0.000000000000000000, 1.000000000000000000 ) ) ;
#1282 = CARTESIAN_POINT ( 'NONE',  ( 10.84999999999990905, 2.500000000000000000, -7.288010851410854585 ) ) ;
#1283 = FACE_BOUND ( 'NONE', #29371, .T. ) ;
#1284 = DIRECTION ( 'NONE',  ( -0.000000000000000000, 1.000000000000000000, -0.000000000000000000 ) ) ;
#1285 = EDGE_CURVE ( 'NONE', #65003, #93435, #96710, .T. ) ;
#1286 = CONICAL_SURFACE ( 'NONE', #7534, 0.09999999999999982514, 0.003490658503988666988 ) ;
#1287 = LINE ( 'NONE', #60239, #54902 ) ;
#1288 = EDGE_CURVE ( 'NONE', #110742, #77067, #67759, .T. ) ;
#1289 = ORIENTED_EDGE ( 'NONE', *, *, #26689, .F. ) ;
#1290 = LINE ( 'NONE', #22241, #2696 ) ;
#1291 = CARTESIAN_POINT ( 'NONE',  ( 1.249999999999988454, 12.50000000000000000, 2.165063509461097713 ) ) ;
#1292 = VERTEX_POINT ( 'NONE', #3113 ) ;
#1293 = DIRECTION ( 'NONE',  ( -0.000000000000000000, -1.000000000000000000, -0.000000000000000000 ) ) ;
#1294 = FACE_OUTER_BOUND ( 'NONE', #121910, .T. ) ;
#1295 = EDGE_CURVE ( 'NONE', #118275, #98777, #128552, .T. ) ;
#1297 = VECTOR ( 'NONE', #4974, 1000.000000000000000 ) ;
#1296 = CIRCLE ( 'NONE', #43377, 0.09999999999999982514 ) ;
#1298 = DIRECTION ( 'NONE',  ( 0.000000000000000000, 0.000000000000000000, 1.000000000000000000 ) ) ;
#1299 = PLANE ( 'NONE',  #126302 ) ;
#1301 = CIRCLE ( 'NONE', #116310, 0.06509327318403745899 ) ;
#1300 = CIRCLE ( 'NONE', #97452, 0.06509327318403745899 ) ;
#1302 = ORIENTED_EDGE ( 'NONE', *, *, #63770, .T. ) ;
#1303 = AXIS2_PLACEMENT_3D ( 'NONE', #65571, #46568, #38054 ) ;
#1304 = DIRECTION ( 'NONE',  ( 0.000000000000000000, 0.000000000000000000, -1.000000000000000000 ) ) ;
#1305 = CARTESIAN_POINT ( 'NONE',  ( -2.900000000000029665, 2.500000000000000000, 3.637306695894644726 ) ) ;
#1306 = DIRECTION ( 'NONE',  ( 0.000000000000000000, 0.000000000000000000, -1.000000000000000000 ) ) ;
#1307 = VERTEX_POINT ( 'NONE', #129199 ) ;
#1308 = ORIENTED_EDGE ( 'NONE', *, *, #106310, .T. ) ;
#1309 = FACE_OUTER_BOUND ( 'NONE', #46149, .T. ) ;
#1310 = ORIENTED_EDGE ( 'NONE', *, *, #78972, .F. ) ;
#1311 = DIRECTION ( 'NONE',  ( 0.000000000000000000, 0.000000000000000000, 1.000000000000000000 ) ) ;
#1312 = LINE ( 'NONE', #113194, #30722 ) ;
#1313 = CARTESIAN_POINT ( 'NONE',  ( 4.399999999999937295, 2.500000000000000000, 3.983716857408420964 ) ) ;
#1314 = VERTEX_POINT ( 'NONE', #49986 ) ;
#1315 = DIRECTION ( 'NONE',  ( -0.000000000000000000, 1.000000000000000000, -0.000000000000000000 ) ) ;
#1316 = CARTESIAN_POINT ( 'NONE',  ( 2.699999999999946443, 12.50000000000000000, 0.3464101615137735735 ) ) ;
#1317 = DIRECTION ( 'NONE',  ( 0.000000000000000000, -0.9999939076577903929, 0.003490651415223739937 ) ) ;
#1318 = DIRECTION ( 'NONE',  ( 0.000000000000000000, 0.000000000000000000, -1.000000000000000000 ) ) ;
#1319 = DIRECTION ( 'NONE',  ( 0.000000000000000000, 0.000000000000000000, 1.000000000000000000 ) ) ;
#1320 = CIRCLE ( 'NONE', #36847, 0.1000000000000000472 ) ;
#1321 = DIRECTION ( 'NONE',  ( 0.000000000000000000, 0.000000000000000000, 1.000000000000000000 ) ) ;
#1322 = ORIENTED_EDGE ( 'NONE', *, *, #125991, .F. ) ;
#1323 = ORIENTED_EDGE ( 'NONE', *, *, #22673, .F. ) ;
#1324 = DIRECTION ( 'NONE',  ( 0.000000000000000000, 1.000000000000000000, 0.000000000000000000 ) ) ;
#1325 = ORIENTED_EDGE ( 'NONE', *, *, #65628, .T. ) ;
#1326 = AXIS2_PLACEMENT_3D ( 'NONE', #104398, #63835, #72374 ) ;
#1327 = DIRECTION ( 'NONE',  ( -1.000000000000000000, -0.000000000000000000, -0.000000000000000000 ) ) ;
#1329 = EDGE_LOOP ( 'NONE', ( #53660, #26725 ) ) ;
#1328 = ORIENTED_EDGE ( 'NONE', *, *, #113030, .F. ) ;
#1330 = AXIS2_PLACEMENT_3D ( 'NONE', #86304, #57514, #117044 ) ;
#1331 = EDGE_LOOP ( 'NONE', ( #72263, #28879, #15786, #82302 ) ) ;
#1332 = CARTESIAN_POINT ( 'NONE',  ( 8.349999999999923261, 12.50000000000000000, 2.099970236277060032 ) ) ;
#1333 = VECTOR ( 'NONE', #38513, 1000.000000000000000 ) ;
#1334 = AXIS2_PLACEMENT_3D ( 'NONE', #20461, #101598, #10607 ) ;
#1335 = CARTESIAN_POINT ( 'NONE',  ( -1.450000000000036371, 2.500000000000000000, 6.841600689897072485 ) ) ;
#1336 = DIRECTION ( 'NONE',  ( 0.000000000000000000, 1.000000000000000000, 0.000000000000000000 ) ) ;
#1337 = CARTESIAN_POINT ( 'NONE',  ( -0.8000000000000315747, 2.500000000000000000, 0.000000000000000000 ) ) ;
#1338 = DIRECTION ( 'NONE',  ( 0.000000000000000000, 0.000000000000000000, -1.000000000000000000 ) ) ;
#1339 = CARTESIAN_POINT ( 'NONE',  ( 3.549999999999944755, 2.500000000000000000, -6.841600689897077814 ) ) ;
#1340 = EDGE_CURVE ( 'NONE', #2601, #71725, #123903, .T. ) ;
#1341 = CARTESIAN_POINT ( 'NONE',  ( -3.350000000000028511, 12.50000000000000000, -2.857883832488653741 ) ) ;
#1342 = CARTESIAN_POINT ( 'NONE',  ( -1.900000000000034106, 2.500000000000000000, 0.4464101615137735513 ) ) ;
#1343 = ADVANCED_FACE ( 'NONE', ( #70250 ), #124200, .T. ) ;
#1344 = DIRECTION ( 'NONE',  ( 0.000000000000000000, 1.000000000000000000, 0.000000000000000000 ) ) ;
#1345 = CIRCLE ( 'NONE', #59970, 0.06509327318403745899 ) ;
#1346 = ORIENTED_EDGE ( 'NONE', *, *, #57071, .F. ) ;
#1348 = CIRCLE ( 'NONE', #55730, 0.1000000000000002554 ) ;
#1347 = AXIS2_PLACEMENT_3D ( 'NONE', #82334, #73777, #14206 ) ;
#1349 = DIRECTION ( 'NONE',  ( -0.000000000000000000, -1.000000000000000000, -0.000000000000000000 ) ) ;
#1350 = VERTEX_POINT ( 'NONE', #108865 ) ;
#1351 = EDGE_CURVE ( 'NONE', #25898, #31429, #87294, .T. ) ;
#1352 = ORIENTED_EDGE ( 'NONE', *, *, #91149, .T. ) ;
#1353 = DIRECTION ( 'NONE',  ( 1.000000000000000000, 0.000000000000000000, 0.000000000000000000 ) ) ;
#1354 = CARTESIAN_POINT ( 'NONE',  ( 10.84999999999991260, 12.50000000000000000, 6.495190528383297135 ) ) ;
#1355 = FACE_OUTER_BOUND ( 'NONE', #119817, .T. ) ;
#1356 = CARTESIAN_POINT ( 'NONE',  ( -2.900000000000029221, 12.50000000000000000, -0.6928203230275541413 ) ) ;
#1357 = CARTESIAN_POINT ( 'NONE',  ( -9.800000000000006040, 2.500000000000000000, -4.676537180435974328 ) ) ;
#1358 = FACE_OUTER_BOUND ( 'NONE', #50552, .T. ) ;
#1359 = ORIENTED_EDGE ( 'NONE', *, *, #63750, .T. ) ;
#1360 = EDGE_LOOP ( 'NONE', ( #49377, #81992, #122314 ) ) ;
#1361 = VERTEX_POINT ( 'NONE', #127245 ) ;
#1363 = ADVANCED_FACE ( 'NONE', ( #59151 ), #119338, .T. ) ;
#1362 = FACE_OUTER_BOUND ( 'NONE', #11330, .T. ) ;
#1364 = ORIENTED_EDGE ( 'NONE', *, *, #72648, .F. ) ;
#1365 = ORIENTED_EDGE ( 'NONE', *, *, #24267, .F. ) ;
#1366 = DIRECTION ( 'NONE',  ( -0.000000000000000000, -1.000000000000000000, -0.000000000000000000 ) ) ;
#1367 = DIRECTION ( 'NONE',  ( 0.000000000000000000, 0.000000000000000000, 1.000000000000000000 ) ) ;
#1368 = EDGE_CURVE ( 'NONE', #120113, #49114, #80068, .T. ) ;
#1369 = AXIS2_PLACEMENT_3D ( 'NONE', #11132, #61553, #12426 ) ;
#1370 = DIRECTION ( 'NONE',  ( -0.000000000000000000, 1.000000000000000000, -0.000000000000000000 ) ) ;
#1372 = CARTESIAN_POINT ( 'NONE',  ( -12.49999999999995737, 2.500000000000000000, 4.330127018922196314 ) ) ;
#1371 = CIRCLE ( 'NONE', #74543, 0.09999999999999982514 ) ;
#1373 = CARTESIAN_POINT ( 'NONE',  ( 17.50000000000000000, -1.666666666666667851, 4.000000000000001776 ) ) ;
#1374 = VERTEX_POINT ( 'NONE', #30344 ) ;
#1375 = CARTESIAN_POINT ( 'NONE',  ( 4.349999999999941025, 2.500000000000000000, -6.048780366869526581 ) ) ;
#1376 = CARTESIAN_POINT ( 'NONE',  ( -12.04999999999999538, 2.500000000000000000, 2.065063509461097624 ) ) ;
#1377 = EDGE_CURVE ( 'NONE', #21459, #55389, #67444, .T. ) ;
#1378 = EDGE_CURVE ( 'NONE', #32526, #19824, #107178, .T. ) ;
#1379 = CARTESIAN_POINT ( 'NONE',  ( 10.84999999999990905, 2.500000000000000000, -7.188010851410854052 ) ) ;
#1380 = EDGE_CURVE ( 'NONE', #50137, #26812, #566, .T. ) ;
#1381 = CARTESIAN_POINT ( 'NONE',  ( 10.84999999999991260, 2.500000000000000000, -2.957883832488653830 ) ) ;
#1382 = EDGE_CURVE ( 'NONE', #66554, #27692, #120003, .T. ) ;
#1384 = CONICAL_SURFACE ( 'NONE', #30660, 0.1000000000000002554, 0.003490658503988666988 ) ;
#1383 = AXIS2_PLACEMENT_3D ( 'NONE', #122480, #63559, #123118 ) ;
#1385 = DIRECTION ( 'NONE',  ( 0.000000000000000000, 0.000000000000000000, 1.000000000000000000 ) ) ;
#1386 = ORIENTED_EDGE ( 'NONE', *, *, #66111, .T. ) ;
#1387 = EDGE_LOOP ( 'NONE', ( #28668, #87934 ) ) ;
#1389 = EDGE_LOOP ( 'NONE', ( #22240, #45904, #119155, #304 ) ) ;
#1388 = ADVANCED_FACE ( 'NONE', ( #5661 ), #113747, .T. ) ;
#1390 = DIRECTION ( 'NONE',  ( 0.000000000000000000, 0.000000000000000000, 1.000000000000000000 ) ) ;
#1391 = ADVANCED_FACE ( 'NONE', ( #58515 ), #117623, .T. ) ;
#1392 = VERTEX_POINT ( 'NONE', #77482 ) ;
#1393 = AXIS2_PLACEMENT_3D ( 'NONE', #74636, #111998, #3959 ) ;
#1394 = FACE_OUTER_BOUND ( 'NONE', #6170, .T. ) ;
#1395 = DIRECTION ( 'NONE',  ( 0.000000000000000000, 0.000000000000000000, -1.000000000000000000 ) ) ;
#1396 = EDGE_CURVE ( 'NONE', #59296, #94218, #34037, .T. ) ;
#1397 = ADVANCED_FACE ( 'NONE', ( #107594 ), #84193, .T. ) ;
#1398 = EDGE_LOOP ( 'NONE', ( #37016, #92349 ) ) ;
#1399 = FACE_OUTER_BOUND ( 'NONE', #32904, .T. ) ;
#1400 = DIRECTION ( 'NONE',  ( 0.000000000000000000, 1.000000000000000000, 0.000000000000000000 ) ) ;
#1401 = EDGE_CURVE ( 'NONE', #83172, #54921, #74024, .T. ) ;
#1402 = CARTESIAN_POINT ( 'NONE',  ( -12.94999999999999218, 2.500000000000000000, -2.165063509461099489 ) ) ;
#1403 = CARTESIAN_POINT ( 'NONE',  ( 14.34999999999989662, 2.500000000000000000, 2.411473670974873862 ) ) ;
#1404 = ADVANCED_FACE ( 'NONE', ( #99070 ), #28396, .T. ) ;
#1405 = DIRECTION ( 'NONE',  ( 0.000000000000000000, 1.000000000000000000, 0.000000000000000000 ) ) ;
#1406 = VERTEX_POINT ( 'NONE', #48679 ) ;
#1407 = ORIENTED_EDGE ( 'NONE', *, *, #69792, .F. ) ;
#1408 = LINE ( 'NONE', #59721, #100806 ) ;
#1409 = CIRCLE ( 'NONE', #128988, 0.06509327318403745899 ) ;
#1410 = CARTESIAN_POINT ( 'NONE',  ( 183.8906250003414016, 0.000000000000000000, 7.564683531250000925 ) ) ;
#1411 = AXIS2_PLACEMENT_3D ( 'NONE', #95661, #26921, #115942 ) ;
#1412 = CARTESIAN_POINT ( 'NONE',  ( -9.600000000000008527, 12.50000000000000000, -4.330127018922197202 ) ) ;
#1413 = DIRECTION ( 'NONE',  ( -0.000000000000000000, 1.000000000000000000, -0.000000000000000000 ) ) ;
#1414 = ORIENTED_EDGE ( 'NONE', *, *, #64492, .T. ) ;
#1415 = AXIS2_PLACEMENT_3D ( 'NONE', #22542, #51359, #62463 ) ;
#1416 = ORIENTED_EDGE ( 'NONE', *, *, #126850, .F. ) ;
#1417 = LINE ( 'NONE', #79984, #45970 ) ;
#1418 = DIRECTION ( 'NONE',  ( 0.000000000000000000, 1.000000000000000000, 0.000000000000000000 ) ) ;
#1419 = AXIS2_PLACEMENT_3D ( 'NONE', #65191, #103861, #123481 ) ;
#1420 = CARTESIAN_POINT ( 'NONE',  ( 8.349999999999919709, 2.500000000000000000, -1.572243186433550211 ) ) ;
#1421 = CIRCLE ( 'NONE', #53663, 0.06509327318403745899 ) ;
#1422 = ORIENTED_EDGE ( 'NONE', *, *, #217, .F. ) ;
#1423 = DIRECTION ( 'NONE',  ( -0.000000000000000000, 1.000000000000000000, -0.000000000000000000 ) ) ;
#1424 = VECTOR ( 'NONE', #85113, 1000.000000000000000 ) ;
#1425 = DIRECTION ( 'NONE',  ( 0.000000000000000000, 1.000000000000000000, 0.000000000000000000 ) ) ;
#1426 = ORIENTED_EDGE ( 'NONE', *, *, #123113, .T. ) ;
#1427 = CARTESIAN_POINT ( 'NONE',  ( -2.700000000000029932, 2.500000000000000000, -4.676537180435977881 ) ) ;
#1428 = EDGE_LOOP ( 'NONE', ( #20451, #119614 ) ) ;
#1430 = FACE_OUTER_BOUND ( 'NONE', #106469, .T. ) ;
#1429 = CIRCLE ( 'NONE', #51631, 0.06509327318403745899 ) ;
#1431 = ORIENTED_EDGE ( 'NONE', *, *, #49770, .T. ) ;
#1432 = ADVANCED_FACE ( 'NONE', ( #79438 ), #869, .T. ) ;
#1434 = CIRCLE ( 'NONE', #59973, 0.06509327318403745899 ) ;
#1433 = VECTOR ( 'NONE', #68469, 1000.000000000000000 ) ;
#1435 = VERTEX_POINT ( 'NONE', #1495 ) ;
#1436 = CARTESIAN_POINT ( 'NONE',  ( -8.150000000000012790, 12.50000000000000000, -2.511473670974877948 ) ) ;
#1437 = CARTESIAN_POINT ( 'NONE',  ( 3.299999999999944755, 2.500000000000000000, -4.330127018922201643 ) ) ;
#1438 = ADVANCED_FACE ( 'NONE', ( #51907 ), #34338, .T. ) ;
#1439 = ORIENTED_EDGE ( 'NONE', *, *, #63482, .T. ) ;
#1440 = EDGE_LOOP ( 'NONE', ( #100464, #41406 ) ) ;
#1441 = CARTESIAN_POINT ( 'NONE',  ( 4.149999999999941735, 2.500000000000000000, -1.472243186433550122 ) ) ;
#1442 = DIRECTION ( 'NONE',  ( 0.000000000000000000, -0.9999939076577903929, 0.003490651415223739937 ) ) ;
#1443 = EDGE_LOOP ( 'NONE', ( #44686, #21921 ) ) ;
#1444 = CARTESIAN_POINT ( 'NONE',  ( 3.349999999999942801, 2.500000000000000000, 2.957883832488649389 ) ) ;
#1445 = CARTESIAN_POINT ( 'NONE',  ( 186.1093750003413732, 9.264065473108010111E-16, -7.564683531250000925 ) ) ;
#1446 = CARTESIAN_POINT ( 'NONE',  ( 13.74999999999989342, 2.500000000000000000, -1.572243186433550211 ) ) ;
#1447 = LINE ( 'NONE', #102858, #84868 ) ;
#1448 = CARTESIAN_POINT ( 'NONE',  ( -3.950000000000024603, 2.500000000000000000, -2.411473670974877859 ) ) ;
#1449 = DIRECTION ( 'NONE',  ( 0.000000000000000000, 0.000000000000000000, -1.000000000000000000 ) ) ;
#1450 = LINE ( 'NONE', #70843, #115246 ) ;
#1451 = EDGE_LOOP ( 'NONE', ( #103006, #91378 ) ) ;
#1452 = EDGE_LOOP ( 'NONE', ( #64604, #82814 ) ) ;
#1453 = CARTESIAN_POINT ( 'NONE',  ( -13.29999999999998828, 2.500000000000000000, 4.430127018922196847 ) ) ;
#1454 = ORIENTED_EDGE ( 'NONE', *, *, #49195, .T. ) ;
#1455 = LINE ( 'NONE', #100942, #43379 ) ;
#1456 = CARTESIAN_POINT ( 'NONE',  ( 2.299999999999949640, 2.500000000000000000, -0.3464101615137782364 ) ) ;
#1457 = DIRECTION ( 'NONE',  ( 0.000000000000000000, 1.000000000000000000, 0.000000000000000000 ) ) ;
#1459 = EDGE_LOOP ( 'NONE', ( #125884, #66672 ) ) ;
#1458 = ORIENTED_EDGE ( 'NONE', *, *, #2203, .T. ) ;
#1460 = FACE_BOUND ( 'NONE', #57391, .T. ) ;
#1461 = ORIENTED_EDGE ( 'NONE', *, *, #128440, .T. ) ;
#1462 = DIRECTION ( 'NONE',  ( 0.000000000000000000, 1.000000000000000000, 0.000000000000000000 ) ) ;
#1463 = DIRECTION ( 'NONE',  ( 0.000000000000000000, -0.9999939076577903929, 0.003490651415223739937 ) ) ;
#1464 = DIRECTION ( 'NONE',  ( 0.000000000000000000, 1.000000000000000000, 0.000000000000000000 ) ) ;
#1465 = CARTESIAN_POINT ( 'NONE',  ( -9.150000000000005684, 2.500000000000000000, 6.595190528383296780 ) ) ;
#1466 = CARTESIAN_POINT ( 'NONE',  ( -8.749999999999975131, 12.50000000000000000, 2.099970236277060032 ) ) ;
#1467 = CIRCLE ( 'NONE', #124818, 0.1000000000000002554 ) ;
#1468 = CARTESIAN_POINT ( 'NONE',  ( 6.849999999999929479, 2.500000000000000000, -2.511473670974877948 ) ) ;
#1469 = DIRECTION ( 'NONE',  ( -0.000000000000000000, -1.000000000000000000, -0.000000000000000000 ) ) ;
#1470 = CARTESIAN_POINT ( 'NONE',  ( -3.150000000000033218, 12.50000000000000000, -6.841600689897078702 ) ) ;
#1471 = CARTESIAN_POINT ( 'NONE',  ( -8.150000000000009237, 12.50000000000000000, 6.083687093685482772 ) ) ;
#1472 = LINE ( 'NONE', #21116, #128183 ) ;
#1473 = DIRECTION ( 'NONE',  ( 0.000000000000000000, 0.000000000000000000, -1.000000000000000000 ) ) ;
#1475 = AXIS2_PLACEMENT_3D ( 'NONE', #13618, #73199, #90902 ) ;
#1474 = AXIS2_PLACEMENT_3D ( 'NONE', #28142, #117777, #65470 ) ;
#1476 = EDGE_CURVE ( 'NONE', #5550, #44934, #23863, .T. ) ;
#1477 = ORIENTED_EDGE ( 'NONE', *, *, #31433, .F. ) ;
#1478 = VERTEX_POINT ( 'NONE', #10649 ) ;
#1479 = EDGE_LOOP ( 'NONE', ( #86829, #111611, #47767, #112960 ) ) ;
#1480 = ORIENTED_EDGE ( 'NONE', *, *, #104369, .F. ) ;
#1481 = CARTESIAN_POINT ( 'NONE',  ( -8.300000000000011369, 12.50000000000000000, -4.330127018922201643 ) ) ;
#1482 = DIRECTION ( 'NONE',  ( 0.000000000000000000, 0.000000000000000000, -1.000000000000000000 ) ) ;
#1484 = ORIENTED_EDGE ( 'NONE', *, *, #47971, .T. ) ;
#1483 = ORIENTED_EDGE ( 'NONE', *, *, #1655, .F. ) ;
#1485 = ORIENTED_EDGE ( 'NONE', *, *, #41052, .F. ) ;
#1486 = CARTESIAN_POINT ( 'NONE',  ( -13.54999999999999005, 2.500000000000000000, -1.918653347947324006 ) ) ;
#1488 = AXIS2_PLACEMENT_3D ( 'NONE', #13005, #52966, #92904 ) ;
#1487 = CONICAL_SURFACE ( 'NONE', #74645, 0.1000000000000002554, 0.003490658503988666988 ) ;
#1489 = AXIS2_PLACEMENT_3D ( 'NONE', #12709, #100466, #89990 ) ;
#1490 = DIRECTION ( 'NONE',  ( 0.000000000000000000, 1.000000000000000000, 0.000000000000000000 ) ) ;
#1491 = DIRECTION ( 'NONE',  ( 0.000000000000000000, 0.000000000000000000, 1.000000000000000000 ) ) ;
#1492 = CARTESIAN_POINT ( 'NONE',  ( -6.250000000000019540, 2.500000000000000000, -2.857883832488653741 ) ) ;
#1493 = LINE ( 'NONE', #31616, #118766 ) ;
#1494 = EDGE_CURVE ( 'NONE', #126431, #111547, #44793, .T. ) ;
#1495 = CARTESIAN_POINT ( 'NONE',  ( 11.64999999999990798, 2.500000000000000000, 7.088010851410848190 ) ) ;
#1496 = ADVANCED_FACE ( 'NONE', ( #72828 ), #116493, .T. ) ;
#1497 = ORIENTED_EDGE ( 'NONE', *, *, #44549, .T. ) ;
#1498 = DIRECTION ( 'NONE',  ( -0.000000000000000000, -1.000000000000000000, -0.000000000000000000 ) ) ;
#1499 = ORIENTED_EDGE ( 'NONE', *, *, #101448, .T. ) ;
#1500 = VERTEX_POINT ( 'NONE', #81371 ) ;
#1501 = VERTEX_POINT ( 'NONE', #122575 ) ;
#1502 = DIRECTION ( 'NONE',  ( 0.000000000000000000, 1.000000000000000000, 0.000000000000000000 ) ) ;
#1503 = ORIENTED_EDGE ( 'NONE', *, *, #53326, .T. ) ;
#1504 = EDGE_CURVE ( 'NONE', #20597, #48724, #112756, .T. ) ;
#1505 = EDGE_LOOP ( 'NONE', ( #86966, #46034, #1880, #27546 ) ) ;
#1506 = ORIENTED_EDGE ( 'NONE', *, *, #14929, .T. ) ;
#1507 = VECTOR ( 'NONE', #92268, 1000.000000000000000 ) ;
#1508 =( NAMED_UNIT ( * ) SI_UNIT ( $, .STERADIAN. ) SOLID_ANGLE_UNIT ( ) );
#1510 = AXIS2_PLACEMENT_3D ( 'NONE', #129124, #37509, #47321 ) ;
#1509 = DIRECTION ( 'NONE',  ( -0.000000000000000000, -1.000000000000000000, -0.000000000000000000 ) ) ;
#1511 = CARTESIAN_POINT ( 'NONE',  ( -11.84999999999999787, 2.500000000000000000, -6.741600689897073728 ) ) ;
#1512 = DIRECTION ( 'NONE',  ( 0.000000000000000000, 0.000000000000000000, 1.000000000000000000 ) ) ;
#1513 = DIRECTION ( 'NONE',  ( -0.000000000000000000, -1.000000000000000000, -0.000000000000000000 ) ) ;
#1514 = CIRCLE ( 'NONE', #72635, 0.1000000000000002554 ) ;
#1516 = AXIS2_PLACEMENT_3D ( 'NONE', #4333, #11604, #122217 ) ;
#1515 = FACE_OUTER_BOUND ( 'NONE', #37511, .T. ) ;
#1517 = ORIENTED_EDGE ( 'NONE', *, *, #114538, .T. ) ;
#1518 = CONICAL_SURFACE ( 'NONE', #26667, 0.1000000000000002554, 0.003490658503988666988 ) ;
#1519 = DIRECTION ( 'NONE',  ( 0.000000000000000000, -0.000000000000000000, 1.000000000000000000 ) ) ;
#1520 = EDGE_LOOP ( 'NONE', ( #101696, #91460 ) ) ;
#1521 = CARTESIAN_POINT ( 'NONE',  ( 7.099999999999928590, 12.50000000000000000, 3.572213422710607489 ) ) ;
#1522 = CARTESIAN_POINT ( 'NONE',  ( 0.1999999999999576006, 12.50000000000000000, -4.676537180435978769 ) ) ;
#1523 = VERTEX_POINT ( 'NONE', #110178 ) ;
#1524 = DIRECTION ( 'NONE',  ( -0.000000000000000000, -1.000000000000000000, -0.000000000000000000 ) ) ;
#1525 = VERTEX_POINT ( 'NONE', #861 ) ;
#1526 = DIRECTION ( 'NONE',  ( 0.000000000000000000, 0.000000000000000000, 1.000000000000000000 ) ) ;
#1527 = EDGE_CURVE ( 'NONE', #13290, #20697, #51764, .T. ) ;
#1529 = AXIS2_PLACEMENT_3D ( 'NONE', #46535, #76655, #108037 ) ;
#1528 = VECTOR ( 'NONE', #99732, 1000.000000000000000 ) ;
#1530 = LINE ( 'NONE', #42115, #88478 ) ;
#1531 = EDGE_LOOP ( 'NONE', ( #12078, #21547 ) ) ;
#1532 = ORIENTED_EDGE ( 'NONE', *, *, #68147, .T. ) ;
#1533 = DIRECTION ( 'NONE',  ( 0.000000000000000000, 0.000000000000000000, -1.000000000000000000 ) ) ;
#1534 = CARTESIAN_POINT ( 'NONE',  ( 8.549999999999924327, 2.500000000000000000, 1.718653347947321386 ) ) ;
#1535 = EDGE_CURVE ( 'NONE', #118142, #30008, #5758, .T. ) ;
#1536 = CARTESIAN_POINT ( 'NONE',  ( 184.2552083336747444, 6.551208109652275624, -3.782341765624998686 ) ) ;
#1537 = FACE_OUTER_BOUND ( 'NONE', #100316, .T. ) ;
#1538 = EDGE_CURVE ( 'NONE', #39278, #122805, #62234, .T. ) ;
#1539 = CARTESIAN_POINT ( 'NONE',  ( -8.350000000000008527, 2.500000000000000000, 5.802370205355744659 ) ) ;
#1540 = ORIENTED_EDGE ( 'NONE', *, *, #125339, .T. ) ;
#1541 = DIRECTION ( 'NONE',  ( 0.000000000000000000, 0.000000000000000000, 1.000000000000000000 ) ) ;
#1542 = EDGE_CURVE ( 'NONE', #54932, #127552, #45513, .T. ) ;
#1543 = ADVANCED_FACE ( 'NONE', ( #71524 ), #92454, .T. ) ;
#1544 = EDGE_CURVE ( 'NONE', #109083, #54236, #103992, .T. ) ;
#1545 = VECTOR ( 'NONE', #55567, 1000.000000000000000 ) ;
#1546 = EDGE_CURVE ( 'NONE', #22099, #41508, #14081, .T. ) ;
#1547 = EDGE_LOOP ( 'NONE', ( #100115, #18678, #20513, #77162 ) ) ;
#1548 = FACE_OUTER_BOUND ( 'NONE', #17091, .T. ) ;
#1549 = DIRECTION ( 'NONE',  ( -0.000000000000000000, -1.000000000000000000, -0.000000000000000000 ) ) ;
#1550 = EDGE_CURVE ( 'NONE', #29645, #16079, #47561, .T. ) ;
#1551 = CARTESIAN_POINT ( 'NONE',  ( 187.1302083336747444, -4.367472073101514418, -7.564683531250002702 ) ) ;
#1552 = DIRECTION ( 'NONE',  ( 0.000000000000000000, 0.000000000000000000, 1.000000000000000000 ) ) ;
#1553 = DIRECTION ( 'NONE',  ( 0.000000000000000000, 0.000000000000000000, 1.000000000000000000 ) ) ;
#1554 = DIRECTION ( 'NONE',  ( 0.000000000000000000, 1.000000000000000000, 0.000000000000000000 ) ) ;
#1555 = CARTESIAN_POINT ( 'NONE',  ( 14.14999999999989733, 2.500000000000000000, 1.472243186433545459 ) ) ;
#1556 = VERTEX_POINT ( 'NONE', #62373 ) ;
#1557 = EDGE_CURVE ( 'NONE', #14107, #20554, #61063, .T. ) ;
#1558 = AXIS2_PLACEMENT_3D ( 'NONE', #75074, #73772, #3117 ) ;
#1559 = DIRECTION ( 'NONE',  ( -0.000000000000000000, -1.000000000000000000, -0.000000000000000000 ) ) ;
#1560 = AXIS2_PLACEMENT_3D ( 'NONE', #83976, #123908, #36197 ) ;
#1561 = CARTESIAN_POINT ( 'NONE',  ( -7.500000000000015099, 2.500000000000000000, -0.5928203230275541635 ) ) ;
#1562 = DIRECTION ( 'NONE',  ( 0.000000000000000000, 1.000000000000000000, 0.000000000000000000 ) ) ;
#1563 = ORIENTED_EDGE ( 'NONE', *, *, #37850, .F. ) ;
#1565 = AXIS2_PLACEMENT_3D ( 'NONE', #35225, #114402, #14883 ) ;
#1564 = CONICAL_SURFACE ( 'NONE', #112308, 0.09999999999999982514, 0.003490658503988666988 ) ;
#1566 = CARTESIAN_POINT ( 'NONE',  ( -4.150000000000027889, 12.50000000000000000, -6.495190528383302464 ) ) ;
#1567 = VECTOR ( 'NONE', #124513, 1000.000000000000000 ) ;
#1568 = ORIENTED_EDGE ( 'NONE', *, *, #103239, .F. ) ;
#1569 = ORIENTED_EDGE ( 'NONE', *, *, #59789, .F. ) ;
#1570 = FACE_OUTER_BOUND ( 'NONE', #73684, .T. ) ;
#1571 = ORIENTED_EDGE ( 'NONE', *, *, #47825, .T. ) ;
#1572 = CARTESIAN_POINT ( 'NONE',  ( 17.84432265422648101, -2.533187527837326591, -5.021315468710856322 ) ) ;
#1573 = DIRECTION ( 'NONE',  ( 0.000000000000000000, 0.000000000000000000, 1.000000000000000000 ) ) ;
#1574 = AXIS2_PLACEMENT_3D ( 'NONE', #16025, #34421, #5561 ) ;
#1575 = ORIENTED_EDGE ( 'NONE', *, *, #38640, .F. ) ;
#1576 = AXIS2_PLACEMENT_3D ( 'NONE', #57161, #97090, #7402 ) ;
#1577 = CARTESIAN_POINT ( 'NONE',  ( -6.450000000000019718, 2.500000000000000000, -6.148780366869526226 ) ) ;
#1578 = CARTESIAN_POINT ( 'NONE',  ( -12.09999999999999609, 12.50000000000000000, -5.022947341949751454 ) ) ;
#1579 = EDGE_LOOP ( 'NONE', ( #111478, #116715, #36521, #1047 ) ) ;
#1580 = VECTOR ( 'NONE', #61651, 1000.000000000000000 ) ;
#1582 = ORIENTED_EDGE ( 'NONE', *, *, #116388, .F. ) ;
#1581 = ADVANCED_FACE ( 'NONE', ( #32926 ), #124918, .T. ) ;
#1583 = EDGE_LOOP ( 'NONE', ( #10309, #54978, #30149, #12881 ) ) ;
#1584 = DIRECTION ( 'NONE',  ( 0.000000000000000000, 1.000000000000000000, 0.000000000000000000 ) ) ;
#1585 = CARTESIAN_POINT ( 'NONE',  ( -3.100000000000028511, 2.500000000000000000, -3.883716857408426648 ) ) ;
#1586 = CARTESIAN_POINT ( 'NONE',  ( 11.89999999999990443, 12.50000000000000000, -0.2813168883297408329 ) ) ;
#1587 = FACE_BOUND ( 'NONE', #51323, .T. ) ;
#1588 = EDGE_LOOP ( 'NONE', ( #64511, #122818 ) ) ;
#1589 = VECTOR ( 'NONE', #37866, 1000.000000000000000 ) ;
#1590 = DIRECTION ( 'NONE',  ( -0.000000000000000000, 1.000000000000000000, -0.000000000000000000 ) ) ;
#1591 = DIRECTION ( 'NONE',  ( -0.000000000000000000, -1.000000000000000000, -0.000000000000000000 ) ) ;
#1592 = AXIS2_PLACEMENT_3D ( 'NONE', #107180, #7685, #89484 ) ;
#1593 = ORIENTED_EDGE ( 'NONE', *, *, #83190, .F. ) ;
#1594 = EDGE_CURVE ( 'NONE', #122488, #118638, #63003, .T. ) ;
#1595 = CARTESIAN_POINT ( 'NONE',  ( -10.80000000000000249, 2.500000000000000000, -4.330127018922197202 ) ) ;
#1596 = PLANE ( 'NONE',  #9499 ) ;
#1597 = AXIS2_PLACEMENT_3D ( 'NONE', #6212, #114251, #85435 ) ;
#1598 = CARTESIAN_POINT ( 'NONE',  ( 9.349999999999916156, 2.500000000000000000, 6.148780366869520009 ) ) ;
#1599 = LINE ( 'NONE', #84023, #42958 ) ;
#1600 = CARTESIAN_POINT ( 'NONE',  ( -9.600000000000006750, 12.50000000000000000, -0.6277270498435167934 ) ) ;
#1601 = LINE ( 'NONE', #110277, #88988 ) ;
#1602 = VECTOR ( 'NONE', #125277, 1000.000000000000000 ) ;
#1603 = FACE_OUTER_BOUND ( 'NONE', #60406, .T. ) ;
#1604 = AXIS2_PLACEMENT_3D ( 'NONE', #112241, #63791, #103716 ) ;
#1605 = CIRCLE ( 'NONE', #43490, 0.06509327318403745899 ) ;
#1606 = ORIENTED_EDGE ( 'NONE', *, *, #4797, .T. ) ;
#1607 = ORIENTED_EDGE ( 'NONE', *, *, #89892, .T. ) ;
#1608 = ORIENTED_EDGE ( 'NONE', *, *, #108778, .F. ) ;
#1609 = VERTEX_POINT ( 'NONE', #93120 ) ;
#1610 = LINE ( 'NONE', #90645, #91377 ) ;
#1611 = CARTESIAN_POINT ( 'NONE',  ( 12.69999999999990337, 2.500000000000000000, 3.983716857408420076 ) ) ;
#1612 = VECTOR ( 'NONE', #128044, 1000.000000000000000 ) ;
#1613 = ORIENTED_EDGE ( 'NONE', *, *, #16015, .T. ) ;
#1614 = FACE_BOUND ( 'NONE', #122207, .T. ) ;
#1615 = CARTESIAN_POINT ( 'NONE',  ( -10.60000000000000320, 12.50000000000000000, -3.983716857408421852 ) ) ;
#1616 = CARTESIAN_POINT ( 'NONE',  ( 1.049999999999953637, 12.50000000000000000, -1.818653347947326138 ) ) ;
#1617 = DIRECTION ( 'NONE',  ( -0.9961946980917455452, -1.067350013832299517E-17, 0.08715574274765836016 ) ) ;
#1619 = AXIS2_PLACEMENT_3D ( 'NONE', #126509, #36204, #55191 ) ;
#1618 = AXIS2_PLACEMENT_3D ( 'NONE', #115980, #104231, #44031 ) ;
#1620 = CARTESIAN_POINT ( 'NONE',  ( -4.550000000000022915, 2.500000000000000000, 2.165063509461097713 ) ) ;
#1621 = CARTESIAN_POINT ( 'NONE',  ( -8.100000000000013856, 2.500000000000000000, -0.3464101615137782364 ) ) ;
#1622 = CARTESIAN_POINT ( 'NONE',  ( 7.699999999999922018, 2.500000000000000000, 0.3464101615137735735 ) ) ;
#1624 = CARTESIAN_POINT ( 'NONE',  ( -2.950000000000030376, 2.500000000000000000, 6.495190528383297135 ) ) ;
#1623 =( BOUNDED_SURFACE ( )  B_SPLINE_SURFACE ( 2, 3, ( 
 ( #37303, #126319, #127607, #77848 ),
 ( #77220, #117759, #88972, #57590 ),
 ( #28117, #56277, #107966, #128268 ),
 ( #47125, #88302, #96194, #6499 ),
 ( #26830, #86382, #58865, #9118 ) ),
 .UNSPECIFIED., .F., .F., .F. ) 
 B_SPLINE_SURFACE_WITH_KNOTS ( ( 3, 2, 3 ),
 ( 4, 4 ),
 ( 0.000000000000000000, 1.000000000000000000, 1.133771318130139871 ),
 ( -0.0002500000000000000052, 0.005250000000000000326 ),
 .UNSPECIFIED. ) 
 GEOMETRIC_REPRESENTATION_ITEM ( )  RATIONAL_B_SPLINE_SURFACE ( (
 ( 1.000000000000000000, 1.000000000000000000, 1.000000000000000000, 1.000000000000000000),
 ( 0.7071067811865475727, 0.7071067811865475727, 0.7071067811865475727, 0.7071067811865475727),
 ( 1.000000000000000000, 1.000000000000000000, 1.000000000000000000, 1.000000000000000000),
 ( 1.000000000000000000, 1.000000000000000000, 1.000000000000000000, 1.000000000000000000),
 ( 1.000000000000000000, 1.000000000000000000, 1.000000000000000000, 1.000000000000000000) ) ) 
 REPRESENTATION_ITEM ( '' )  SURFACE ( )  );
#1625 = CARTESIAN_POINT ( 'NONE',  ( -1.450000000000035039, 12.50000000000000000, -6.841600689897077814 ) ) ;
#1626 = CARTESIAN_POINT ( 'NONE',  ( -0.4000000000000339950, 2.500000000000000000, 0.7928203230275517877 ) ) ;
#1627 = ORIENTED_EDGE ( 'NONE', *, *, #19572, .F. ) ;
#1628 = EDGE_LOOP ( 'NONE', ( #87048, #126957, #21833, #6855 ) ) ;
#1629 = EDGE_CURVE ( 'NONE', #101564, #44902, #5358, .T. ) ;
#1631 = ORIENTED_EDGE ( 'NONE', *, *, #14352, .T. ) ;
#1630 = B_SPLINE_CURVE_WITH_KNOTS ( 'NONE', 3,
 ( #25452, #14975, #54922, #124969, #75216, #57521, #49000, #29997, #90167, #9042, #69914, #78465, #28706, #127544, #88911, #98707, #118358, #8396, #60112, #20165, #98075, #88229, #67964, #97429, #107895, #48336, #68611, #7755, #89547, #100021, #10342, #128193, #50275, #507, #108546, #49645, #128861, #129506 ),
 .UNSPECIFIED., .F., .F.,
 ( 4, 2, 2, 2, 2, 2, 2, 2, 2, 2, 2, 2, 2, 2, 2, 2, 2, 2, 4 ),
 ( 0.000000000000000000, 0.001007299096406573174, 0.002014598192813146348, 0.003021897289219719306, 0.004029196385626292697, 0.005036495482032866088, 0.006043794578439438611, 0.007051093674846012002, 0.008058392771252585393, 0.008562042319455872089, 0.009065691867659158784, 0.01007299096406573218, 0.01108029006047230557, 0.01208758915687887722, 0.01309488825328545061, 0.01410218734969202400, 0.01510948644609859740, 0.01561313599430188409, 0.01611678554250517079 ),
 .UNSPECIFIED. ) ;
#1632 = ORIENTED_EDGE ( 'NONE', *, *, #12805, .F. ) ;
#1633 = ORIENTED_EDGE ( 'NONE', *, *, #80465, .F. ) ;
#1634 = ORIENTED_EDGE ( 'NONE', *, *, #126096, .F. ) ;
#1635 = DIRECTION ( 'NONE',  ( 0.000000000000000000, 1.000000000000000000, 0.000000000000000000 ) ) ;
#1636 = ORIENTED_EDGE ( 'NONE', *, *, #31142, .F. ) ;
#1637 = EDGE_CURVE ( 'NONE', #74213, #62109, #45309, .T. ) ;
#1638 = DIRECTION ( 'NONE',  ( 0.000000000000000000, 0.000000000000000000, 1.000000000000000000 ) ) ;
#1639 = DIRECTION ( 'NONE',  ( -0.000000000000000000, 1.000000000000000000, -0.000000000000000000 ) ) ;
#1640 = CARTESIAN_POINT ( 'NONE',  ( 2.099999999999949463, 2.500000000000000000, -3.637306695894650055 ) ) ;
#1641 = DIRECTION ( 'NONE',  ( 0.000000000000000000, 0.000000000000000000, -1.000000000000000000 ) ) ;
#1643 = ADVANCED_FACE ( 'NONE', ( #54464 ), #122771, .T. ) ;
#1642 = CIRCLE ( 'NONE', #129227, 0.06509327318403743123 ) ;
#1644 = ADVANCED_FACE ( 'NONE', ( #105512 ), #87241, .T. ) ;
#1645 = VERTEX_POINT ( 'NONE', #4694 ) ;
#1646 = CARTESIAN_POINT ( 'NONE',  ( -6.450000000000019718, 2.500000000000000000, -1.818653347947326138 ) ) ;
#1647 = CONICAL_SURFACE ( 'NONE', #85278, 0.1000000000000002554, 0.003490658503988666988 ) ;
#1648 = EDGE_LOOP ( 'NONE', ( #39907, #129114, #125910, #101323 ) ) ;
#1649 = AXIS2_PLACEMENT_3D ( 'NONE', #79969, #87202, #98968 ) ;
#1650 = ORIENTED_EDGE ( 'NONE', *, *, #89470, .F. ) ;
#1651 = DIRECTION ( 'NONE',  ( -0.000000000000000000, -1.000000000000000000, -0.000000000000000000 ) ) ;
#1652 = EDGE_CURVE ( 'NONE', #36694, #85926, #95692, .T. ) ;
#1653 = CARTESIAN_POINT ( 'NONE',  ( -12.89999999999999147, 12.50000000000000000, 4.330127018922196314 ) ) ;
#1654 = DIRECTION ( 'NONE',  ( -0.000000000000000000, 1.000000000000000000, -0.000000000000000000 ) ) ;
#1655 = EDGE_CURVE ( 'NONE', #124666, #40568, #58027, .T. ) ;
#1656 = EDGE_LOOP ( 'NONE', ( #124418, #42763 ) ) ;
#1658 = ORIENTED_EDGE ( 'NONE', *, *, #93470, .T. ) ;
#1657 = AXIS2_PLACEMENT_3D ( 'NONE', #58736, #98635, #88830 ) ;
#1659 = CARTESIAN_POINT ( 'NONE',  ( 0.8499999999999553468, 12.50000000000000000, -2.165063509461101710 ) ) ;
#1660 = DIRECTION ( 'NONE',  ( -0.000000000000000000, 1.000000000000000000, -0.000000000000000000 ) ) ;
#1661 = DIRECTION ( 'NONE',  ( 0.000000000000000000, 0.000000000000000000, 1.000000000000000000 ) ) ;
#1662 = CARTESIAN_POINT ( 'NONE',  ( 8.349999999999919709, 12.50000000000000000, -1.407149913249512663 ) ) ;
#1663 = ORIENTED_EDGE ( 'NONE', *, *, #28422, .T. ) ;
#1664 = DIRECTION ( 'NONE',  ( 0.000000000000000000, 0.000000000000000000, -1.000000000000000000 ) ) ;
#1665 = ORIENTED_EDGE ( 'NONE', *, *, #99190, .F. ) ;
#1666 = CARTESIAN_POINT ( 'NONE',  ( 14.93723468728801507, -2.499999999999999112, 6.174425104148753896 ) ) ;
#1667 = AXIS2_PLACEMENT_3D ( 'NONE', #84534, #74072, #104798 ) ;
#1668 = ORIENTED_EDGE ( 'NONE', *, *, #111949, .T. ) ;
#1669 = DIRECTION ( 'NONE',  ( -0.000000000000000000, -1.000000000000000000, -0.000000000000000000 ) ) ;
#1670 = DIRECTION ( 'NONE',  ( 0.000000000000000000, -0.9999939076577903929, 0.003490651415223739937 ) ) ;
#1671 = CARTESIAN_POINT ( 'NONE',  ( -8.749999999999975131, 2.500000000000000000, 2.265063509461097357 ) ) ;
#1672 = AXIS2_PLACEMENT_3D ( 'NONE', #78183, #118088, #59192 ) ;
#1673 = DIRECTION ( 'NONE',  ( 0.000000000000000000, 1.000000000000000000, 0.000000000000000000 ) ) ;
#1674 = DIRECTION ( 'NONE',  ( 0.000000000000000000, 0.000000000000000000, 1.000000000000000000 ) ) ;
#1675 = ORIENTED_EDGE ( 'NONE', *, *, #80020, .T. ) ;
#1677 = AXIS2_PLACEMENT_3D ( 'NONE', #116368, #37191, #26716 ) ;
#1676 = DIRECTION ( 'NONE',  ( -0.000000000000000000, 1.000000000000000000, -0.000000000000000000 ) ) ;
#1678 =( GEOMETRIC_REPRESENTATION_CONTEXT ( 3 ) GLOBAL_UNCERTAINTY_ASSIGNED_CONTEXT ( ( #101904 ) ) GLOBAL_UNIT_ASSIGNED_CONTEXT ( ( #110801, #83298, #46567 ) ) REPRESENTATION_CONTEXT ( 'NONE', 'WORKASPACE' ) );
#1679 = PLANE ( 'NONE',  #46523 ) ;
#1680 = EDGE_LOOP ( 'NONE', ( #122884, #69929 ) ) ;
#1681 = ORIENTED_EDGE ( 'NONE', *, *, #117977, .F. ) ;
#1682 = EDGE_LOOP ( 'NONE', ( #119202, #20973, #82004, #126348 ) ) ;
#1683 = CARTESIAN_POINT ( 'NONE',  ( 17.50000000000000000, -0.9166666666666696273, 2.864912725862981624 ) ) ;
#1684 = DIRECTION ( 'NONE',  ( -0.000000000000000000, -1.000000000000000000, -0.000000000000000000 ) ) ;
#1685 = FACE_OUTER_BOUND ( 'NONE', #10697, .T. ) ;
#1686 = AXIS2_PLACEMENT_3D ( 'NONE', #69594, #89239, #129198 ) ;
#1688 = CIRCLE ( 'NONE', #7950, 0.1000000000000002554 ) ;
#1687 = CARTESIAN_POINT ( 'NONE',  ( -8.750000000000008882, 2.500000000000000000, -2.957883832488653830 ) ) ;
#1690 = EDGE_CURVE ( 'NONE', #55973, #54643, #125147, .T. ) ;
#1689 = CARTESIAN_POINT ( 'NONE',  ( -3.642919299551294898E-14, 2.500000000000000000, 0.7928203230275517877 ) ) ;
#1691 = CARTESIAN_POINT ( 'NONE',  ( -11.69999999999999929, 2.500000000000000000, -4.430127018922199511 ) ) ;
#1692 = DIRECTION ( 'NONE',  ( 0.000000000000000000, 0.000000000000000000, -1.000000000000000000 ) ) ;
#1693 = CARTESIAN_POINT ( 'NONE',  ( 8.349999999999923261, 12.50000000000000000, 1.537336459617582918 ) ) ;
#1694 = EDGE_CURVE ( 'NONE', #129065, #13310, #26621, .T. ) ;
#1695 = EDGE_CURVE ( 'NONE', #119558, #2346, #9897, .T. ) ;
#1696 = AXIS2_PLACEMENT_3D ( 'NONE', #73430, #112734, #94360 ) ;
#1697 = EDGE_CURVE ( 'NONE', #68225, #38667, #93754, .T. ) ;
#1698 = EDGE_CURVE ( 'NONE', #109625, #1000, #112399, .T. ) ;
#1699 = EDGE_LOOP ( 'NONE', ( #70879, #8956 ) ) ;
#1700 = EDGE_CURVE ( 'NONE', #92524, #46914, #3635, .T. ) ;
#1701 = DIRECTION ( 'NONE',  ( -0.000000000000000000, 1.000000000000000000, -0.000000000000000000 ) ) ;
#1702 = VECTOR ( 'NONE', #67936, 1000.000000000000000 ) ;
#1703 = DIRECTION ( 'NONE',  ( 0.000000000000000000, 0.000000000000000000, 1.000000000000000000 ) ) ;
#1704 = DIRECTION ( 'NONE',  ( 0.000000000000000000, 0.000000000000000000, -1.000000000000000000 ) ) ;
#1705 = CARTESIAN_POINT ( 'NONE',  ( -11.84999999999999787, 12.50000000000000000, -2.511473670974873951 ) ) ;
#1706 = ORIENTED_EDGE ( 'NONE', *, *, #57819, .F. ) ;
#1707 = ADVANCED_FACE ( 'NONE', ( #4071 ), #49719, .T. ) ;
#1708 = CARTESIAN_POINT ( 'NONE',  ( -8.350000000000013856, 2.500000000000000000, -5.702370205355745014 ) ) ;
#1711 = ADVANCED_FACE ( 'NONE', ( #44019 ), #106040, .T. ) ;
#1710 = AXIS2_PLACEMENT_3D ( 'NONE', #52444, #93668, #4603 ) ;
#1709 = CIRCLE ( 'NONE', #22666, 0.06509327318403745899 ) ;
#1712 = CARTESIAN_POINT ( 'NONE',  ( 13.29999999999990301, 2.500000000000000000, 4.230127018922196669 ) ) ;
#1714 = ORIENTED_EDGE ( 'NONE', *, *, #69909, .F. ) ;
#1713 = CARTESIAN_POINT ( 'NONE',  ( 13.54999999999989946, 2.500000000000000000, 2.411473670974873862 ) ) ;
#1715 = EDGE_LOOP ( 'NONE', ( #99532, #98552, #53633, #123665 ) ) ;
#1716 = DIRECTION ( 'NONE',  ( -0.000000000000000000, -1.000000000000000000, -0.000000000000000000 ) ) ;
#1717 = EDGE_LOOP ( 'NONE', ( #7917, #95060 ) ) ;
#1718 = ORIENTED_EDGE ( 'NONE', *, *, #67888, .T. ) ;
#1719 = CARTESIAN_POINT ( 'NONE',  ( -10.80000000000000071, 2.500000000000000000, 4.230127018922196669 ) ) ;
#1720 = VECTOR ( 'NONE', #87234, 1000.000000000000000 ) ;
#1721 = ADVANCED_FACE ( 'NONE', ( #73456 ), #65573, .T. ) ;
#1722 = CARTESIAN_POINT ( 'NONE',  ( 20.64614705759136015, 2.669560853936051803, -2.247897417617913618 ) ) ;
#1723 = FACE_OUTER_BOUND ( 'NONE', #80418, .T. ) ;
#1724 = DIRECTION ( 'NONE',  ( 0.000000000000000000, 1.000000000000000000, 0.000000000000000000 ) ) ;
#1725 = VERTEX_POINT ( 'NONE', #125763 ) ;
#1726 = CIRCLE ( 'NONE', #116747, 0.1000000000000002554 ) ;
#1727 = VECTOR ( 'NONE', #90995, 1000.000000000000000 ) ;
#1728 = AXIS2_PLACEMENT_3D ( 'NONE', #37888, #80405, #128217 ) ;
#1729 = FACE_OUTER_BOUND ( 'NONE', #112827, .T. ) ;
#1730 = VERTEX_POINT ( 'NONE', #36125 ) ;
#1731 = CARTESIAN_POINT ( 'NONE',  ( -2.050000000000033129, 12.50000000000000000, 2.230156782645134950 ) ) ;
#1732 = DIRECTION ( 'NONE',  ( 0.000000000000000000, 1.000000000000000000, 0.000000000000000000 ) ) ;
#1733 = VERTEX_POINT ( 'NONE', #24369 ) ;
#1734 = CONICAL_SURFACE ( 'NONE', #10164, 0.1000000000000002554, 0.003490658503988666988 ) ;
#1735 = AXIS2_PLACEMENT_3D ( 'NONE', #124187, #66542, #114358 ) ;
#1736 = ORIENTED_EDGE ( 'NONE', *, *, #62762, .F. ) ;
#1737 = ORIENTED_EDGE ( 'NONE', *, *, #92849, .T. ) ;
#1738 = VERTEX_POINT ( 'NONE', #26310 ) ;
#1739 = LINE ( 'NONE', #90113, #23146 ) ;
#1740 = CARTESIAN_POINT ( 'NONE',  ( 15.22989033368257950, 2.499999999999486633, 7.180069491320466568 ) ) ;
#1741 = DIRECTION ( 'NONE',  ( 0.000000000000000000, 1.000000000000000000, 0.000000000000000000 ) ) ;
#1742 = FACE_BOUND ( 'NONE', #81437, .T. ) ;
#1743 = ORIENTED_EDGE ( 'NONE', *, *, #72468, .F. ) ;
#1744 = CARTESIAN_POINT ( 'NONE',  ( -12.29999999999999538, 2.500000000000000000, -4.676537180435976104 ) ) ;
#1745 = CARTESIAN_POINT ( 'NONE',  ( 187.1510416670080303, 4.367472073101518859, -7.564683531249999149 ) ) ;
#1746 = CIRCLE ( 'NONE', #85383, 0.06509327318403745899 ) ;
#1747 = CARTESIAN_POINT ( 'NONE',  ( 13.14999999999990088, 2.500000000000000000, 2.511473670974873507 ) ) ;
#1748 = CARTESIAN_POINT ( 'NONE',  ( 1.049999999999954969, 2.500000000000000000, -6.941600689897077459 ) ) ;
#1749 = EDGE_CURVE ( 'NONE', #29970, #98422, #85199, .T. ) ;
#1750 = AXIS2_PLACEMENT_3D ( 'NONE', #14406, #116475, #75914 ) ;
#1751 = CARTESIAN_POINT ( 'NONE',  ( -3.750000000000025757, 12.50000000000000000, 1.472243186433545459 ) ) ;
#1752 = FACE_OUTER_BOUND ( 'NONE', #45837, .T. ) ;
#1753 = FACE_OUTER_BOUND ( 'NONE', #56528, .T. ) ;
#1754 = AXIS2_PLACEMENT_3D ( 'NONE', #92929, #123026, #44456 ) ;
#1755 = DIRECTION ( 'NONE',  ( 0.000000000000000000, 1.000000000000000000, 0.000000000000000000 ) ) ;
#1756 = EDGE_LOOP ( 'NONE', ( #44364, #81307 ) ) ;
#1757 = VERTEX_POINT ( 'NONE', #14525 ) ;
#1758 = EDGE_LOOP ( 'NONE', ( #81359, #118787, #83378, #9902 ) ) ;
#1759 = ORIENTED_EDGE ( 'NONE', *, *, #85925, .F. ) ;
#1760 = VERTEX_POINT ( 'NONE', #23732 ) ;
#1761 = VECTOR ( 'NONE', #57075, 1000.000000000000000 ) ;
#1762 = CARTESIAN_POINT ( 'NONE',  ( -14.39999999999998614, 2.500000000000000000, -0.2464101615137760659 ) ) ;
#1763 = CARTESIAN_POINT ( 'NONE',  ( -13.54999999999998828, 12.50000000000000000, 1.818653347947325472 ) ) ;
#1764 = VERTEX_POINT ( 'NONE', #56391 ) ;
#1765 = FACE_BOUND ( 'NONE', #79748, .T. ) ;
#1766 = CARTESIAN_POINT ( 'NONE',  ( -3.550000000000027356, 2.500000000000000000, -2.411473670974877859 ) ) ;
#1767 = AXIS2_PLACEMENT_3D ( 'NONE', #111146, #61445, #101361 ) ;
#1768 = ORIENTED_EDGE ( 'NONE', *, *, #14795, .F. ) ;
#1769 = DIRECTION ( 'NONE',  ( 0.000000000000000000, 0.000000000000000000, 1.000000000000000000 ) ) ;
#1770 = DIRECTION ( 'NONE',  ( 0.000000000000000000, 0.000000000000000000, -1.000000000000000000 ) ) ;
#1771 = FACE_OUTER_BOUND ( 'NONE', #67507, .T. ) ;
#1772 = CARTESIAN_POINT ( 'NONE',  ( -1.900000000000034550, 2.500000000000000000, 4.676537180435972552 ) ) ;
#1773 = EDGE_LOOP ( 'NONE', ( #63223, #58049, #57994, #59182 ) ) ;
#1774 = CIRCLE ( 'NONE', #72812, 0.06509327318403745899 ) ;
#1775 = FACE_OUTER_BOUND ( 'NONE', #66052, .T. ) ;
#1776 = VERTEX_POINT ( 'NONE', #113382 ) ;
#1777 = EDGE_LOOP ( 'NONE', ( #30067, #66294, #114054, #128798 ) ) ;
#1778 = DIRECTION ( 'NONE',  ( 0.000000000000000000, 1.000000000000000000, 0.000000000000000000 ) ) ;
#1779 = CARTESIAN_POINT ( 'NONE',  ( -7.700000000000014388, 2.500000000000000000, -4.576537180435977348 ) ) ;
#1780 = AXIS2_PLACEMENT_3D ( 'NONE', #75355, #96278, #24978 ) ;
#1781 = EDGE_LOOP ( 'NONE', ( #12829, #105421 ) ) ;
#1782 = DIRECTION ( 'NONE',  ( 0.000000000000000000, 0.000000000000000000, 1.000000000000000000 ) ) ;
#1783 = ADVANCED_FACE ( 'NONE', ( #63659 ), #47886, .F. ) ;
#1784 = CARTESIAN_POINT ( 'NONE',  ( 6.049999999999934097, 12.50000000000000000, -2.576566944158915184 ) ) ;
#1785 = CARTESIAN_POINT ( 'NONE',  ( -10.45000000000000107, 2.500000000000000000, 2.165063509461097713 ) ) ;
#1786 = DIRECTION ( 'NONE',  ( 0.000000000000000000, 0.000000000000000000, -1.000000000000000000 ) ) ;
#1787 = CARTESIAN_POINT ( 'NONE',  ( -10.65000000000000391, 2.500000000000000000, -6.941600689897075682 ) ) ;
#1788 = VERTEX_POINT ( 'NONE', #17753 ) ;
#1789 = AXIS2_PLACEMENT_3D ( 'NONE', #105785, #58630, #46212 ) ;
#1790 = ADVANCED_FACE ( 'NONE', ( #99565 ), #109366, .T. ) ;
#1791 = FACE_OUTER_BOUND ( 'NONE', #48669, .T. ) ;
#1792 = EDGE_CURVE ( 'NONE', #118832, #51819, #89409, .T. ) ;
#1793 = ORIENTED_EDGE ( 'NONE', *, *, #105090, .T. ) ;
#1794 = FACE_OUTER_BOUND ( 'NONE', #102906, .T. ) ;
#1796 = AXIS2_PLACEMENT_3D ( 'NONE', #33307, #73216, #83679 ) ;
#1795 = CIRCLE ( 'NONE', #18534, 0.06509327318403745899 ) ;
#1797 = ORIENTED_EDGE ( 'NONE', *, *, #33724, .F. ) ;
#1798 = DIRECTION ( 'NONE',  ( -0.000000000000000000, -1.000000000000000000, -0.000000000000000000 ) ) ;
#1799 = EDGE_LOOP ( 'NONE', ( #33142, #114576, #21469, #104478 ) ) ;
#1800 = CARTESIAN_POINT ( 'NONE',  ( -10.60000000000000142, 12.50000000000000000, 4.741630453620009789 ) ) ;
#1801 = FACE_OUTER_BOUND ( 'NONE', #20259, .T. ) ;
#1802 = EDGE_CURVE ( 'NONE', #54180, #54197, #83071, .T. ) ;
#1803 = EDGE_CURVE ( 'NONE', #83051, #56486, #37096, .T. ) ;
#1804 = DIRECTION ( 'NONE',  ( 0.000000000000000000, 1.000000000000000000, 0.000000000000000000 ) ) ;
#1805 = EDGE_CURVE ( 'NONE', #101014, #844, #53807, .T. ) ;
#1806 = DIRECTION ( 'NONE',  ( 0.000000000000000000, -0.9999939076577903929, 0.003490651415223739937 ) ) ;
#1807 = ADVANCED_FACE ( 'NONE', ( #127715 ), #14171, .T. ) ;
#1808 = CARTESIAN_POINT ( 'NONE',  ( 11.24999999999994493, 12.50000000000000000, 6.495190528383297135 ) ) ;
#1809 = ORIENTED_EDGE ( 'NONE', *, *, #114284, .F. ) ;
#1810 = ORIENTED_EDGE ( 'NONE', *, *, #2599, .F. ) ;
#1811 = ORIENTED_EDGE ( 'NONE', *, *, #13485, .F. ) ;
#1812 = DIRECTION ( 'NONE',  ( 0.000000000000000000, 0.000000000000000000, -1.000000000000000000 ) ) ;
#1813 = DIRECTION ( 'NONE',  ( 0.000000000000000000, 0.000000000000000000, -1.000000000000000000 ) ) ;
#1814 = CARTESIAN_POINT ( 'NONE',  ( -3.550000000000027356, 12.50000000000000000, -2.576566944158915184 ) ) ;
#1817 = ORIENTED_EDGE ( 'NONE', *, *, #121797, .F. ) ;
#1816 = ORIENTED_EDGE ( 'NONE', *, *, #52997, .F. ) ;
#1815 = AXIS2_PLACEMENT_3D ( 'NONE', #38514, #27358, #107869 ) ;
#1818 = EDGE_LOOP ( 'NONE', ( #77084, #103594, #92488, #80314 ) ) ;
#1819 = ADVANCED_FACE ( 'NONE', ( #89728 ), #48520, .F. ) ;
#1820 = DIRECTION ( 'NONE',  ( 0.000000000000000000, 0.000000000000000000, 1.000000000000000000 ) ) ;
#1821 = ORIENTED_EDGE ( 'NONE', *, *, #128507, .F. ) ;
#1822 = CARTESIAN_POINT ( 'NONE',  ( -9.350000000000008527, 12.50000000000000000, -6.776507416713035248 ) ) ;
#1823 = DIRECTION ( 'NONE',  ( -0.000000000000000000, 1.000000000000000000, -0.000000000000000000 ) ) ;
#1824 = AXIS2_PLACEMENT_3D ( 'NONE', #98141, #100092, #38610 ) ;
#1826 = DIRECTION ( 'NONE',  ( -0.000000000000000000, 1.000000000000000000, -0.000000000000000000 ) ) ;
#1825 = AXIS2_PLACEMENT_3D ( 'NONE', #10072, #109562, #128584 ) ;
#1827 = LINE ( 'NONE', #19541, #104599 ) ;
#1828 = AXIS2_PLACEMENT_3D ( 'NONE', #23389, #53520, #13569 ) ;
#1829 = DIRECTION ( 'NONE',  ( 0.000000000000000000, -0.9999939076577903929, 0.003490651415223739937 ) ) ;
#1830 = FACE_OUTER_BOUND ( 'NONE', #82276, .T. ) ;
#1831 = CARTESIAN_POINT ( 'NONE',  ( -10.00000000000000355, 2.500000000000000000, -0.7928203230275542301 ) ) ;
#1832 = FACE_OUTER_BOUND ( 'NONE', #114504, .T. ) ;
#1833 = VECTOR ( 'NONE', #105501, 1000.000000000000000 ) ;
#1834 = ORIENTED_EDGE ( 'NONE', *, *, #103239, .T. ) ;
#1835 = CONICAL_SURFACE ( 'NONE', #106387, 0.09999999999999999167, 0.003490658503988666988 ) ;
#1837 = PLANE ( 'NONE',  #36128 ) ;
#1836 = VECTOR ( 'NONE', #90045, 1000.000000000000000 ) ;
#1838 = CARTESIAN_POINT ( 'NONE',  ( 34.93074629416160803, -2.900242961800562291, 4.640733549227246790 ) ) ;
#1839 = EDGE_LOOP ( 'NONE', ( #128772, #75940 ) ) ;
#1840 = ORIENTED_EDGE ( 'NONE', *, *, #49030, .T. ) ;
#1841 = CARTESIAN_POINT ( 'NONE',  ( 186.2968750003414584, 8.734944146203032389, 5.348610694689227483E-16 ) ) ;
#1842 = FACE_OUTER_BOUND ( 'NONE', #82318, .T. ) ;
#1843 = CARTESIAN_POINT ( 'NONE',  ( -2.500000000000030642, 2.500000000000000000, -0.7928203230275542301 ) ) ;
#1844 = AXIS2_PLACEMENT_3D ( 'NONE', #18655, #118793, #59252 ) ;
#1845 = DIRECTION ( 'NONE',  ( 0.000000000000000000, 0.000000000000000000, 1.000000000000000000 ) ) ;
#1846 = DIRECTION ( 'NONE',  ( -4.274815082592931898E-19, -0.9999939076577903929, -0.003490651415223739937 ) ) ;
#1847 = DIRECTION ( 'NONE',  ( 0.000000000000000000, 0.000000000000000000, -1.000000000000000000 ) ) ;
#1848 = CARTESIAN_POINT ( 'NONE',  ( -6.250000000000017764, 2.500000000000000000, 7.188010851410848723 ) ) ;
#1849 = DIRECTION ( 'NONE',  ( 0.000000000000000000, -0.9999939076577903929, 0.003490651415223739937 ) ) ;
#1850 = EDGE_CURVE ( 'NONE', #55993, #39292, #57031, .T. ) ;
#1851 = ADVANCED_FACE ( 'NONE', ( #96964 ), #7287, .T. ) ;
#1852 = DIRECTION ( 'NONE',  ( 0.000000000000000000, 0.000000000000000000, 1.000000000000000000 ) ) ;
#1853 = VERTEX_POINT ( 'NONE', #28239 ) ;
#1854 = ORIENTED_EDGE ( 'NONE', *, *, #97187, .T. ) ;
#1855 = ADVANCED_FACE ( 'NONE', ( #7934 ), #43454, .T. ) ;
#1856 = ORIENTED_EDGE ( 'NONE', *, *, #13373, .F. ) ;
#1857 = CIRCLE ( 'NONE', #35332, 0.06509327318403745899 ) ;
#1858 = ORIENTED_EDGE ( 'NONE', *, *, #51957, .T. ) ;
#1859 = ADVANCED_FACE ( 'NONE', ( #77970 ), #8568, .T. ) ;
#1860 = DIRECTION ( 'NONE',  ( 0.000000000000000000, 0.000000000000000000, -1.000000000000000000 ) ) ;
#1861 = CYLINDRICAL_SURFACE ( 'NONE', #39546, 7.700000000000000178 ) ;
#1862 = EDGE_CURVE ( 'NONE', #97069, #24036, #116601, .T. ) ;
#1863 = VERTEX_POINT ( 'NONE', #28888 ) ;
#1864 = EDGE_CURVE ( 'NONE', #54180, #45787, #68800, .T. ) ;
#1865 = CARTESIAN_POINT ( 'NONE',  ( 127.5000000000000000, 0.000000000000000000, 0.000000000000000000 ) ) ;
#1866 = FACE_OUTER_BOUND ( 'NONE', #20948, .T. ) ;
#1867 = EDGE_CURVE ( 'NONE', #79959, #108868, #98899, .T. ) ;
#1868 = VECTOR ( 'NONE', #100532, 1000.000000000000000 ) ;
#1869 = CARTESIAN_POINT ( 'NONE',  ( 12.69999999999990337, 2.500000000000000000, 3.883716857408420431 ) ) ;
#1871 = EDGE_LOOP ( 'NONE', ( #54821, #36111 ) ) ;
#1870 = DIRECTION ( 'NONE',  ( -4.274815082592931898E-19, -0.9999939076577903929, -0.003490651415223739937 ) ) ;
#1872 = DIRECTION ( 'NONE',  ( 0.000000000000000000, -0.9999939076577903929, 0.003490651415223739937 ) ) ;
#1873 = VECTOR ( 'NONE', #114832, 1000.000000000000000 ) ;
#1874 = ADVANCED_FACE ( 'NONE', ( #89092 ), #9986, .T. ) ;
#1875 = DIRECTION ( 'NONE',  ( 0.000000000000000000, 1.000000000000000000, 0.000000000000000000 ) ) ;
#1876 = ORIENTED_EDGE ( 'NONE', *, *, #111837, .F. ) ;
#1877 = AXIS2_PLACEMENT_3D ( 'NONE', #47145, #7843, #37961 ) ;
#1878 = ORIENTED_EDGE ( 'NONE', *, *, #68368, .F. ) ;
#1879 = ORIENTED_EDGE ( 'NONE', *, *, #103961, .T. ) ;
#1880 = ORIENTED_EDGE ( 'NONE', *, *, #12323, .T. ) ;
#1881 = CARTESIAN_POINT ( 'NONE',  ( -9.400000000000007461, 2.500000000000000000, 4.676537180435972552 ) ) ;
#1882 = CIRCLE ( 'NONE', #43681, 0.06509327318403741736 ) ;
#1883 = CARTESIAN_POINT ( 'NONE',  ( -0.8000000000000381251, 12.50000000000000000, 4.330127018922196314 ) ) ;
#1884 = CARTESIAN_POINT ( 'NONE',  ( 8.299999999999922551, 12.50000000000000000, -2.385244779468109755E-15 ) ) ;
#1885 = ORIENTED_EDGE ( 'NONE', *, *, #34709, .T. ) ;
#1887 = VECTOR ( 'NONE', #113154, 1000.000000000000000 ) ;
#1886 = VECTOR ( 'NONE', #79946, 1000.000000000000000 ) ;
#1888 = CARTESIAN_POINT ( 'NONE',  ( 10.44999999999991047, 12.50000000000000000, 2.165063509461097713 ) ) ;
#1889 = VERTEX_POINT ( 'NONE', #49825 ) ;
#1890 = LINE ( 'NONE', #52294, #110239 ) ;
#1892 = CONICAL_SURFACE ( 'NONE', #75062, 0.1000000000000002554, 0.003490658503988666988 ) ;
#1891 = CARTESIAN_POINT ( 'NONE',  ( 6.649999999999931966, 2.500000000000000000, -7.188010851410854052 ) ) ;
#1893 = FACE_OUTER_BOUND ( 'NONE', #63778, .T. ) ;
#1894 = CARTESIAN_POINT ( 'NONE',  ( 21.15177371151418839, -2.593223176056364210, 4.151029080743465549 ) ) ;
#1895 = ADVANCED_FACE ( 'NONE', ( #41292 ), #60181, .T. ) ;
#1896 = ORIENTED_EDGE ( 'NONE', *, *, #27117, .T. ) ;
#1898 = CIRCLE ( 'NONE', #116905, 0.1000000000000002554 ) ;
#1897 = CIRCLE ( 'NONE', #102263, 0.09999999999999982514 ) ;
#1899 = VERTEX_POINT ( 'NONE', #81209 ) ;
#1900 = VERTEX_POINT ( 'NONE', #52 ) ;
#1901 = DIRECTION ( 'NONE',  ( -4.274815082592931898E-19, -0.9999939076577903929, -0.003490651415223739937 ) ) ;
#1902 = DIRECTION ( 'NONE',  ( 0.000000000000000000, 0.000000000000000000, 1.000000000000000000 ) ) ;
#1903 = FACE_BOUND ( 'NONE', #74197, .T. ) ;
#1904 = DIRECTION ( 'NONE',  ( -0.000000000000000000, -1.000000000000000000, -0.000000000000000000 ) ) ;
#1905 = LINE ( 'NONE', #43796, #79948 ) ;
#1906 = LINE ( 'NONE', #41223, #91776 ) ;
#1907 = EDGE_CURVE ( 'NONE', #93919, #96281, #3719, .T. ) ;
#1908 = CARTESIAN_POINT ( 'NONE',  ( 0.8499999999999557909, 12.50000000000000000, -6.495190528383302464 ) ) ;
#1909 = DIRECTION ( 'NONE',  ( 0.000000000000000000, -0.9999939076577903929, 0.003490651415223739937 ) ) ;
#1910 = CARTESIAN_POINT ( 'NONE',  ( -11.25000000000000000, 12.50000000000000000, 7.188010851410848723 ) ) ;
#1911 = ORIENTED_EDGE ( 'NONE', *, *, #8933, .T. ) ;
#1912 = CARTESIAN_POINT ( 'NONE',  ( -13.94999999999998685, 2.500000000000000000, 1.818653347947325472 ) ) ;
#1913 = CONICAL_SURFACE ( 'NONE', #73026, 0.1000000000000000472, 0.003490658503988666988 ) ;
#1914 = CONICAL_SURFACE ( 'NONE', #68823, 0.1000000000000000472, 0.003490658503988666988 ) ;
#1915 = CARTESIAN_POINT ( 'NONE',  ( 2.949999999999943334, 2.500000000000000000, 6.495190528383297135 ) ) ;
#1916 = EDGE_LOOP ( 'NONE', ( #32518, #36802 ) ) ;
#1917 = ORIENTED_EDGE ( 'NONE', *, *, #91979, .T. ) ;
#1918 = DIRECTION ( 'NONE',  ( -0.000000000000000000, 1.000000000000000000, -0.000000000000000000 ) ) ;
#1919 = EDGE_CURVE ( 'NONE', #121644, #26032, #51747, .T. ) ;
#1920 = DIRECTION ( 'NONE',  ( -0.000000000000000000, 1.000000000000000000, -0.000000000000000000 ) ) ;
#1921 = FACE_BOUND ( 'NONE', #34728, .T. ) ;
#1922 = CARTESIAN_POINT ( 'NONE',  ( 7.049999999999926992, 2.500000000000000000, 2.265063509461097357 ) ) ;
#1923 = CIRCLE ( 'NONE', #123123, 0.09999999999999982514 ) ;
#1924 = AXIS2_PLACEMENT_3D ( 'NONE', #114998, #124843, #3777 ) ;
#1925 = AXIS2_PLACEMENT_3D ( 'NONE', #19700, #117881, #28232 ) ;
#1926 = EDGE_LOOP ( 'NONE', ( #31248, #128784 ) ) ;
#1927 = CARTESIAN_POINT ( 'NONE',  ( 6.899999999999928413, 12.50000000000000000, 4.676537180435972552 ) ) ;
#1928 = CARTESIAN_POINT ( 'NONE',  ( 185.4583333333333144, 4.445597072760117285, 7.699999999999999289 ) ) ;
#1929 = AXIS2_PLACEMENT_3D ( 'NONE', #81457, #102386, #61166 ) ;
#1930 = ORIENTED_EDGE ( 'NONE', *, *, #113657, .F. ) ;
#1931 = CARTESIAN_POINT ( 'NONE',  ( -13.14999999999999147, 2.500000000000000000, 1.818653347947325472 ) ) ;
#1932 = PLANE ( 'NONE',  #55460 ) ;
#1933 = VECTOR ( 'NONE', #87660, 1000.000000000000000 ) ;
#1934 = EDGE_LOOP ( 'NONE', ( #126264, #112449 ) ) ;
#1935 = DIRECTION ( 'NONE',  ( 0.000000000000000000, 0.000000000000000000, 1.000000000000000000 ) ) ;
#1936 = FACE_OUTER_BOUND ( 'NONE', #34415, .T. ) ;
#1937 = ORIENTED_EDGE ( 'NONE', *, *, #30650, .F. ) ;
#1938 = ADVANCED_FACE ( 'NONE', ( #81831 ), #7918, .T. ) ;
#1939 = LINE ( 'NONE', #90311, #82223 ) ;
#1940 = CARTESIAN_POINT ( 'NONE',  ( -15.39999999999997904, 12.50000000000000000, -0.06509327318403743123 ) ) ;
#1941 = CARTESIAN_POINT ( 'NONE',  ( 175.5000000000000000, 0.000000000000000000, 0.000000000000000000 ) ) ;
#1942 = AXIS2_PLACEMENT_3D ( 'NONE', #45673, #115030, #116960 ) ;
#1943 = EDGE_LOOP ( 'NONE', ( #79197, #1963, #90048, #4280 ) ) ;
#1944 = EDGE_LOOP ( 'NONE', ( #6201, #74544, #26451, #49616 ) ) ;
#1945 = DIRECTION ( 'NONE',  ( 0.000000000000000000, -0.9999939076577903929, 0.003490651415223739937 ) ) ;
#1946 = EDGE_CURVE ( 'NONE', #118122, #5223, #20455, .T. ) ;
#1947 = ORIENTED_EDGE ( 'NONE', *, *, #126529, .F. ) ;
#1948 = CARTESIAN_POINT ( 'NONE',  ( 14.59999999999989484, 2.500000000000000000, 0.6928203230275494784 ) ) ;
#1949 = CARTESIAN_POINT ( 'NONE',  ( 11.24999999999990763, 2.500000000000000000, -7.288010851410854585 ) ) ;
#1950 = DIRECTION ( 'NONE',  ( -0.000000000000000000, 1.000000000000000000, -0.000000000000000000 ) ) ;
#1951 = EDGE_LOOP ( 'NONE', ( #35179, #119082 ) ) ;
#1952 = LINE ( 'NONE', #55582, #72543 ) ;
#1953 = DIRECTION ( 'NONE',  ( 0.000000000000000000, 0.000000000000000000, -1.000000000000000000 ) ) ;
#1954 = CARTESIAN_POINT ( 'NONE',  ( -6.850000000000017408, 2.500000000000000000, -6.741600689897077281 ) ) ;
#1955 = EDGE_CURVE ( 'NONE', #42274, #129541, #12445, .T. ) ;
#1956 = EDGE_CURVE ( 'NONE', #7039, #31303, #74832, .T. ) ;
#1957 = DIRECTION ( 'NONE',  ( 0.000000000000000000, 0.000000000000000000, 1.000000000000000000 ) ) ;
#1958 = DIRECTION ( 'NONE',  ( 0.000000000000000000, 1.000000000000000000, 0.000000000000000000 ) ) ;
#1959 = ADVANCED_FACE ( 'NONE', ( #40659 ), #110026, .T. ) ;
#1960 = ADVANCED_FACE ( 'NONE', ( #80568 ), #104080, .T. ) ;
#1961 = CONICAL_SURFACE ( 'NONE', #83468, 0.1000000000000002554, 0.003490658503988666988 ) ;
#1962 = CARTESIAN_POINT ( 'NONE',  ( -10.80000000000000071, 2.500000000000000000, -2.276824562219559311E-15 ) ) ;
#1963 = ORIENTED_EDGE ( 'NONE', *, *, #82838, .F. ) ;
#1964 = VERTEX_POINT ( 'NONE', #61578 ) ;
#1965 = PLANE ( 'NONE',  #20225 ) ;
#1966 = ORIENTED_EDGE ( 'NONE', *, *, #68617, .F. ) ;
#1967 = CARTESIAN_POINT ( 'NONE',  ( 103.0694403040216400, 7.655046866769239955, 0.8471574321703054800 ) ) ;
#1969 = VERTEX_POINT ( 'NONE', #22303 ) ;
#1968 = EDGE_LOOP ( 'NONE', ( #32474, #90546, #56776, #69502 ) ) ;
#1970 = ORIENTED_EDGE ( 'NONE', *, *, #23266, .T. ) ;
#1971 = VECTOR ( 'NONE', #36293, 1000.000000000000000 ) ;
#1972 = EDGE_CURVE ( 'NONE', #59884, #29149, #122425, .T. ) ;
#1973 = FACE_OUTER_BOUND ( 'NONE', #96621, .T. ) ;
#1974 = ADVANCED_FACE ( 'NONE', ( #102133 ), #95199, .T. ) ;
#1975 = CARTESIAN_POINT ( 'NONE',  ( -4.350000000000023626, 12.50000000000000000, 6.841600689897072485 ) ) ;
#1976 = EDGE_CURVE ( 'NONE', #29091, #11967, #22049, .T. ) ;
#1977 = CARTESIAN_POINT ( 'NONE',  ( -4.550000000000022915, 2.500000000000000000, -2.065063509461102065 ) ) ;
#1978 =( LENGTH_UNIT ( ) NAMED_UNIT ( * ) SI_UNIT ( .MILLI., .METRE. ) );
#1979 = VECTOR ( 'NONE', #7005, 1000.000000000000000 ) ;
#1980 = DIRECTION ( 'NONE',  ( 0.000000000000000000, -0.000000000000000000, 1.000000000000000000 ) ) ;
#1981 = FACE_OUTER_BOUND ( 'NONE', #28031, .T. ) ;
#1982 = CARTESIAN_POINT ( 'NONE',  ( -4.800000000000024691, 2.500000000000000000, 0.2464101615137735679 ) ) ;
#1983 = CARTESIAN_POINT ( 'NONE',  ( 8.349999999999919709, 2.500000000000000000, -2.165063509461101710 ) ) ;
#1984 = LINE ( 'NONE', #3287, #46618 ) ;
#1985 = AXIS2_PLACEMENT_3D ( 'NONE', #76175, #47358, #75510 ) ;
#1986 = PRODUCT_RELATED_PRODUCT_CATEGORY ( 'part', '', ( #33622 ) ) ;
#1987 = DIRECTION ( 'NONE',  ( 0.000000000000000000, 0.000000000000000000, 1.000000000000000000 ) ) ;
#1989 = CIRCLE ( 'NONE', #106542, 0.1000000000000002554 ) ;
#1988 = AXIS2_PLACEMENT_3D ( 'NONE', #48885, #88791, #39075 ) ;
#1990 = ORIENTED_EDGE ( 'NONE', *, *, #37165, .T. ) ;
#1991 = CARTESIAN_POINT ( 'NONE',  ( 9.549999999999918998, 12.50000000000000000, -6.495190528383302464 ) ) ;
#1992 = EDGE_LOOP ( 'NONE', ( #83331, #6563, #5558, #78744 ) ) ;
#1993 = VERTEX_POINT ( 'NONE', #32772 ) ;
#1994 = CARTESIAN_POINT ( 'NONE',  ( -9.350000000000008527, 2.500000000000000000, -6.148780366869520897 ) ) ;
#1995 = DIRECTION ( 'NONE',  ( -0.000000000000000000, 1.000000000000000000, -0.000000000000000000 ) ) ;
#1996 = DIRECTION ( 'NONE',  ( -0.000000000000000000, -1.000000000000000000, -0.000000000000000000 ) ) ;
#1997 = CARTESIAN_POINT ( 'NONE',  ( -12.29999999999999538, 12.50000000000000000, 4.676537180435972552 ) ) ;
#1998 = DIRECTION ( 'NONE',  ( -0.000000000000000000, 1.000000000000000000, -0.000000000000000000 ) ) ;
#1999 = DIRECTION ( 'NONE',  ( 0.000000000000000000, 0.000000000000000000, -1.000000000000000000 ) ) ;
#2001 = CONICAL_SURFACE ( 'NONE', #118989, 0.1000000000000000056, 0.003490658503988666988 ) ;
#2000 = DIRECTION ( 'NONE',  ( 0.000000000000000000, 0.000000000000000000, 1.000000000000000000 ) ) ;
#2002 = ORIENTED_EDGE ( 'NONE', *, *, #98816, .T. ) ;
#2003 = ORIENTED_EDGE ( 'NONE', *, *, #62084, .T. ) ;
#2004 = VECTOR ( 'NONE', #262, 1000.000000000000000 ) ;
#2006 = EDGE_LOOP ( 'NONE', ( #52260, #56304 ) ) ;
#2005 = AXIS2_PLACEMENT_3D ( 'NONE', #37136, #18764, #126145 ) ;
#2007 = ORIENTED_EDGE ( 'NONE', *, *, #55189, .T. ) ;
#2008 = ADVANCED_FACE ( 'NONE', ( #72675 ), #112602, .T. ) ;
#2009 = ORIENTED_EDGE ( 'NONE', *, *, #69256, .T. ) ;
#2011 = AXIS2_PLACEMENT_3D ( 'NONE', #76092, #107487, #6042 ) ;
#2010 = LINE ( 'NONE', #81858, #10583 ) ;
#2012 = DIRECTION ( 'NONE',  ( 0.000000000000000000, 0.000000000000000000, 1.000000000000000000 ) ) ;
#2014 = CONICAL_SURFACE ( 'NONE', #75188, 0.1000000000000002554, 0.003490658503988666988 ) ;
#2013 = VECTOR ( 'NONE', #33725, 1000.000000000000000 ) ;
#2015 = ADVANCED_FACE ( 'NONE', ( #79910 ), #17816, .T. ) ;
#2016 = CARTESIAN_POINT ( 'NONE',  ( 10.59999999999990905, 12.50000000000000000, -4.676537180435978769 ) ) ;
#2017 = DIRECTION ( 'NONE',  ( -0.000000000000000000, -1.000000000000000000, -0.000000000000000000 ) ) ;
#2018 = EDGE_CURVE ( 'NONE', #110215, #88657, #24093, .T. ) ;
#2019 = DIRECTION ( 'NONE',  ( -0.000000000000000000, -1.000000000000000000, -0.000000000000000000 ) ) ;
#2020 = VERTEX_POINT ( 'NONE', #70098 ) ;
#2021 = DIRECTION ( 'NONE',  ( -0.000000000000000000, 1.000000000000000000, -0.000000000000000000 ) ) ;
#2022 = DIRECTION ( 'NONE',  ( 0.000000000000000000, 0.000000000000000000, 1.000000000000000000 ) ) ;
#2023 = CARTESIAN_POINT ( 'NONE',  ( 4.149999999999939959, 2.500000000000000000, 1.472243186433545459 ) ) ;
#2024 = LINE ( 'NONE', #30873, #24273 ) ;
#2025 = AXIS2_PLACEMENT_3D ( 'NONE', #23024, #54404, #123157 ) ;
#2026 = EDGE_CURVE ( 'NONE', #29271, #62565, #20350, .T. ) ;
#2027 = CARTESIAN_POINT ( 'NONE',  ( -0.6000000000000383915, 2.500000000000000000, -3.983716857408426293 ) ) ;
#2028 = AXIS2_PLACEMENT_3D ( 'NONE', #8140, #64017, #45034 ) ;
#2029 = ORIENTED_EDGE ( 'NONE', *, *, #71569, .T. ) ;
#2030 = VECTOR ( 'NONE', #116044, 1000.000000000000000 ) ;
#2031 = EDGE_LOOP ( 'NONE', ( #104443, #44555 ) ) ;
#2032 = ORIENTED_EDGE ( 'NONE', *, *, #21171, .T. ) ;
#2033 = DIRECTION ( 'NONE',  ( 0.000000000000000000, 0.000000000000000000, 1.000000000000000000 ) ) ;
#2034 = ORIENTED_EDGE ( 'NONE', *, *, #3891, .T. ) ;
#2035 = CIRCLE ( 'NONE', #108649, 0.1000000000000000056 ) ;
#2036 = DIRECTION ( 'NONE',  ( 0.000000000000000000, 1.000000000000000000, 0.000000000000000000 ) ) ;
#2037 = CARTESIAN_POINT ( 'NONE',  ( 2.949999999999946887, 12.50000000000000000, -6.495190528383302464 ) ) ;
#2038 = CIRCLE ( 'NONE', #62708, 0.09999999999999982514 ) ;
#2039 = EDGE_LOOP ( 'NONE', ( #78932, #71187, #48499, #34133 ) ) ;
#2040 = CARTESIAN_POINT ( 'NONE',  ( -3.749999999999991118, 2.500000000000000000, -2.165063509461101710 ) ) ;
#2041 = DIRECTION ( 'NONE',  ( 0.000000000000000000, 0.000000000000000000, 1.000000000000000000 ) ) ;
#2042 = DIRECTION ( 'NONE',  ( 0.000000000000000000, 0.000000000000000000, 1.000000000000000000 ) ) ;
#2043 = EDGE_CURVE ( 'NONE', #116823, #102121, #53346, .T. ) ;
#2044 = DIRECTION ( 'NONE',  ( 0.000000000000000000, 1.000000000000000000, 0.000000000000000000 ) ) ;
#2045 = DIRECTION ( 'NONE',  ( 0.000000000000000000, -0.000000000000000000, 1.000000000000000000 ) ) ;
#2046 = VERTEX_POINT ( 'NONE', #63497 ) ;
#2047 = ORIENTED_EDGE ( 'NONE', *, *, #103340, .F. ) ;
#2048 = DIRECTION ( 'NONE',  ( 0.000000000000000000, 0.000000000000000000, 1.000000000000000000 ) ) ;
#2049 = DIRECTION ( 'NONE',  ( 0.000000000000000000, 1.000000000000000000, 0.000000000000000000 ) ) ;
#2050 = DIRECTION ( 'NONE',  ( 0.000000000000000000, 1.000000000000000000, 0.000000000000000000 ) ) ;
#2051 = CARTESIAN_POINT ( 'NONE',  ( 6.649999999999929301, 12.50000000000000000, -2.230156782645139391 ) ) ;
#2052 = ORIENTED_EDGE ( 'NONE', *, *, #17167, .F. ) ;
#2053 = EDGE_CURVE ( 'NONE', #16443, #71159, #109772, .T. ) ;
#2054 = ORIENTED_EDGE ( 'NONE', *, *, #108201, .T. ) ;
#2056 = AXIS2_PLACEMENT_3D ( 'NONE', #75866, #74588, #114501 ) ;
#2055 = DIRECTION ( 'NONE',  ( 0.000000000000000000, 0.000000000000000000, 1.000000000000000000 ) ) ;
#2057 = CARTESIAN_POINT ( 'NONE',  ( -3.150000000000029221, 2.500000000000000000, -1.718653347947326049 ) ) ;
#2058 = DIRECTION ( 'NONE',  ( 0.000000000000000000, 0.000000000000000000, 1.000000000000000000 ) ) ;
#2059 = DIRECTION ( 'NONE',  ( 0.000000000000000000, -0.9999939076577903929, 0.003490651415223739937 ) ) ;
#2060 = EDGE_LOOP ( 'NONE', ( #72816, #22527, #87175, #90661 ) ) ;
#2061 = DIRECTION ( 'NONE',  ( -0.000000000000000000, 1.000000000000000000, -0.000000000000000000 ) ) ;
#2063 = AXIS2_PLACEMENT_3D ( 'NONE', #22709, #23318, #114286 ) ;
#2062 = VECTOR ( 'NONE', #123414, 1000.000000000000000 ) ;
#2064 = DIRECTION ( 'NONE',  ( 0.000000000000000000, 0.000000000000000000, 1.000000000000000000 ) ) ;
#2065 = ORIENTED_EDGE ( 'NONE', *, *, #105794, .F. ) ;
#2066 = DIRECTION ( 'NONE',  ( 0.000000000000000000, 0.000000000000000000, 1.000000000000000000 ) ) ;
#2067 = EDGE_CURVE ( 'NONE', #69989, #11966, #9427, .T. ) ;
#2068 = EDGE_LOOP ( 'NONE', ( #577, #22664 ) ) ;
#2069 = CARTESIAN_POINT ( 'NONE',  ( 184.5000000000000000, 0.000000000000000000, 0.000000000000000000 ) ) ;
#2071 = CIRCLE ( 'NONE', #5991, 0.06509327318403745899 ) ;
#2070 = AXIS2_PLACEMENT_3D ( 'NONE', #54502, #104260, #34251 ) ;
#2072 = ORIENTED_EDGE ( 'NONE', *, *, #96533, .F. ) ;
#2073 = DIRECTION ( 'NONE',  ( -0.000000000000000000, 1.000000000000000000, -0.000000000000000000 ) ) ;
#2074 = FACE_OUTER_BOUND ( 'NONE', #73731, .T. ) ;
#2075 = ORIENTED_EDGE ( 'NONE', *, *, #123890, .T. ) ;
#2076 = EDGE_CURVE ( 'NONE', #126002, #109254, #61763, .T. ) ;
#2077 = ORIENTED_EDGE ( 'NONE', *, *, #65642, .T. ) ;
#2078 = LINE ( 'NONE', #10597, #125064 ) ;
#2079 = DIRECTION ( 'NONE',  ( -0.000000000000000000, 1.000000000000000000, -0.000000000000000000 ) ) ;
#2080 = CARTESIAN_POINT ( 'NONE',  ( 187.3802083336747444, 4.367472073101515306, 7.564683531250000925 ) ) ;
#2081 = CARTESIAN_POINT ( 'NONE',  ( 184.7760416670080588, 6.551208109652274736, 3.782341765625001351 ) ) ;
#2082 = CARTESIAN_POINT ( 'NONE',  ( 0.000000000000000000, 2.500000000000000000, 0.000000000000000000 ) ) ;
#2083 = DIRECTION ( 'NONE',  ( -4.274815082592931898E-19, -0.9999939076577903929, -0.003490651415223739937 ) ) ;
#2084 = DIRECTION ( 'NONE',  ( -0.000000000000000000, 1.000000000000000000, -0.000000000000000000 ) ) ;
#2085 = CARTESIAN_POINT ( 'NONE',  ( -4.200000000000025935, 2.500000000000000000, 4.430127018922196847 ) ) ;
#2086 = DIRECTION ( 'NONE',  ( -0.000000000000000000, 1.000000000000000000, -0.000000000000000000 ) ) ;
#2087 = CIRCLE ( 'NONE', #98244, 0.1000000000000002554 ) ;
#2088 = CIRCLE ( 'NONE', #46039, 0.06509327318403745899 ) ;
#2089 = VERTEX_POINT ( 'NONE', #45796 ) ;
#2091 = ORIENTED_EDGE ( 'NONE', *, *, #119329, .T. ) ;
#2090 = EDGE_CURVE ( 'NONE', #56145, #82216, #19899, .T. ) ;
#2092 = DIRECTION ( 'NONE',  ( 0.000000000000000000, 0.000000000000000000, 1.000000000000000000 ) ) ;
#2093 = EDGE_LOOP ( 'NONE', ( #26547, #67364 ) ) ;
#2094 = LINE ( 'NONE', #11278, #78879 ) ;
#2095 = DIRECTION ( 'NONE',  ( -0.000000000000000000, 1.000000000000000000, -0.000000000000000000 ) ) ;
#2096 = CARTESIAN_POINT ( 'NONE',  ( 11.24999999999990941, 2.500000000000000000, 7.288010851410849256 ) ) ;
#2098 = VERTEX_POINT ( 'NONE', #55605 ) ;
#2097 = ORIENTED_EDGE ( 'NONE', *, *, #86362, .T. ) ;
#2099 = FACE_BOUND ( 'NONE', #82400, .T. ) ;
#2100 = EDGE_LOOP ( 'NONE', ( #12731, #84755, #61103, #86237 ) ) ;
#2101 = CARTESIAN_POINT ( 'NONE',  ( -7.050000000000016698, 2.500000000000000000, -6.495190528383302464 ) ) ;
#2102 = DIRECTION ( 'NONE',  ( 0.000000000000000000, 0.000000000000000000, -1.000000000000000000 ) ) ;
#2103 = AXIS2_PLACEMENT_3D ( 'NONE', #1888, #117953, #109928 ) ;
#2105 = ADVANCED_FACE ( 'NONE', ( #13732 ), #114512, .T. ) ;
#2104 = LINE ( 'NONE', #93725, #17844 ) ;
#2106 = DIRECTION ( 'NONE',  ( 0.000000000000000000, -0.9999939076577903929, 0.003490651415223739937 ) ) ;
#2107 = CARTESIAN_POINT ( 'NONE',  ( -14.34999999999998543, 2.500000000000000000, -1.818653347947323695 ) ) ;
#2108 = FACE_OUTER_BOUND ( 'NONE', #7305, .T. ) ;
#2109 = PLANE ( 'NONE',  #51899 ) ;
#2110 = CARTESIAN_POINT ( 'NONE',  ( -6.050000000000022027, 12.50000000000000000, -1.818653347947326138 ) ) ;
#2111 = EDGE_CURVE ( 'NONE', #114814, #54801, #54954, .T. ) ;
#2112 = ADVANCED_FACE ( 'NONE', ( #94884 ), #42900, .T. ) ;
#2113 = DIRECTION ( 'NONE',  ( 0.000000000000000000, 0.000000000000000000, 1.000000000000000000 ) ) ;
#2114 = CARTESIAN_POINT ( 'NONE',  ( 0.3999999999999568345, 12.50000000000000000, -5.088040615133791356 ) ) ;
#2115 = ADVANCED_FACE ( 'NONE', ( #5198 ), #13609, .T. ) ;
#2117 = EDGE_CURVE ( 'NONE', #59989, #16485, #36632, .T. ) ;
#2116 = AXIS2_PLACEMENT_3D ( 'NONE', #32554, #1129, #12858 ) ;
#2118 = DIRECTION ( 'NONE',  ( -0.000000000000000000, -1.000000000000000000, -0.000000000000000000 ) ) ;
#2119 = AXIS2_PLACEMENT_3D ( 'NONE', #116659, #105564, #7342 ) ;
#2120 = ORIENTED_EDGE ( 'NONE', *, *, #123129, .F. ) ;
#2121 = EDGE_LOOP ( 'NONE', ( #99318, #70918, #55112, #35769 ) ) ;
#2122 = AXIS2_PLACEMENT_3D ( 'NONE', #49903, #9959, #102214 ) ;
#2123 = ORIENTED_EDGE ( 'NONE', *, *, #1805, .F. ) ;
#2124 = DIRECTION ( 'NONE',  ( 0.000000000000000000, 0.000000000000000000, -1.000000000000000000 ) ) ;
#2125 = VERTEX_POINT ( 'NONE', #45157 ) ;
#2126 = DIRECTION ( 'NONE',  ( -0.000000000000000000, 1.000000000000000000, -0.000000000000000000 ) ) ;
#2127 = EDGE_CURVE ( 'NONE', #6598, #3681, #116024, .T. ) ;
#2128 = FACE_OUTER_BOUND ( 'NONE', #86643, .T. ) ;
#2131 = ORIENTED_EDGE ( 'NONE', *, *, #4841, .T. ) ;
#2130 = ORIENTED_EDGE ( 'NONE', *, *, #61987, .T. ) ;
#2129 = EDGE_CURVE ( 'NONE', #10801, #33059, #70061, .T. ) ;
#2132 = EDGE_LOOP ( 'NONE', ( #51989, #93357, #36210, #32245 ) ) ;
#2133 = ADVANCED_FACE ( 'NONE', ( #75240 ), #59622, .T. ) ;
#2134 = CARTESIAN_POINT ( 'NONE',  ( -9.400000000000007461, 12.50000000000000000, 4.611443907251934426 ) ) ;
#2135 = AXIS2_PLACEMENT_3D ( 'NONE', #18953, #80492, #79199 ) ;
#2136 = EDGE_CURVE ( 'NONE', #77027, #10762, #44491, .T. ) ;
#2137 = ADVANCED_FACE ( 'NONE', ( #73958 ), #57546, .T. ) ;
#2138 = CARTESIAN_POINT ( 'NONE',  ( -0.4000000000000401013, 2.500000000000000000, -3.537306695894649966 ) ) ;
#2139 = CARTESIAN_POINT ( 'NONE',  ( -3.750000000000031086, 12.50000000000000000, -5.802370205355749988 ) ) ;
#2140 = CARTESIAN_POINT ( 'NONE',  ( -10.00000000000000711, 2.500000000000000000, -3.737306695894645259 ) ) ;
#2141 = CIRCLE ( 'NONE', #29349, 0.1000000000000002554 ) ;
#2142 = CARTESIAN_POINT ( 'NONE',  ( -7.050000000000016698, 2.500000000000000000, -2.265063509461101798 ) ) ;
#2143 = CARTESIAN_POINT ( 'NONE',  ( 3.749999999999942268, 2.500000000000000000, -5.902370205355750521 ) ) ;
#2144 = EDGE_LOOP ( 'NONE', ( #12589, #99223 ) ) ;
#2145 = EDGE_CURVE ( 'NONE', #112302, #40817, #26153, .T. ) ;
#2146 = DIRECTION ( 'NONE',  ( 0.000000000000000000, -0.9999939076577903929, 0.003490651415223739937 ) ) ;
#2147 = VERTEX_POINT ( 'NONE', #4536 ) ;
#2148 = VERTEX_POINT ( 'NONE', #84417 ) ;
#2149 = ORIENTED_EDGE ( 'NONE', *, *, #71143, .T. ) ;
#2150 = DIRECTION ( 'NONE',  ( 0.000000000000000000, 0.000000000000000000, -1.000000000000000000 ) ) ;
#2151 = ORIENTED_EDGE ( 'NONE', *, *, #94338, .T. ) ;
#2152 = ORIENTED_EDGE ( 'NONE', *, *, #11842, .F. ) ;
#2153 = ORIENTED_EDGE ( 'NONE', *, *, #30560, .F. ) ;
#2154 = LINE ( 'NONE', #100369, #90385 ) ;
#2155 = CARTESIAN_POINT ( 'NONE',  ( -11.84999999999999787, 2.500000000000000000, -2.511473670974873951 ) ) ;
#2156 = DIRECTION ( 'NONE',  ( 0.000000000000000000, 0.000000000000000000, -1.000000000000000000 ) ) ;
#2157 = FACE_OUTER_BOUND ( 'NONE', #5443, .T. ) ;
#2158 = LINE ( 'NONE', #61090, #65860 ) ;
#2159 = CIRCLE ( 'NONE', #96232, 0.06509327318403745899 ) ;
#2160 = DIRECTION ( 'NONE',  ( 1.000000000000000000, 0.000000000000000000, 0.000000000000000000 ) ) ;
#2161 = CONICAL_SURFACE ( 'NONE', #4204, 0.1000000000000002554, 0.003490658503988666988 ) ;
#2162 = DIRECTION ( 'NONE',  ( 0.000000000000000000, 0.000000000000000000, -1.000000000000000000 ) ) ;
#2163 = ORIENTED_EDGE ( 'NONE', *, *, #93567, .T. ) ;
#2164 = CARTESIAN_POINT ( 'NONE',  ( 9.149999999999918643, 12.50000000000000000, -6.495190528383302464 ) ) ;
#2166 = CIRCLE ( 'NONE', #35633, 0.1000000000000002554 ) ;
#2165 = AXIS2_PLACEMENT_3D ( 'NONE', #45371, #33609, #25070 ) ;
#2167 = ORIENTED_EDGE ( 'NONE', *, *, #97078, .T. ) ;
#2168 = CARTESIAN_POINT ( 'NONE',  ( 1.649999999999951950, 2.500000000000000000, -5.702370205355749455 ) ) ;
#2169 = ORIENTED_EDGE ( 'NONE', *, *, #19435, .F. ) ;
#2170 = DIRECTION ( 'NONE',  ( -0.000000000000000000, 1.000000000000000000, -0.000000000000000000 ) ) ;
#2171 = VERTEX_POINT ( 'NONE', #83148 ) ;
#2172 = CARTESIAN_POINT ( 'NONE',  ( 184.3177083336747160, 4.367472073101515306, 7.564683531250000925 ) ) ;
#2173 = EDGE_CURVE ( 'NONE', #76, #94866, #40844, .T. ) ;
#2174 = CARTESIAN_POINT ( 'NONE',  ( 10.44999999999991047, 12.50000000000000000, -6.430097255199264339 ) ) ;
#2175 = ADVANCED_FACE ( 'NONE', ( #73301 ), #111918, .T. ) ;
#2176 = EDGE_LOOP ( 'NONE', ( #95967, #28992 ) ) ;
#2177 = EDGE_LOOP ( 'NONE', ( #104373, #50226 ) ) ;
#2178 = CARTESIAN_POINT ( 'NONE',  ( -7.900000000000014566, 2.500000000000000000, -4.922947341949753586 ) ) ;
#2179 = FACE_OUTER_BOUND ( 'NONE', #77936, .T. ) ;
#2180 = CARTESIAN_POINT ( 'NONE',  ( -5.200000000000020606, 12.50000000000000000, 3.983716857408420964 ) ) ;
#2181 = DIRECTION ( 'NONE',  ( 0.000000000000000000, 0.000000000000000000, 1.000000000000000000 ) ) ;
#2182 = EDGE_CURVE ( 'NONE', #9827, #97225, #122304, .T. ) ;
#2183 = DIRECTION ( 'NONE',  ( 0.000000000000000000, 1.000000000000000000, 0.000000000000000000 ) ) ;
#2184 = EDGE_LOOP ( 'NONE', ( #6771, #10215 ) ) ;
#2185 = CARTESIAN_POINT ( 'NONE',  ( -14.59999999999998366, 12.50000000000000000, 0.6928203230275518099 ) ) ;
#2186 = ORIENTED_EDGE ( 'NONE', *, *, #13563, .F. ) ;
#2187 = DIRECTION ( 'NONE',  ( 0.000000000000000000, 1.000000000000000000, 0.000000000000000000 ) ) ;
#2188 = CARTESIAN_POINT ( 'NONE',  ( 14.79999999999989235, 2.500000000000000000, 0.3464101615137735735 ) ) ;
#2189 = VECTOR ( 'NONE', #5687, 1000.000000000000000 ) ;
#2190 = FACE_OUTER_BOUND ( 'NONE', #87131, .T. ) ;
#2191 = FACE_OUTER_BOUND ( 'NONE', #19020, .T. ) ;
#2192 = DIRECTION ( 'NONE',  ( 0.000000000000000000, 1.000000000000000000, 0.000000000000000000 ) ) ;
#2193 = DIRECTION ( 'NONE',  ( -0.000000000000000000, -1.000000000000000000, -0.000000000000000000 ) ) ;
#2194 = DIRECTION ( 'NONE',  ( 0.000000000000000000, 1.000000000000000000, 0.000000000000000000 ) ) ;
#2195 = VERTEX_POINT ( 'NONE', #66702 ) ;
#2196 = CIRCLE ( 'NONE', #90019, 0.06509327318403745899 ) ;
#2197 = DIRECTION ( 'NONE',  ( -0.000000000000000000, -1.000000000000000000, -0.000000000000000000 ) ) ;
#2198 = DIRECTION ( 'NONE',  ( 0.000000000000000000, 1.000000000000000000, 0.000000000000000000 ) ) ;
#2199 = DIRECTION ( 'NONE',  ( 0.000000000000000000, -0.000000000000000000, 1.000000000000000000 ) ) ;
#2200 = ORIENTED_EDGE ( 'NONE', *, *, #44168, .T. ) ;
#2201 = EDGE_LOOP ( 'NONE', ( #109300, #34604 ) ) ;
#2202 = DIRECTION ( 'NONE',  ( 0.000000000000000000, 1.000000000000000000, 0.000000000000000000 ) ) ;
#2203 = EDGE_CURVE ( 'NONE', #91908, #127901, #38787, .T. ) ;
#2204 = VECTOR ( 'NONE', #106545, 1000.000000000000000 ) ;
#2205 = ORIENTED_EDGE ( 'NONE', *, *, #63753, .T. ) ;
#2206 = B_SPLINE_SURFACE_WITH_KNOTS ( 'NONE', 3, 1, ( 
 ( #98243, #108068 ),
 ( #128385, #119182 ),
 ( #44, #90347 ),
 ( #59652, #10501 ),
 ( #70725, #79900 ),
 ( #70088, #58979 ),
 ( #110016, #110646 ),
 ( #58348, #98889 ),
 ( #20342, #30826 ),
 ( #60291, #20978 ) ),
 .UNSPECIFIED., .F., .F., .F.,
 ( 4, 2, 2, 2, 4 ),
 ( 2, 2 ),
 ( 0.000000000000000000, 0.2500000000000000555, 0.5000000000000001110, 0.7500000000000000000, 1.000000000000000000 ),
 ( 0.000000000000000000, 1.000000000000000000 ),
 .UNSPECIFIED. ) ;
#2207 = VERTEX_POINT ( 'NONE', #28734 ) ;
#2208 = FACE_OUTER_BOUND ( 'NONE', #5583, .T. ) ;
#2209 = ORIENTED_EDGE ( 'NONE', *, *, #56633, .T. ) ;
#2210 = CARTESIAN_POINT ( 'NONE',  ( 18.98912670146303938, -2.543039972612231026, -4.488908218021264496 ) ) ;
#2211 = DIRECTION ( 'NONE',  ( 0.000000000000000000, 1.000000000000000000, 0.000000000000000000 ) ) ;
#2212 = CARTESIAN_POINT ( 'NONE',  ( 20.37025966759629725, 0.6621301594407191793, 4.188616773932410275 ) ) ;
#2213 = CONICAL_SURFACE ( 'NONE', #14809, 0.1000000000000002554, 0.003490658503988666988 ) ;
#2214 = ORIENTED_EDGE ( 'NONE', *, *, #2357, .T. ) ;
#2215 = DIRECTION ( 'NONE',  ( 0.000000000000000000, 1.000000000000000000, 0.000000000000000000 ) ) ;
#2216 = DIRECTION ( 'NONE',  ( 0.000000000000000000, 0.000000000000000000, -1.000000000000000000 ) ) ;
#2217 = CIRCLE ( 'NONE', #56591, 0.06509327318403745899 ) ;
#2218 = ADVANCED_FACE ( 'NONE', ( #67322 ), #55487, .T. ) ;
#2219 = EDGE_CURVE ( 'NONE', #58977, #67840, #113971, .T. ) ;
#2220 = VERTEX_POINT ( 'NONE', #58830 ) ;
#2221 = EDGE_LOOP ( 'NONE', ( #51847, #87279, #93317, #109129 ) ) ;
#2222 = ORIENTED_EDGE ( 'NONE', *, *, #29947, .T. ) ;
#2223 = DIRECTION ( 'NONE',  ( -0.000000000000000000, -1.000000000000000000, -0.000000000000000000 ) ) ;
#2224 = DIRECTION ( 'NONE',  ( 0.000000000000000000, 1.000000000000000000, 0.000000000000000000 ) ) ;
#2225 = CARTESIAN_POINT ( 'NONE',  ( 5.649999999999934630, 12.50000000000000000, -1.818653347947325916 ) ) ;
#2226 = EDGE_CURVE ( 'NONE', #87462, #63696, #69273, .T. ) ;
#2227 = FACE_BOUND ( 'NONE', #42197, .T. ) ;
#2228 = EDGE_LOOP ( 'NONE', ( #117663, #107045, #105670, #22259 ) ) ;
#2229 = DIRECTION ( 'NONE',  ( -0.000000000000000000, 1.000000000000000000, -0.000000000000000000 ) ) ;
#2230 = CARTESIAN_POINT ( 'NONE',  ( 6.249999999999928946, 12.50000000000000000, 2.792790559304612064 ) ) ;
#2231 = ORIENTED_EDGE ( 'NONE', *, *, #19266, .T. ) ;
#2232 = DIRECTION ( 'NONE',  ( -4.274815082592931898E-19, -0.9999939076577903929, -0.003490651415223739937 ) ) ;
#2233 = DIRECTION ( 'NONE',  ( 0.000000000000000000, 0.000000000000000000, -1.000000000000000000 ) ) ;
#2235 = DIRECTION ( 'NONE',  ( 0.000000000000000000, 1.000000000000000000, 0.000000000000000000 ) ) ;
#2234 = VECTOR ( 'NONE', #76226, 1000.000000000000000 ) ;
#2236 = CARTESIAN_POINT ( 'NONE',  ( 3.749999999999942268, 2.500000000000000000, -5.802370205355749988 ) ) ;
#2237 = CARTESIAN_POINT ( 'NONE',  ( 6.049999999999932321, 2.500000000000000000, 1.718653347947321386 ) ) ;
#2238 = CIRCLE ( 'NONE', #185, 0.1000000000000002554 ) ;
#2239 = AXIS2_PLACEMENT_3D ( 'NONE', #129365, #18081, #57375 ) ;
#2240 = DIRECTION ( 'NONE',  ( -0.000000000000000000, -1.000000000000000000, -0.000000000000000000 ) ) ;
#2241 = DIRECTION ( 'NONE',  ( 0.000000000000000000, 0.000000000000000000, -1.000000000000000000 ) ) ;
#2242 = AXIS2_PLACEMENT_3D ( 'NONE', #15885, #95748, #76106 ) ;
#2243 = EDGE_LOOP ( 'NONE', ( #9958, #124399, #108955, #90283 ) ) ;
#2244 = EDGE_LOOP ( 'NONE', ( #111426, #90679, #74627, #129328 ) ) ;
#2245 = EDGE_LOOP ( 'NONE', ( #34887, #68094, #50064, #123822 ) ) ;
#2246 = ORIENTED_EDGE ( 'NONE', *, *, #28925, .T. ) ;
#2247 = DIRECTION ( 'NONE',  ( -4.274815082592931898E-19, -0.9999939076577903929, -0.003490651415223739937 ) ) ;
#2248 = CARTESIAN_POINT ( 'NONE',  ( -10.40000000000000213, 2.500000000000000000, -5.122947341949750211 ) ) ;
#2249 = AXIS2_PLACEMENT_3D ( 'NONE', #82818, #122094, #32446 ) ;
#2250 = LINE ( 'NONE', #112229, #61372 ) ;
#2251 = VERTEX_POINT ( 'NONE', #36630 ) ;
#2252 = FACE_BOUND ( 'NONE', #106027, .T. ) ;
#2253 = CARTESIAN_POINT ( 'NONE',  ( -13.74999999999995381, 12.50000000000000000, -2.165063509461099489 ) ) ;
#2254 = CARTESIAN_POINT ( 'NONE',  ( -13.34999999999999076, 12.50000000000000000, -2.165063509461099489 ) ) ;
#2256 = EDGE_CURVE ( 'NONE', #70431, #9486, #15752, .T. ) ;
#2255 = CARTESIAN_POINT ( 'NONE',  ( 4.349999999999941025, 12.50000000000000000, -1.818653347947326138 ) ) ;
#2257 = CARTESIAN_POINT ( 'NONE',  ( 0.5999999999999555689, 2.500000000000000000, 4.676537180435972552 ) ) ;
#2258 = FACE_OUTER_BOUND ( 'NONE', #54075, .T. ) ;
#2259 = DIRECTION ( 'NONE',  ( 0.000000000000000000, 1.000000000000000000, 0.000000000000000000 ) ) ;
#2260 = FACE_OUTER_BOUND ( 'NONE', #8307, .T. ) ;
#2261 = DIRECTION ( 'NONE',  ( -0.000000000000000000, -1.000000000000000000, -0.000000000000000000 ) ) ;
#2262 = EDGE_CURVE ( 'NONE', #111941, #240, #82590, .T. ) ;
#2263 = DIRECTION ( 'NONE',  ( 0.000000000000000000, 1.000000000000000000, 0.000000000000000000 ) ) ;
#2264 = EDGE_CURVE ( 'NONE', #38409, #7115, #76326, .T. ) ;
#2265 = ORIENTED_EDGE ( 'NONE', *, *, #128795, .F. ) ;
#2266 = EDGE_LOOP ( 'NONE', ( #92439, #23875, #12611, #22147 ) ) ;
#2267 = VERTEX_POINT ( 'NONE', #109201 ) ;
#2268 = ORIENTED_EDGE ( 'NONE', *, *, #26548, .F. ) ;
#2269 = VERTEX_POINT ( 'NONE', #58202 ) ;
#2270 = EDGE_CURVE ( 'NONE', #56716, #12489, #56869, .T. ) ;
#2271 = EDGE_LOOP ( 'NONE', ( #24593, #18778, #12277, #12430 ) ) ;
#2273 = ADVANCED_FACE ( 'NONE', ( #56239 ), #99413, .T. ) ;
#2272 = DIRECTION ( 'NONE',  ( 0.000000000000000000, -0.9999939076577903929, 0.003490651415223739937 ) ) ;
#2275 = ORIENTED_EDGE ( 'NONE', *, *, #124504, .T. ) ;
#2274 = EDGE_CURVE ( 'NONE', #123488, #121393, #30466, .T. ) ;
#2276 = VERTEX_POINT ( 'NONE', #96804 ) ;
#2277 = CIRCLE ( 'NONE', #92168, 0.06509327318403745899 ) ;
#2278 = CONICAL_SURFACE ( 'NONE', #48261, 0.1000000000000000056, 0.003490658503988666988 ) ;
#2280 = ADVANCED_FACE ( 'NONE', ( #117083 ), #86865, .T. ) ;
#2279 = DIRECTION ( 'NONE',  ( -0.000000000000000000, -1.000000000000000000, -0.000000000000000000 ) ) ;
#2281 = CARTESIAN_POINT ( 'NONE',  ( 14.18215599412843098, -2.499999999999999556, 6.639800459772741803 ) ) ;
#2282 = DIRECTION ( 'NONE',  ( 0.000000000000000000, -0.9999939076577903929, 0.003490651415223739937 ) ) ;
#2283 = LINE ( 'NONE', #50130, #27987 ) ;
#2284 = ORIENTED_EDGE ( 'NONE', *, *, #97865, .T. ) ;
#2285 = CARTESIAN_POINT ( 'NONE',  ( -9.150000000000005684, 12.50000000000000000, 5.802370205355744659 ) ) ;
#2286 = EDGE_CURVE ( 'NONE', #127872, #14057, #47173, .T. ) ;
#2287 = CIRCLE ( 'NONE', #110947, 0.06509327318403745899 ) ;
#2288 = ORIENTED_EDGE ( 'NONE', *, *, #86039, .F. ) ;
#2289 = VERTEX_POINT ( 'NONE', #38570 ) ;
#2290 = CARTESIAN_POINT ( 'NONE',  ( -17.50000000000000000, 2.500000000000000000, -9.999999999999998224 ) ) ;
#2291 = DIRECTION ( 'NONE',  ( 0.000000000000000000, -0.9999939076577903929, 0.003490651415223739937 ) ) ;
#2292 = ORIENTED_EDGE ( 'NONE', *, *, #98914, .T. ) ;
#2293 = ORIENTED_EDGE ( 'NONE', *, *, #65057, .T. ) ;
#2294 = CIRCLE ( 'NONE', #92185, 0.06509327318403745899 ) ;
#2295 = DIRECTION ( 'NONE',  ( 0.000000000000000000, -0.000000000000000000, 1.000000000000000000 ) ) ;
#2296 = AXIS2_PLACEMENT_3D ( 'NONE', #31865, #42327, #122183 ) ;
#2297 = FACE_OUTER_BOUND ( 'NONE', #63665, .T. ) ;
#2298 = LINE ( 'NONE', #44833, #68775 ) ;
#2299 = DIRECTION ( 'NONE',  ( -0.000000000000000000, 1.000000000000000000, -0.000000000000000000 ) ) ;
#2300 = CARTESIAN_POINT ( 'NONE',  ( 12.29999999999990479, 12.50000000000000000, 4.676537180435972552 ) ) ;
#2301 = CONICAL_SURFACE ( 'NONE', #88061, 0.09999999999999982514, 0.003490658503988666988 ) ;
#2302 = ORIENTED_EDGE ( 'NONE', *, *, #121294, .F. ) ;
#2303 = CARTESIAN_POINT ( 'NONE',  ( 7.180215335565367063, -2.500000000000000000, 8.697219394475791177 ) ) ;
#2304 = ORIENTED_EDGE ( 'NONE', *, *, #62845, .F. ) ;
#2305 = CARTESIAN_POINT ( 'NONE',  ( 187.5000000000000000, -1.500000000000000000, 6.000000000000000000 ) ) ;
#2306 = CARTESIAN_POINT ( 'NONE',  ( 10.39999999999990976, 2.500000000000000000, 4.330127018922196314 ) ) ;
#2307 = VECTOR ( 'NONE', #80832, 1000.000000000000000 ) ;
#2308 = CARTESIAN_POINT ( 'NONE',  ( 6.849999999999929479, 2.500000000000000000, 6.941600689897073018 ) ) ;
#2309 = CARTESIAN_POINT ( 'NONE',  ( 4.399999999999937295, 12.50000000000000000, 4.611443907251934426 ) ) ;
#2310 = FACE_OUTER_BOUND ( 'NONE', #115573, .T. ) ;
#2311 = ORIENTED_EDGE ( 'NONE', *, *, #57397, .T. ) ;
#2312 = DIRECTION ( 'NONE',  ( 0.000000000000000000, 0.000000000000000000, 1.000000000000000000 ) ) ;
#2313 = EDGE_CURVE ( 'NONE', #28179, #11893, #24183, .T. ) ;
#2314 = FACE_OUTER_BOUND ( 'NONE', #7225, .T. ) ;
#2315 = EDGE_LOOP ( 'NONE', ( #116559, #35390, #114477, #73866 ) ) ;
#2316 = ORIENTED_EDGE ( 'NONE', *, *, #92232, .F. ) ;
#2317 = EDGE_LOOP ( 'NONE', ( #127543, #42310 ) ) ;
#2318 = DIRECTION ( 'NONE',  ( 0.000000000000000000, 0.000000000000000000, 1.000000000000000000 ) ) ;
#2319 = FACE_OUTER_BOUND ( 'NONE', #56475, .T. ) ;
#2320 = PRESENTATION_STYLE_ASSIGNMENT (( #29873 ) ) ;
#2321 = DIRECTION ( 'NONE',  ( 0.000000000000000000, 0.000000000000000000, 1.000000000000000000 ) ) ;
#2322 = CARTESIAN_POINT ( 'NONE',  ( 8.549999999999920774, 2.500000000000000000, -2.411473670974877859 ) ) ;
#2323 = EDGE_CURVE ( 'NONE', #8397, #120782, #53438, .T. ) ;
#2324 = FACE_OUTER_BOUND ( 'NONE', #38482, .T. ) ;
#2325 = CARTESIAN_POINT ( 'NONE',  ( 7.499999999999927169, 12.50000000000000000, -5.022947341949754119 ) ) ;
#2326 = DIRECTION ( 'NONE',  ( 0.000000000000000000, 0.000000000000000000, 1.000000000000000000 ) ) ;
#2327 = AXIS2_PLACEMENT_3D ( 'NONE', #125629, #85073, #126943 ) ;
#2328 = CIRCLE ( 'NONE', #65015, 0.1000000000000002554 ) ;
#2329 = AXIS2_PLACEMENT_3D ( 'NONE', #114833, #65740, #6166 ) ;
#2330 = CONICAL_SURFACE ( 'NONE', #31611, 0.09999999999999982514, 0.003490658503988666988 ) ;
#2331 = CIRCLE ( 'NONE', #62997, 4.000000000000000000 ) ;
#2332 = ORIENTED_EDGE ( 'NONE', *, *, #69303, .F. ) ;
#2333 = CARTESIAN_POINT ( 'NONE',  ( -13.09999999999999254, 12.50000000000000000, -0.3464101615137741286 ) ) ;
#2334 = CONICAL_SURFACE ( 'NONE', #77658, 0.09999999999999982514, 0.003490658503988666988 ) ;
#2335 = CARTESIAN_POINT ( 'NONE',  ( 4.149999999999941735, 2.500000000000000000, -2.857883832488653741 ) ) ;
#2336 = DIRECTION ( 'NONE',  ( 0.000000000000000000, 0.000000000000000000, 1.000000000000000000 ) ) ;
#2337 = CARTESIAN_POINT ( 'NONE',  ( 12.29999999999990656, 12.50000000000000000, -4.741630453620015118 ) ) ;
#2338 = ORIENTED_EDGE ( 'NONE', *, *, #57239, .F. ) ;
#2339 = FACE_OUTER_BOUND ( 'NONE', #19616, .T. ) ;
#2340 = FACE_OUTER_BOUND ( 'NONE', #3049, .T. ) ;
#2342 = ORIENTED_EDGE ( 'NONE', *, *, #12243, .F. ) ;
#2341 = DIRECTION ( 'NONE',  ( 0.000000000000000000, 0.000000000000000000, 1.000000000000000000 ) ) ;
#2343 = ORIENTED_EDGE ( 'NONE', *, *, #8656, .F. ) ;
#2344 = CARTESIAN_POINT ( 'NONE',  ( 3.549999999999944755, 2.500000000000000000, -6.941600689897077459 ) ) ;
#2345 = EDGE_CURVE ( 'NONE', #25156, #460, #122391, .T. ) ;
#2346 = VERTEX_POINT ( 'NONE', #29383 ) ;
#2347 = ORIENTED_EDGE ( 'NONE', *, *, #100683, .T. ) ;
#2348 = FACE_OUTER_BOUND ( 'NONE', #121730, .T. ) ;
#2349 = CARTESIAN_POINT ( 'NONE',  ( 19.21290572970694299, 2.587129408759306859, -2.394140119531837918 ) ) ;
#2350 = DIRECTION ( 'NONE',  ( -0.000000000000000000, 1.000000000000000000, -0.000000000000000000 ) ) ;
#2351 = DIRECTION ( 'NONE',  ( 0.000000000000000000, 0.000000000000000000, 1.000000000000000000 ) ) ;
#2352 = EDGE_CURVE ( 'NONE', #84054, #128741, #77807, .T. ) ;
#2353 = ORIENTED_EDGE ( 'NONE', *, *, #36045, .F. ) ;
#2354 = AXIS2_PLACEMENT_3D ( 'NONE', #77507, #126623, #67679 ) ;
#2355 = DIRECTION ( 'NONE',  ( 0.000000000000000000, 1.000000000000000000, 0.000000000000000000 ) ) ;
#2356 = VERTEX_POINT ( 'NONE', #20194 ) ;
#2357 = EDGE_CURVE ( 'NONE', #75351, #128756, #82692, .T. ) ;
#2358 = CARTESIAN_POINT ( 'NONE',  ( 6.449999999999928235, 2.500000000000000000, 2.511473670974873507 ) ) ;
#2359 = DIRECTION ( 'NONE',  ( 0.000000000000000000, -0.9999939076577903929, 0.003490651415223739937 ) ) ;
#2360 = EDGE_CURVE ( 'NONE', #83282, #12520, #91509, .T. ) ;
#2361 = AXIS2_PLACEMENT_3D ( 'NONE', #77236, #65473, #15055 ) ;
#2362 = ORIENTED_EDGE ( 'NONE', *, *, #22963, .F. ) ;
#2363 = AXIS2_PLACEMENT_3D ( 'NONE', #68660, #8435, #38583 ) ;
#2364 = ORIENTED_EDGE ( 'NONE', *, *, #79466, .F. ) ;
#2365 = EDGE_CURVE ( 'NONE', #47194, #52167, #93148, .T. ) ;
#2366 = ORIENTED_EDGE ( 'NONE', *, *, #39428, .F. ) ;
#2367 = EDGE_LOOP ( 'NONE', ( #119048, #26114 ) ) ;
#2368 = DIRECTION ( 'NONE',  ( 0.000000000000000000, 1.000000000000000000, 0.000000000000000000 ) ) ;
#2369 = CARTESIAN_POINT ( 'NONE',  ( 16.31212829107016660, 2.500000000000259348, 6.358241997069723261 ) ) ;
#2370 =( BOUNDED_CURVE ( )  B_SPLINE_CURVE ( 2, ( #36862, #103671, #76781, #74847, #23816, #114754, #54535 ),
 .UNSPECIFIED., .F., .F. ) 
 B_SPLINE_CURVE_WITH_KNOTS ( ( 3, 2, 2, 3 ),
 ( 0.2142857142857144681, 0.2380952380952383041, 0.2619047619047621955, 0.2857142857142859760 ),
 .UNSPECIFIED. ) 
 CURVE ( )  GEOMETRIC_REPRESENTATION_ITEM ( )  RATIONAL_B_SPLINE_CURVE ( ( 0.9999999999999988898, 0.8660254037844397068, 1.000000000000000000, 0.8660254037844387076, 1.000000000000000000, 0.8660254037844371533, 1.000000000000001554 ) ) 
 REPRESENTATION_ITEM ( '' )  );
#2371 = DIRECTION ( 'NONE',  ( 0.000000000000000000, 1.000000000000000000, 0.000000000000000000 ) ) ;
#2372 = ADVANCED_FACE ( 'NONE', ( #1830 ), #63890, .T. ) ;
#2373 = FACE_BOUND ( 'NONE', #69819, .T. ) ;
#2374 = EDGE_LOOP ( 'NONE', ( #15043, #18988 ) ) ;
#2375 = CARTESIAN_POINT ( 'NONE',  ( 183.9895833340161175, -4.445597072760115509, -7.700000000000001954 ) ) ;
#2376 = DIRECTION ( 'NONE',  ( 0.000000000000000000, 0.000000000000000000, 1.000000000000000000 ) ) ;
#2377 = LINE ( 'NONE', #35108, #73188 ) ;
#2378 = AXIS2_PLACEMENT_3D ( 'NONE', #85601, #25379, #46319 ) ;
#2379 = AXIS2_PLACEMENT_3D ( 'NONE', #45152, #34030, #95534 ) ;
#2380 = AXIS2_PLACEMENT_3D ( 'NONE', #128646, #97221, #29145 ) ;
#2381 = VECTOR ( 'NONE', #81570, 1000.000000000000000 ) ;
#2382 = DIRECTION ( 'NONE',  ( 0.000000000000000000, 0.000000000000000000, 1.000000000000000000 ) ) ;
#2383 = CARTESIAN_POINT ( 'NONE',  ( 15.83209681635531041, -1.500000000000000888, 5.404881881984402447 ) ) ;
#2384 = UNCERTAINTY_MEASURE_WITH_UNIT (LENGTH_MEASURE( 1.000000000000000082E-05 ), #1978, 'distance_accuracy_value', 'NONE');
#2385 = DIRECTION ( 'NONE',  ( 0.000000000000000000, 0.000000000000000000, 1.000000000000000000 ) ) ;
#2386 = CIRCLE ( 'NONE', #340, 0.1000000000000000472 ) ;
#2387 = DIRECTION ( 'NONE',  ( 0.000000000000000000, 0.000000000000000000, -1.000000000000000000 ) ) ;
#2388 = VERTEX_POINT ( 'NONE', #21480 ) ;
#2389 = CIRCLE ( 'NONE', #63058, 5.200000000000000178 ) ;
#2390 = VECTOR ( 'NONE', #37748, 1000.000000000000000 ) ;
#2391 = EDGE_LOOP ( 'NONE', ( #116054, #1797 ) ) ;
#2392 = EDGE_LOOP ( 'NONE', ( #23017, #78011 ) ) ;
#2393 = ADVANCED_BREP_SHAPE_REPRESENTATION ( '', ( #58784, #108296 ), #47765 ) ;
#2394 = ORIENTED_EDGE ( 'NONE', *, *, #103651, .T. ) ;
#2395 = VERTEX_POINT ( 'NONE', #41791 ) ;
#2396 = CARTESIAN_POINT ( 'NONE',  ( -4.600000000000024514, 12.50000000000000000, 3.637306695894644726 ) ) ;
#2397 = CARTESIAN_POINT ( 'NONE',  ( 4.599999999999940137, 2.500000000000000000, -4.230127018922201998 ) ) ;
#2398 = EDGE_LOOP ( 'NONE', ( #19752, #25268 ) ) ;
#2399 = FACE_BOUND ( 'NONE', #103410, .T. ) ;
#2400 = PLANE ( 'NONE',  #95896 ) ;
#2401 = EDGE_CURVE ( 'NONE', #77067, #110742, #80629, .T. ) ;
#2402 = ORIENTED_EDGE ( 'NONE', *, *, #56485, .F. ) ;
#2403 = CARTESIAN_POINT ( 'NONE',  ( 6.449999999999930012, 12.50000000000000000, 1.818653347947321475 ) ) ;
#2404 = CARTESIAN_POINT ( 'NONE',  ( 9.149999999999916866, 2.500000000000000000, -1.472243186433550122 ) ) ;
#2405 = DIRECTION ( 'NONE',  ( -0.000000000000000000, 1.000000000000000000, -0.000000000000000000 ) ) ;
#2406 = ORIENTED_EDGE ( 'NONE', *, *, #28810, .F. ) ;
#2407 = CARTESIAN_POINT ( 'NONE',  ( 4.149999999999939959, 2.500000000000000000, -2.165063509461101710 ) ) ;
#2408 = ADVANCED_FACE ( 'NONE', ( #39858 ), #76418, .T. ) ;
#2409 = VERTEX_POINT ( 'NONE', #101339 ) ;
#2410 = ORIENTED_EDGE ( 'NONE', *, *, #89206, .F. ) ;
#2411 = VECTOR ( 'NONE', #32048, 1000.000000000000000 ) ;
#2412 = ORIENTED_EDGE ( 'NONE', *, *, #86879, .T. ) ;
#2413 = VECTOR ( 'NONE', #84929, 1000.000000000000000 ) ;
#2414 = EDGE_CURVE ( 'NONE', #87409, #54592, #89576, .T. ) ;
#2415 = FACE_OUTER_BOUND ( 'NONE', #71981, .T. ) ;
#2416 = DIRECTION ( 'NONE',  ( 0.000000000000000000, -0.000000000000000000, 1.000000000000000000 ) ) ;
#2417 = DIRECTION ( 'NONE',  ( 0.000000000000000000, 0.000000000000000000, 1.000000000000000000 ) ) ;
#2419 = ORIENTED_EDGE ( 'NONE', *, *, #15548, .F. ) ;
#2418 = EDGE_CURVE ( 'NONE', #112557, #122705, #30679, .T. ) ;
#2420 = DIRECTION ( 'NONE',  ( 0.000000000000000000, 1.000000000000000000, 0.000000000000000000 ) ) ;
#2421 = EDGE_CURVE ( 'NONE', #22876, #34089, #74353, .T. ) ;
#2422 = FACE_OUTER_BOUND ( 'NONE', #55216, .T. ) ;
#2423 = AXIS2_PLACEMENT_3D ( 'NONE', #23473, #91570, #101401 ) ;
#2425 = AXIS2_PLACEMENT_3D ( 'NONE', #1646, #33076, #72979 ) ;
#2424 = CARTESIAN_POINT ( 'NONE',  ( 8.299999999999922551, 2.500000000000000000, -2.385244779468109755E-15 ) ) ;
#2427 = EDGE_CURVE ( 'NONE', #29791, #85654, #34668, .T. ) ;
#2426 = CARTESIAN_POINT ( 'NONE',  ( 10.64999999999990976, 12.50000000000000000, -6.148780366869526226 ) ) ;
#2428 = CARTESIAN_POINT ( 'NONE',  ( 185.9479166673494603, -6.668395609140176816, -3.850000000000003642 ) ) ;
#2429 = ORIENTED_EDGE ( 'NONE', *, *, #98433, .F. ) ;
#2430 = AXIS2_PLACEMENT_3D ( 'NONE', #82803, #121412, #101140 ) ;
#2431 = CARTESIAN_POINT ( 'NONE',  ( 2.049999999999950084, 12.50000000000000000, -6.430097255199264339 ) ) ;
#2432 = VERTEX_POINT ( 'NONE', #111806 ) ;
#2433 = CARTESIAN_POINT ( 'NONE',  ( 105.5000000000000142, 0.000000000000000000, 0.000000000000000000 ) ) ;
#2434 = EDGE_CURVE ( 'NONE', #59088, #19851, #31668, .T. ) ;
#2435 = CIRCLE ( 'NONE', #12894, 0.06509327318403745899 ) ;
#2436 = EDGE_CURVE ( 'NONE', #93873, #74504, #75570, .T. ) ;
#2437 = VERTEX_POINT ( 'NONE', #20840 ) ;
#2438 = PLANE ( 'NONE',  #18318 ) ;
#2439 = VERTEX_POINT ( 'NONE', #110502 ) ;
#2440 = CARTESIAN_POINT ( 'NONE',  ( 1.049999999999952083, 12.50000000000000000, 6.841600689897072485 ) ) ;
#2441 = DIRECTION ( 'NONE',  ( 0.000000000000000000, 0.000000000000000000, -1.000000000000000000 ) ) ;
#2442 = FACE_OUTER_BOUND ( 'NONE', #24617, .T. ) ;
#2443 = FACE_OUTER_BOUND ( 'NONE', #17284, .T. ) ;
#2444 = CARTESIAN_POINT ( 'NONE',  ( 184.4999999999999432, -6.631591114337888726, -3.783919631704756092 ) ) ;
#2445 = ORIENTED_EDGE ( 'NONE', *, *, #104997, .F. ) ;
#2446 = ORIENTED_EDGE ( 'NONE', *, *, #56336, .T. ) ;
#2447 = CARTESIAN_POINT ( 'NONE',  ( -1.850000000000033840, 2.500000000000000000, 2.511473670974873507 ) ) ;
#2448 = LINE ( 'NONE', #31941, #89179 ) ;
#2449 = DIRECTION ( 'NONE',  ( 0.000000000000000000, 0.000000000000000000, -1.000000000000000000 ) ) ;
#2451 = VERTEX_POINT ( 'NONE', #90198 ) ;
#2450 = EDGE_LOOP ( 'NONE', ( #102947, #109387, #77285, #36067 ) ) ;
#2452 = ORIENTED_EDGE ( 'NONE', *, *, #45661, .T. ) ;
#2453 = DIRECTION ( 'NONE',  ( 0.000000000000000000, -0.000000000000000000, 1.000000000000000000 ) ) ;
#2455 = VERTEX_POINT ( 'NONE', #2463 ) ;
#2454 = CIRCLE ( 'NONE', #69266, 0.1000000000000002554 ) ;
#2456 = FACE_OUTER_BOUND ( 'NONE', #93514, .T. ) ;
#2457 = DIRECTION ( 'NONE',  ( 0.000000000000000000, 1.000000000000000000, 0.000000000000000000 ) ) ;
#2458 = CIRCLE ( 'NONE', #90281, 0.09999999999999999167 ) ;
#2459 = DIRECTION ( 'NONE',  ( 0.000000000000000000, 0.000000000000000000, -1.000000000000000000 ) ) ;
#2460 = EDGE_LOOP ( 'NONE', ( #6522, #89055 ) ) ;
#2461 = CARTESIAN_POINT ( 'NONE',  ( 5.199999999999933564, 2.500000000000000000, 0.4464101615137735513 ) ) ;
#2462 = CARTESIAN_POINT ( 'NONE',  ( 6.249999999999932498, 2.500000000000000000, 5.902370205355745192 ) ) ;
#2463 = CARTESIAN_POINT ( 'NONE',  ( 7.699999999999925571, 2.500000000000000000, -4.576537180435978236 ) ) ;
#2464 = PLANE ( 'NONE',  #59350 ) ;
#2465 = FACE_OUTER_BOUND ( 'NONE', #114572, .T. ) ;
#2466 = ORIENTED_EDGE ( 'NONE', *, *, #47546, .T. ) ;
#2467 = CONICAL_SURFACE ( 'NONE', #77772, 0.1000000000000002554, 0.003490658503988666988 ) ;
#2468 = AXIS2_PLACEMENT_3D ( 'NONE', #105545, #6032, #68176 ) ;
#2469 = CARTESIAN_POINT ( 'NONE',  ( -7.500000000000011546, 2.500000000000000000, 3.537306695894645081 ) ) ;
#2470 = AXIS2_PLACEMENT_3D ( 'NONE', #85895, #113601, #86551 ) ;
#2471 = VECTOR ( 'NONE', #96940, 1000.000000000000000 ) ;
#2472 = CARTESIAN_POINT ( 'NONE',  ( 65.34954526970105348, -3.515384427006628787, 5.621991122703798638 ) ) ;
#2473 = EDGE_LOOP ( 'NONE', ( #36913, #54590, #21796, #46091 ) ) ;
#2474 = ORIENTED_EDGE ( 'NONE', *, *, #116064, .T. ) ;
#2475 = CARTESIAN_POINT ( 'NONE',  ( 186.3802083336747444, 4.367472073101515306, 7.564683531250000925 ) ) ;
#2476 = LINE ( 'NONE', #121613, #124283 ) ;
#2477 = CARTESIAN_POINT ( 'NONE',  ( -11.84999999999999609, 2.500000000000000000, 6.741600689897071952 ) ) ;
#2478 = CIRCLE ( 'NONE', #71431, 0.1000000000000002554 ) ;
#2479 = LINE ( 'NONE', #53543, #94922 ) ;
#2480 = FACE_OUTER_BOUND ( 'NONE', #114483, .T. ) ;
#2481 = VECTOR ( 'NONE', #88524, 1000.000000000000000 ) ;
#2482 = EDGE_CURVE ( 'NONE', #85597, #54227, #117303, .T. ) ;
#2483 = DIRECTION ( 'NONE',  ( 0.000000000000000000, 0.000000000000000000, 1.000000000000000000 ) ) ;
#2484 = VECTOR ( 'NONE', #17187, 1000.000000000000000 ) ;
#2485 = CARTESIAN_POINT ( 'NONE',  ( 12.94999999999989981, 2.500000000000000000, -2.065063509461102065 ) ) ;
#2486 = FACE_OUTER_BOUND ( 'NONE', #113369, .T. ) ;
#2487 = CONICAL_SURFACE ( 'NONE', #42519, 0.1000000000000002554, 0.003490658503988666988 ) ;
#2488 = AXIS2_PLACEMENT_3D ( 'NONE', #93850, #116540, #113480 ) ;
#2489 = CARTESIAN_POINT ( 'NONE',  ( -2.499999999999996447, 2.500000000000000000, 4.430127018922196847 ) ) ;
#2490 = ORIENTED_EDGE ( 'NONE', *, *, #78998, .T. ) ;
#2491 = EDGE_LOOP ( 'NONE', ( #88964, #44101 ) ) ;
#2492 = VERTEX_POINT ( 'NONE', #90863 ) ;
#2493 = EDGE_LOOP ( 'NONE', ( #84936, #36789 ) ) ;
#2494 = LINE ( 'NONE', #79786, #16919 ) ;
#2495 = CARTESIAN_POINT ( 'NONE',  ( -15.19999999999998330, 2.500000000000000000, 0.3464101615137758494 ) ) ;
#2496 = ORIENTED_EDGE ( 'NONE', *, *, #72490, .F. ) ;
#2497 = FACE_OUTER_BOUND ( 'NONE', #36409, .T. ) ;
#2498 = LINE ( 'NONE', #1869, #5132 ) ;
#2500 = VERTEX_POINT ( 'NONE', #49674 ) ;
#2499 = CARTESIAN_POINT ( 'NONE',  ( -0.6500000000000403233, 12.50000000000000000, 6.148780366869520009 ) ) ;
#2501 = LINE ( 'NONE', #72570, #7631 ) ;
#2502 = CARTESIAN_POINT ( 'NONE',  ( 9.199999999999915801, 2.500000000000000000, 4.330127018922196314 ) ) ;
#2503 = EDGE_LOOP ( 'NONE', ( #104639, #31206 ) ) ;
#2504 = ORIENTED_EDGE ( 'NONE', *, *, #51530, .F. ) ;
#2505 = VERTEX_POINT ( 'NONE', #72529 ) ;
#2506 = AXIS2_PLACEMENT_3D ( 'NONE', #113004, #44253, #4968 ) ;
#2507 = ORIENTED_EDGE ( 'NONE', *, *, #12285, .T. ) ;
#2508 = DIRECTION ( 'NONE',  ( -0.000000000000000000, 1.000000000000000000, -0.000000000000000000 ) ) ;
#2509 = CONICAL_SURFACE ( 'NONE', #46438, 0.09999999999999982514, 0.003490658503988666988 ) ;
#2510 = CONICAL_SURFACE ( 'NONE', #4645, 0.1000000000000000472, 0.003490658503988666988 ) ;
#2511 = CARTESIAN_POINT ( 'NONE',  ( 6.849999999999929479, 2.500000000000000000, 6.148780366869520009 ) ) ;
#2512 = CARTESIAN_POINT ( 'NONE',  ( 5.849999999999932143, 12.50000000000000000, 2.165063509461097713 ) ) ;
#2513 = CARTESIAN_POINT ( 'NONE',  ( -6.450000000000014388, 12.50000000000000000, 1.883746621131358934 ) ) ;
#2514 = EDGE_CURVE ( 'NONE', #38961, #26037, #31321, .T. ) ;
#2516 = ORIENTED_EDGE ( 'NONE', *, *, #90834, .F. ) ;
#2515 = CIRCLE ( 'NONE', #69426, 0.1000000000000002554 ) ;
#2517 = AXIS2_PLACEMENT_3D ( 'NONE', #83803, #33441, #44527 ) ;
#2518 = DIRECTION ( 'NONE',  ( -4.274815082592931898E-19, -0.9999939076577903929, -0.003490651415223739937 ) ) ;
#2520 = ORIENTED_EDGE ( 'NONE', *, *, #53103, .F. ) ;
#2519 = CIRCLE ( 'NONE', #44399, 0.09999999999999999167 ) ;
#2521 = DIRECTION ( 'NONE',  ( 0.000000000000000000, -0.9999939076577903929, 0.003490651415223739937 ) ) ;
#2522 = CARTESIAN_POINT ( 'NONE',  ( -6.650000000000019007, 2.500000000000000000, -1.572243186433550211 ) ) ;
#2523 = EDGE_CURVE ( 'NONE', #39233, #127679, #43323, .T. ) ;
#2524 = DIRECTION ( 'NONE',  ( 0.000000000000000000, 1.000000000000000000, 0.000000000000000000 ) ) ;
#2525 = DIRECTION ( 'NONE',  ( -0.000000000000000000, -1.000000000000000000, -0.000000000000000000 ) ) ;
#2526 = EDGE_CURVE ( 'NONE', #83361, #34821, #16953, .T. ) ;
#2527 = VECTOR ( 'NONE', #43741, 1000.000000000000000 ) ;
#2528 = ORIENTED_EDGE ( 'NONE', *, *, #46934, .T. ) ;
#2529 = EDGE_LOOP ( 'NONE', ( #120920, #38975, #4099, #127621 ) ) ;
#2530 = EDGE_CURVE ( 'NONE', #112123, #66032, #90130, .T. ) ;
#2532 = ORIENTED_EDGE ( 'NONE', *, *, #65929, .T. ) ;
#2531 = ADVANCED_FACE ( 'NONE', ( #124841 ), #62960, .T. ) ;
#2533 = CARTESIAN_POINT ( 'NONE',  ( -3.350000000000031619, 12.50000000000000000, -5.867463478539787225 ) ) ;
#2534 = DIRECTION ( 'NONE',  ( 0.000000000000000000, 1.000000000000000000, 0.000000000000000000 ) ) ;
#2535 = CARTESIAN_POINT ( 'NONE',  ( 3.349999999999945466, 2.500000000000000000, -2.957883832488653830 ) ) ;
#2536 = ADVANCED_FACE ( 'NONE', ( #74450 ), #60907, .T. ) ;
#2537 = FACE_BOUND ( 'NONE', #110485, .T. ) ;
#2538 = DIRECTION ( 'NONE',  ( 0.000000000000000000, 1.000000000000000000, 0.000000000000000000 ) ) ;
#2539 = CARTESIAN_POINT ( 'NONE',  ( 11.89999999999990443, 2.500000000000000000, -0.4464101615137782142 ) ) ;
#2540 = DIRECTION ( 'NONE',  ( -0.000000000000000000, -1.000000000000000000, -0.000000000000000000 ) ) ;
#2541 = CARTESIAN_POINT ( 'NONE',  ( -5.850000000000021849, 2.500000000000000000, -2.957883832488653830 ) ) ;
#2542 = DIRECTION ( 'NONE',  ( 0.000000000000000000, -0.000000000000000000, 1.000000000000000000 ) ) ;
#2543 = CARTESIAN_POINT ( 'NONE',  ( -0.6000000000000323963, 2.500000000000000000, -0.4464101615137759382 ) ) ;
#2544 = VERTEX_POINT ( 'NONE', #12924 ) ;
#2545 = DIRECTION ( 'NONE',  ( -0.000000000000000000, -1.000000000000000000, -0.000000000000000000 ) ) ;
#2546 = CARTESIAN_POINT ( 'NONE',  ( -4.350000000000027178, 2.500000000000000000, -6.841600689897077814 ) ) ;
#2547 = ORIENTED_EDGE ( 'NONE', *, *, #57080, .T. ) ;
#2548 = ORIENTED_EDGE ( 'NONE', *, *, #18075, .T. ) ;
#2549 = DIRECTION ( 'NONE',  ( 0.000000000000000000, 0.000000000000000000, -1.000000000000000000 ) ) ;
#2550 = DIRECTION ( 'NONE',  ( -0.000000000000000000, -1.000000000000000000, -0.000000000000000000 ) ) ;
#2551 = FACE_BOUND ( 'NONE', #118144, .T. ) ;
#2552 = LINE ( 'NONE', #82451, #28539 ) ;
#2553 = AXIS2_PLACEMENT_3D ( 'NONE', #111461, #83928, #125161 ) ;
#2554 = CIRCLE ( 'NONE', #42390, 0.06509327318403745899 ) ;
#2555 = CIRCLE ( 'NONE', #117464, 0.1000000000000002554 ) ;
#2556 = ORIENTED_EDGE ( 'NONE', *, *, #10699, .T. ) ;
#2557 = FACE_OUTER_BOUND ( 'NONE', #56731, .T. ) ;
#2558 = DIRECTION ( 'NONE',  ( 0.000000000000000000, 1.000000000000000000, 0.000000000000000000 ) ) ;
#2559 = ORIENTED_EDGE ( 'NONE', *, *, #47085, .T. ) ;
#2561 = DIRECTION ( 'NONE',  ( 0.000000000000000000, 1.000000000000000000, 0.000000000000000000 ) ) ;
#2560 = AXIS2_PLACEMENT_3D ( 'NONE', #69678, #19944, #6860 ) ;
#2562 = CARTESIAN_POINT ( 'NONE',  ( 11.84999999999990372, 12.50000000000000000, 1.818653347947321475 ) ) ;
#2563 = CIRCLE ( 'NONE', #50610, 0.1000000000000002554 ) ;
#2564 = AXIS2_PLACEMENT_3D ( 'NONE', #92964, #53670, #123676 ) ;
#2565 = AXIS2_PLACEMENT_3D ( 'NONE', #81835, #21647, #29534 ) ;
#2566 = AXIS2_PLACEMENT_3D ( 'NONE', #66194, #115268, #6596 ) ;
#2567 = EDGE_CURVE ( 'NONE', #26449, #109816, #10706, .T. ) ;
#2568 = VERTEX_POINT ( 'NONE', #53528 ) ;
#2569 = EDGE_CURVE ( 'NONE', #21611, #86863, #21196, .T. ) ;
#2570 = DIRECTION ( 'NONE',  ( 0.000000000000000000, 1.000000000000000000, 0.000000000000000000 ) ) ;
#2571 = DIRECTION ( 'NONE',  ( 0.000000000000000000, 1.000000000000000000, 0.000000000000000000 ) ) ;
#2572 = AXIS2_PLACEMENT_3D ( 'NONE', #24465, #114131, #64381 ) ;
#2573 = ADVANCED_FACE ( 'NONE', ( #14847 ), #106860, .T. ) ;
#2574 = ORIENTED_EDGE ( 'NONE', *, *, #9119, .T. ) ;
#2575 = CARTESIAN_POINT ( 'NONE',  ( -2.700000000000029932, 2.500000000000000000, -0.4464101615137782142 ) ) ;
#2576 = CIRCLE ( 'NONE', #19310, 0.1000000000000000472 ) ;
#2577 = DIRECTION ( 'NONE',  ( 0.000000000000000000, 0.000000000000000000, 1.000000000000000000 ) ) ;
#2578 = CARTESIAN_POINT ( 'NONE',  ( 2.699999999999945555, 2.500000000000000000, 4.083716857408420609 ) ) ;
#2579 = ADVANCED_FACE ( 'NONE', ( #83633 ), #112452, .T. ) ;
#2580 = VERTEX_POINT ( 'NONE', #104550 ) ;
#2581 = VERTEX_POINT ( 'NONE', #93443 ) ;
#2582 = EDGE_CURVE ( 'NONE', #37773, #72985, #94344, .T. ) ;
#2583 = PLANE ( 'NONE',  #65990 ) ;
#2585 = EDGE_LOOP ( 'NONE', ( #117318, #4173 ) ) ;
#2584 = EDGE_CURVE ( 'NONE', #55889, #77376, #123592, .T. ) ;
#2586 = DIRECTION ( 'NONE',  ( 0.000000000000000000, 1.000000000000000000, 0.000000000000000000 ) ) ;
#2587 = CARTESIAN_POINT ( 'NONE',  ( 9.399999999999915090, 12.50000000000000000, 3.918623584224383727 ) ) ;
#2588 = EDGE_CURVE ( 'NONE', #54197, #54180, #19117, .T. ) ;
#2589 = EDGE_CURVE ( 'NONE', #44930, #83361, #84907, .T. ) ;
#2590 = CARTESIAN_POINT ( 'NONE',  ( 7.499999999999960032, 2.500000000000000000, -0.1000000000000022815 ) ) ;
#2591 = ORIENTED_EDGE ( 'NONE', *, *, #117354, .T. ) ;
#2592 = DIRECTION ( 'NONE',  ( -0.000000000000000000, 1.000000000000000000, -0.000000000000000000 ) ) ;
#2593 = DIRECTION ( 'NONE',  ( -0.000000000000000000, 1.000000000000000000, -0.000000000000000000 ) ) ;
#2594 = CARTESIAN_POINT ( 'NONE',  ( 5.399999999999936406, 2.500000000000000000, -3.637306695894650055 ) ) ;
#2595 = FACE_OUTER_BOUND ( 'NONE', #126876, .T. ) ;
#2596 = DIRECTION ( 'NONE',  ( -0.000000000000000000, -1.000000000000000000, -0.000000000000000000 ) ) ;
#2597 = AXIS2_PLACEMENT_3D ( 'NONE', #8601, #106812, #36813 ) ;
#2599 = EDGE_CURVE ( 'NONE', #16102, #105827, #127805, .T. ) ;
#2598 = DIRECTION ( 'NONE',  ( 0.000000000000000000, 1.000000000000000000, 0.000000000000000000 ) ) ;
#2600 = ORIENTED_EDGE ( 'NONE', *, *, #82184, .T. ) ;
#2601 = VERTEX_POINT ( 'NONE', #82996 ) ;
#2602 = CARTESIAN_POINT ( 'NONE',  ( 6.249999999999932498, 2.500000000000000000, -2.957883832488653830 ) ) ;
#2603 = ORIENTED_EDGE ( 'NONE', *, *, #113504, .F. ) ;
#2604 = AXIS2_PLACEMENT_3D ( 'NONE', #11427, #99823, #110274 ) ;
#2605 = LINE ( 'NONE', #53021, #68153 ) ;
#2606 = AXIS2_PLACEMENT_3D ( 'NONE', #81180, #73931, #113864 ) ;
#2607 = VECTOR ( 'NONE', #26167, 1000.000000000000000 ) ;
#2609 = ORIENTED_EDGE ( 'NONE', *, *, #41208, .F. ) ;
#2608 = ORIENTED_EDGE ( 'NONE', *, *, #38797, .F. ) ;
#2610 = ORIENTED_EDGE ( 'NONE', *, *, #58219, .T. ) ;
#2611 = CARTESIAN_POINT ( 'NONE',  ( -9.600000000000008527, 2.500000000000000000, -5.122947341949750211 ) ) ;
#2612 = FACE_OUTER_BOUND ( 'NONE', #65621, .T. ) ;
#2613 = CIRCLE ( 'NONE', #92508, 0.06509327318403745899 ) ;
#2615 = DIRECTION ( 'NONE',  ( -0.000000000000000000, 1.000000000000000000, -0.000000000000000000 ) ) ;
#2614 = AXIS2_PLACEMENT_3D ( 'NONE', #80446, #120370, #128922 ) ;
#2616 = CONICAL_SURFACE ( 'NONE', #59073, 0.09999999999999982514, 0.003490658503988666988 ) ;
#2617 = CARTESIAN_POINT ( 'NONE',  ( 6.249999999999965361, 2.500000000000000000, 2.265063509461097357 ) ) ;
#2618 = FACE_OUTER_BOUND ( 'NONE', #124727, .T. ) ;
#2619 = CARTESIAN_POINT ( 'NONE',  ( 1.649999999999951505, 2.500000000000000000, 2.957883832488649389 ) ) ;
#2620 = DIRECTION ( 'NONE',  ( 0.000000000000000000, 0.000000000000000000, 1.000000000000000000 ) ) ;
#2621 = CARTESIAN_POINT ( 'NONE',  ( 7.499999999999925393, 2.500000000000000000, 5.022947341949748790 ) ) ;
#2622 = CARTESIAN_POINT ( 'NONE',  ( 6.449999999999930012, 2.500000000000000000, -1.718653347947326049 ) ) ;
#2623 = AXIS2_PLACEMENT_3D ( 'NONE', #10238, #77044, #116945 ) ;
#2624 = ORIENTED_EDGE ( 'NONE', *, *, #76613, .F. ) ;
#2625 = CARTESIAN_POINT ( 'NONE',  ( 3.949999999999941558, 2.500000000000000000, -6.048780366869526581 ) ) ;
#2626 = ORIENTED_EDGE ( 'NONE', *, *, #109397, .F. ) ;
#2627 = VERTEX_POINT ( 'NONE', #95378 ) ;
#2628 = DIRECTION ( 'NONE',  ( -0.000000000000000000, -1.000000000000000000, -0.000000000000000000 ) ) ;
#2629 = DIRECTION ( 'NONE',  ( 0.000000000000000000, 0.000000000000000000, 1.000000000000000000 ) ) ;
#2630 = DIRECTION ( 'NONE',  ( 0.000000000000000000, 0.000000000000000000, -1.000000000000000000 ) ) ;
#2631 = CIRCLE ( 'NONE', #105042, 0.06509327318403745899 ) ;
#2632 = CARTESIAN_POINT ( 'NONE',  ( 8.949999999999915801, 2.500000000000000000, 6.841600689897072485 ) ) ;
#2633 = EDGE_CURVE ( 'NONE', #111448, #113894, #121532, .T. ) ;
#2634 = DIRECTION ( 'NONE',  ( 0.000000000000000000, 0.000000000000000000, 1.000000000000000000 ) ) ;
#2635 = CARTESIAN_POINT ( 'NONE',  ( 186.0312500006828031, 9.429780353434619030E-16, -7.700000000000000178 ) ) ;
#2636 = FACE_OUTER_BOUND ( 'NONE', #91479, .T. ) ;
#2637 = ORIENTED_EDGE ( 'NONE', *, *, #71743, .F. ) ;
#2638 = AXIS2_PLACEMENT_3D ( 'NONE', #126653, #95261, #38275 ) ;
#2639 = CIRCLE ( 'NONE', #107205, 0.06509327318403745899 ) ;
#2640 = ORIENTED_EDGE ( 'NONE', *, *, #36405, .F. ) ;
#2641 = CONICAL_SURFACE ( 'NONE', #61154, 0.1000000000000002554, 0.003490658503988666988 ) ;
#2642 = ORIENTED_EDGE ( 'NONE', *, *, #1850, .T. ) ;
#2643 = ORIENTED_EDGE ( 'NONE', *, *, #126696, .T. ) ;
#2644 = EDGE_CURVE ( 'NONE', #113, #119313, #85550, .T. ) ;
#2645 = ORIENTED_EDGE ( 'NONE', *, *, #84372, .T. ) ;
#2646 = CIRCLE ( 'NONE', #600, 0.1000000000000002554 ) ;
#2647 = CARTESIAN_POINT ( 'NONE',  ( -8.300000000000009592, 2.500000000000000000, 4.330127018922196314 ) ) ;
#2648 = LINE ( 'NONE', #103456, #31041 ) ;
#2649 = VECTOR ( 'NONE', #42428, 1000.000000000000000 ) ;
#2650 = AXIS2_PLACEMENT_3D ( 'NONE', #59785, #20485, #51249 ) ;
#2651 = LINE ( 'NONE', #32798, #100813 ) ;
#2652 = DIRECTION ( 'NONE',  ( 0.000000000000000000, 1.000000000000000000, 0.000000000000000000 ) ) ;
#2653 = DIRECTION ( 'NONE',  ( 0.000000000000000000, -0.9999939076577903929, 0.003490651415223739937 ) ) ;
#2654 = VERTEX_POINT ( 'NONE', #35811 ) ;
#2655 = DIRECTION ( 'NONE',  ( 0.000000000000000000, 0.000000000000000000, -1.000000000000000000 ) ) ;
#2656 = DIRECTION ( 'NONE',  ( 0.000000000000000000, 0.000000000000000000, 1.000000000000000000 ) ) ;
#2657 = DIRECTION ( 'NONE',  ( 0.000000000000000000, 0.000000000000000000, 1.000000000000000000 ) ) ;
#2658 = CIRCLE ( 'NONE', #10970, 0.1000000000000002554 ) ;
#2659 = CONICAL_SURFACE ( 'NONE', #17225, 0.1000000000000002554, 0.003490658503988666988 ) ;
#2660 = DIRECTION ( 'NONE',  ( 0.000000000000000000, 1.000000000000000000, 0.000000000000000000 ) ) ;
#2661 = ORIENTED_EDGE ( 'NONE', *, *, #5829, .F. ) ;
#2662 = VECTOR ( 'NONE', #122271, 1000.000000000000000 ) ;
#2663 = CONICAL_SURFACE ( 'NONE', #27806, 0.09999999999999982514, 0.003490658503988666988 ) ;
#2664 = CONICAL_SURFACE ( 'NONE', #56944, 0.1000000000000002554, 0.003490658503988666988 ) ;
#2665 = ORIENTED_EDGE ( 'NONE', *, *, #76878, .T. ) ;
#2666 = ORIENTED_EDGE ( 'NONE', *, *, #6673, .T. ) ;
#2667 = DIRECTION ( 'NONE',  ( 0.000000000000000000, 0.000000000000000000, 1.000000000000000000 ) ) ;
#2668 = CIRCLE ( 'NONE', #15186, 0.06509327318403745899 ) ;
#2669 = VERTEX_POINT ( 'NONE', #52879 ) ;
#2670 = DIRECTION ( 'NONE',  ( -0.000000000000000000, 1.000000000000000000, -0.000000000000000000 ) ) ;
#2671 = DIRECTION ( 'NONE',  ( 0.000000000000000000, 1.000000000000000000, 0.000000000000000000 ) ) ;
#2672 = ADVANCED_FACE ( 'NONE', ( #24064 ), #103910, .T. ) ;
#2673 = AXIS2_PLACEMENT_3D ( 'NONE', #118990, #108523, #9683 ) ;
#2674 = EDGE_LOOP ( 'NONE', ( #118146, #2120, #127648, #44713 ) ) ;
#2675 = CARTESIAN_POINT ( 'NONE',  ( 4.149999999999938183, 2.500000000000000000, 7.188010851410848723 ) ) ;
#2676 = CARTESIAN_POINT ( 'NONE',  ( -0.8000000000000315747, 2.500000000000000000, 0.000000000000000000 ) ) ;
#2677 = CARTESIAN_POINT ( 'NONE',  ( 184.5000000000000000, -6.267304879582558996, 4.236192450104883100 ) ) ;
#2678 = FACE_OUTER_BOUND ( 'NONE', #23150, .T. ) ;
#2679 = EDGE_CURVE ( 'NONE', #40817, #112302, #37925, .T. ) ;
#2680 = DIRECTION ( 'NONE',  ( -0.000000000000000000, -1.000000000000000000, -0.000000000000000000 ) ) ;
#2681 = ORIENTED_EDGE ( 'NONE', *, *, #7492, .F. ) ;
#2682 = EDGE_CURVE ( 'NONE', #50283, #18676, #54636, .T. ) ;
#2683 = ADVANCED_FACE ( 'NONE', ( #67842 ), #47574, .T. ) ;
#2684 = AXIS2_PLACEMENT_3D ( 'NONE', #25158, #123368, #77971 ) ;
#2685 = EDGE_LOOP ( 'NONE', ( #117186, #55891, #76035, #100290 ) ) ;
#2686 = VECTOR ( 'NONE', #45189, 1000.000000000000000 ) ;
#2687 = EDGE_CURVE ( 'NONE', #81254, #110135, #46938, .T. ) ;
#2689 = ADVANCED_FACE ( 'NONE', ( #97946 ), #67167, .T. ) ;
#2688 = CARTESIAN_POINT ( 'NONE',  ( 108.0000000000000142, 8.700999999999998735, -5.000000000000004441 ) ) ;
#2690 = EDGE_CURVE ( 'NONE', #11740, #104068, #71359, .T. ) ;
#2691 = CARTESIAN_POINT ( 'NONE',  ( 7.949999999999925571, 2.500000000000000000, -6.495190528383302464 ) ) ;
#2692 = CARTESIAN_POINT ( 'NONE',  ( -7.500000000000013323, 12.50000000000000000, 5.022947341949748790 ) ) ;
#2693 = CARTESIAN_POINT ( 'NONE',  ( -8.950000000000009948, 12.50000000000000000, -1.818653347947326138 ) ) ;
#2694 = ORIENTED_EDGE ( 'NONE', *, *, #15092, .T. ) ;
#2695 = AXIS2_PLACEMENT_3D ( 'NONE', #88821, #128777, #39108 ) ;
#2696 = VECTOR ( 'NONE', #41880, 1000.000000000000000 ) ;
#2697 = CONICAL_SURFACE ( 'NONE', #126034, 0.09999999999999982514, 0.003490658503988666988 ) ;
#2698 = CIRCLE ( 'NONE', #63365, 0.1000000000000002554 ) ;
#2699 = EDGE_LOOP ( 'NONE', ( #114872, #20001 ) ) ;
#2700 = DIRECTION ( 'NONE',  ( 0.000000000000000000, 0.000000000000000000, 1.000000000000000000 ) ) ;
#2701 = DIRECTION ( 'NONE',  ( 0.000000000000000000, 0.000000000000000000, 1.000000000000000000 ) ) ;
#2702 = EDGE_CURVE ( 'NONE', #34419, #6486, #88066, .T. ) ;
#2703 = DIRECTION ( 'NONE',  ( 0.000000000000000000, 0.000000000000000000, 1.000000000000000000 ) ) ;
#2704 = CARTESIAN_POINT ( 'NONE',  ( 4.999999999999973355, 2.500000000000000000, -4.330127018922201643 ) ) ;
#2705 = ORIENTED_EDGE ( 'NONE', *, *, #116804, .T. ) ;
#2706 = EDGE_CURVE ( 'NONE', #72427, #46092, #81828, .T. ) ;
#2709 = EDGE_CURVE ( 'NONE', #34681, #94526, #127417, .T. ) ;
#2708 = CARTESIAN_POINT ( 'NONE',  ( -3.350000000000028955, 2.500000000000000000, 5.802370205355744659 ) ) ;
#2707 = CIRCLE ( 'NONE', #19432, 0.5000000000000000000 ) ;
#2710 = AXIS2_PLACEMENT_3D ( 'NONE', #39092, #68517, #18775 ) ;
#2711 = CIRCLE ( 'NONE', #46527, 7.700000000000000178 ) ;
#2712 = CARTESIAN_POINT ( 'NONE',  ( -1.050000000000038236, 2.500000000000000000, -1.918653347947326004 ) ) ;
#2713 = AXIS2_PLACEMENT_3D ( 'NONE', #122251, #3116, #91484 ) ;
#2714 = ORIENTED_EDGE ( 'NONE', *, *, #127995, .F. ) ;
#2715 = AXIS2_PLACEMENT_3D ( 'NONE', #49441, #89349, #99819 ) ;
#2716 = CARTESIAN_POINT ( 'NONE',  ( 8.749999999999957367, 12.50000000000000000, 2.099970236277060032 ) ) ;
#2717 = ORIENTED_EDGE ( 'NONE', *, *, #67235, .T. ) ;
#2718 = AXIS2_PLACEMENT_3D ( 'NONE', #41013, #80915, #120835 ) ;
#2719 = DIRECTION ( 'NONE',  ( 0.000000000000000000, 0.000000000000000000, 1.000000000000000000 ) ) ;
#2720 = EDGE_LOOP ( 'NONE', ( #9302, #35012 ) ) ;
#2721 = LINE ( 'NONE', #62939, #86192 ) ;
#2722 = FACE_OUTER_BOUND ( 'NONE', #5768, .T. ) ;
#2723 = ORIENTED_EDGE ( 'NONE', *, *, #70197, .T. ) ;
#2724 = EDGE_LOOP ( 'NONE', ( #70477, #76376, #25055, #26694 ) ) ;
#2725 = LINE ( 'NONE', #101587, #58190 ) ;
#2726 = CARTESIAN_POINT ( 'NONE',  ( -3.100000000000028511, 2.500000000000000000, -4.776537180435977525 ) ) ;
#2727 = AXIS2_PLACEMENT_3D ( 'NONE', #25087, #14602, #92533 ) ;
#2728 = CARTESIAN_POINT ( 'NONE',  ( 187.2968750003414300, 8.734944146203032389, 5.348610694689227483E-16 ) ) ;
#2729 = CARTESIAN_POINT ( 'NONE',  ( 185.2760416670080588, 6.551208109652274736, 3.782341765625001351 ) ) ;
#2730 = CARTESIAN_POINT ( 'NONE',  ( -10.85000000000000142, 2.500000000000000000, -6.495190528383298911 ) ) ;
#2731 = DIRECTION ( 'NONE',  ( 0.000000000000000000, 0.000000000000000000, 1.000000000000000000 ) ) ;
#2732 = DIRECTION ( 'NONE',  ( 0.000000000000000000, -0.000000000000000000, 1.000000000000000000 ) ) ;
#2733 = CARTESIAN_POINT ( 'NONE',  ( -2.900000000000029221, 12.50000000000000000, -0.6928203230275541413 ) ) ;
#2734 = CARTESIAN_POINT ( 'NONE',  ( -3.950000000000029932, 2.500000000000000000, -6.048780366869526581 ) ) ;
#2735 = AXIS2_PLACEMENT_3D ( 'NONE', #53251, #12017, #94440 ) ;
#2736 = ADVANCED_FACE ( 'NONE', ( #106483 ), #42133, .T. ) ;
#2737 = CONICAL_SURFACE ( 'NONE', #29951, 0.1000000000000002554, 0.003490658503988666988 ) ;
#2738 = CIRCLE ( 'NONE', #75908, 0.09999999999999982514 ) ;
#2739 = ORIENTED_EDGE ( 'NONE', *, *, #111630, .F. ) ;
#2740 = ADVANCED_FACE ( 'NONE', ( #27922 ), #86835, .T. ) ;
#2741 = EDGE_LOOP ( 'NONE', ( #15690, #56889, #85690, #21277 ) ) ;
#2742 = DIRECTION ( 'NONE',  ( 0.000000000000000000, -0.9999939076577903929, 0.003490651415223739937 ) ) ;
#2743 = ORIENTED_EDGE ( 'NONE', *, *, #22817, .F. ) ;
#2744 = LINE ( 'NONE', #112070, #122776 ) ;
#2745 = CARTESIAN_POINT ( 'NONE',  ( -11.84999999999999609, 2.500000000000000000, 6.048780366869521252 ) ) ;
#2746 = CARTESIAN_POINT ( 'NONE',  ( -6.050000000000022027, 12.50000000000000000, -1.818653347947326138 ) ) ;
#2748 = EDGE_LOOP ( 'NONE', ( #74714, #97201 ) ) ;
#2747 = ORIENTED_EDGE ( 'NONE', *, *, #127482, .F. ) ;
#2749 = FACE_BOUND ( 'NONE', #15038, .T. ) ;
#2750 = ORIENTED_EDGE ( 'NONE', *, *, #14810, .F. ) ;
#2751 = ADVANCED_FACE ( 'NONE', ( #118234 ), #88100, .T. ) ;
#2752 = AXIS2_PLACEMENT_3D ( 'NONE', #113963, #23646, #83844 ) ;
#2753 = DIRECTION ( 'NONE',  ( -0.000000000000000000, 1.000000000000000000, -0.000000000000000000 ) ) ;
#2754 = CARTESIAN_POINT ( 'NONE',  ( 17.79089025268843827, -2.511997385349134415, 2.795007471442847002 ) ) ;
#2755 = VECTOR ( 'NONE', #54178, 1000.000000000000000 ) ;
#2756 = EDGE_CURVE ( 'NONE', #60318, #53692, #16783, .T. ) ;
#2758 = DIRECTION ( 'NONE',  ( 0.000000000000000000, 1.000000000000000000, 0.000000000000000000 ) ) ;
#2757 = CIRCLE ( 'NONE', #90483, 0.06509327318403745899 ) ;
#2759 = DIRECTION ( 'NONE',  ( -0.000000000000000000, 1.000000000000000000, -0.000000000000000000 ) ) ;
#2760 = CONICAL_SURFACE ( 'NONE', #11062, 0.1000000000000002554, 0.003490658503988666988 ) ;
#2761 = CARTESIAN_POINT ( 'NONE',  ( -11.84999999999999787, 2.500000000000000000, -6.841600689897074261 ) ) ;
#2762 = EDGE_CURVE ( 'NONE', #109689, #101886, #108407, .T. ) ;
#2763 = DIRECTION ( 'NONE',  ( 0.000000000000000000, 1.000000000000000000, 0.000000000000000000 ) ) ;
#2764 = CARTESIAN_POINT ( 'NONE',  ( 2.899999999999946620, 2.500000000000000000, -0.6928203230275542523 ) ) ;
#2765 = DIRECTION ( 'NONE',  ( 0.000000000000000000, 1.000000000000000000, 0.000000000000000000 ) ) ;
#2766 = DIRECTION ( 'NONE',  ( 0.000000000000000000, 1.000000000000000000, 0.000000000000000000 ) ) ;
#2767 = DIRECTION ( 'NONE',  ( 0.000000000000000000, 0.000000000000000000, -1.000000000000000000 ) ) ;
#2768 = AXIS2_PLACEMENT_3D ( 'NONE', #116367, #45078, #5754 ) ;
#2770 = EDGE_CURVE ( 'NONE', #78466, #109968, #58678, .T. ) ;
#2769 = LINE ( 'NONE', #838, #101550 ) ;
#2771 = EDGE_LOOP ( 'NONE', ( #86641, #125935 ) ) ;
#2772 = ORIENTED_EDGE ( 'NONE', *, *, #76296, .T. ) ;
#2773 = ORIENTED_EDGE ( 'NONE', *, *, #42941, .F. ) ;
#2774 = DIRECTION ( 'NONE',  ( 0.000000000000000000, 0.000000000000000000, -1.000000000000000000 ) ) ;
#2776 = ORIENTED_EDGE ( 'NONE', *, *, #84116, .T. ) ;
#2775 = AXIS2_PLACEMENT_3D ( 'NONE', #21221, #71612, #12045 ) ;
#2777 = AXIS2_PLACEMENT_3D ( 'NONE', #7477, #30371, #38251 ) ;
#2778 = AXIS2_PLACEMENT_3D ( 'NONE', #73139, #30652, #20818 ) ;
#2779 = CARTESIAN_POINT ( 'NONE',  ( 11.64999999999990443, 2.500000000000000000, -5.702370205355749455 ) ) ;
#2781 = EDGE_LOOP ( 'NONE', ( #104980, #33286, #114242, #8049 ) ) ;
#2780 = ORIENTED_EDGE ( 'NONE', *, *, #6961, .T. ) ;
#2782 = VERTEX_POINT ( 'NONE', #128734 ) ;
#2783 = VECTOR ( 'NONE', #25937, 1000.000000000000000 ) ;
#2784 = CARTESIAN_POINT ( 'NONE',  ( 3.949999999999942446, 2.500000000000000000, -6.941600689897078347 ) ) ;
#2785 = FACE_OUTER_BOUND ( 'NONE', #35121, .T. ) ;
#2786 = AXIS2_PLACEMENT_3D ( 'NONE', #75674, #122866, #103222 ) ;
#2787 = DIRECTION ( 'NONE',  ( -0.000000000000000000, 1.000000000000000000, -0.000000000000000000 ) ) ;
#2788 = CARTESIAN_POINT ( 'NONE',  ( -7.100000000000017408, 12.50000000000000000, 0.6277270498435120194 ) ) ;
#2789 = CARTESIAN_POINT ( 'NONE',  ( 3.549999999999944755, 12.50000000000000000, -6.776507416713039689 ) ) ;
#2790 = DIRECTION ( 'NONE',  ( -0.000000000000000000, 1.000000000000000000, -0.000000000000000000 ) ) ;
#2791 = ADVANCED_FACE ( 'NONE', ( #75722 ), #116286, .T. ) ;
#2792 = ORIENTED_EDGE ( 'NONE', *, *, #117683, .F. ) ;
#2793 = DIRECTION ( 'NONE',  ( 0.000000000000000000, 0.000000000000000000, 1.000000000000000000 ) ) ;
#2794 = VERTEX_POINT ( 'NONE', #57387 ) ;
#2795 = ORIENTED_EDGE ( 'NONE', *, *, #95965, .F. ) ;
#2796 = ORIENTED_EDGE ( 'NONE', *, *, #29487, .F. ) ;
#2797 = EDGE_CURVE ( 'NONE', #44668, #51310, #23245, .T. ) ;
#2798 = DIRECTION ( 'NONE',  ( -1.000000000000000000, -0.000000000000000000, -0.000000000000000000 ) ) ;
#2799 = AXIS2_PLACEMENT_3D ( 'NONE', #118385, #8423, #18252 ) ;
#2800 = CIRCLE ( 'NONE', #13247, 0.06509327318403745899 ) ;
#2801 = VERTEX_POINT ( 'NONE', #118883 ) ;
#2802 = ORIENTED_EDGE ( 'NONE', *, *, #13755, .F. ) ;
#2803 = EDGE_LOOP ( 'NONE', ( #104737, #104794, #73009, #19513 ) ) ;
#2805 = CARTESIAN_POINT ( 'NONE',  ( 11.04999999999990656, 2.500000000000000000, 2.511473670974873507 ) ) ;
#2804 = AXIS2_PLACEMENT_3D ( 'NONE', #112969, #15396, #3663 ) ;
#2806 = CARTESIAN_POINT ( 'NONE',  ( -4.350000000000023626, 2.500000000000000000, 6.741600689897071952 ) ) ;
#2807 = EDGE_CURVE ( 'NONE', #124598, #74378, #113134, .T. ) ;
#2809 = DIRECTION ( 'NONE',  ( -0.000000000000000000, -1.000000000000000000, -0.000000000000000000 ) ) ;
#2808 = VECTOR ( 'NONE', #86278, 1000.000000000000000 ) ;
#2810 = LINE ( 'NONE', #21823, #28219 ) ;
#2811 = CIRCLE ( 'NONE', #75956, 0.06509327318403745899 ) ;
#2812 = CIRCLE ( 'NONE', #40488, 0.09999999999999982514 ) ;
#2813 = DIRECTION ( 'NONE',  ( -0.000000000000000000, -1.000000000000000000, -0.000000000000000000 ) ) ;
#2814 = DIRECTION ( 'NONE',  ( 0.000000000000000000, 0.000000000000000000, -1.000000000000000000 ) ) ;
#2816 = ORIENTED_EDGE ( 'NONE', *, *, #26281, .F. ) ;
#2815 = CIRCLE ( 'NONE', #78030, 0.06509327318403745899 ) ;
#2817 = DIRECTION ( 'NONE',  ( -0.000000000000000000, 1.000000000000000000, -0.000000000000000000 ) ) ;
#2818 = CIRCLE ( 'NONE', #57097, 0.06509327318403745899 ) ;
#2819 = EDGE_LOOP ( 'NONE', ( #1407, #66731, #34191, #113258 ) ) ;
#2820 = CARTESIAN_POINT ( 'NONE',  ( -7.500000000000001776, -1.500000000000000000, 1.734723475976807094E-15 ) ) ;
#2821 = AXIS2_PLACEMENT_3D ( 'NONE', #94067, #35792, #84886 ) ;
#2822 = VERTEX_POINT ( 'NONE', #52084 ) ;
#2823 = AXIS2_PLACEMENT_3D ( 'NONE', #115984, #76708, #87799 ) ;
#2824 = DIRECTION ( 'NONE',  ( 0.000000000000000000, 0.000000000000000000, 1.000000000000000000 ) ) ;
#2825 = ADVANCED_FACE ( 'NONE', ( #39060 ), #79782, .T. ) ;
#2826 = VERTEX_POINT ( 'NONE', #78973 ) ;
#2827 = CIRCLE ( 'NONE', #54753, 0.06509327318403745899 ) ;
#2828 = CARTESIAN_POINT ( 'NONE',  ( 184.4427083336747160, -6.551208109652278289, 3.782341765624995134 ) ) ;
#2829 = DIRECTION ( 'NONE',  ( -4.274815082592931898E-19, -0.9999939076577903929, -0.003490651415223739937 ) ) ;
#2830 = VERTEX_POINT ( 'NONE', #71712 ) ;
#2831 = ORIENTED_EDGE ( 'NONE', *, *, #96438, .T. ) ;
#2832 = CARTESIAN_POINT ( 'NONE',  ( 5.449999999999937117, 12.50000000000000000, -6.495190528383302464 ) ) ;
#2833 = CARTESIAN_POINT ( 'NONE',  ( -12.29999999999999716, 2.500000000000000000, -3.983716857408423628 ) ) ;
#2834 = APPLICATION_CONTEXT ( 'automotive_design' ) ;
#2835 = CARTESIAN_POINT ( 'NONE',  ( -10.60000000000000142, 2.500000000000000000, 4.676537180435972552 ) ) ;
#2836 = DIRECTION ( 'NONE',  ( 0.000000000000000000, 0.000000000000000000, -1.000000000000000000 ) ) ;
#2837 = AXIS2_PLACEMENT_3D ( 'NONE', #12525, #32840, #52452 ) ;
#2838 = DIRECTION ( 'NONE',  ( -0.000000000000000000, -1.000000000000000000, -0.000000000000000000 ) ) ;
#2839 = VERTEX_POINT ( 'NONE', #80255 ) ;
#2840 = DIRECTION ( 'NONE',  ( 0.000000000000000000, 0.000000000000000000, -1.000000000000000000 ) ) ;
#2841 = AXIS2_PLACEMENT_3D ( 'NONE', #52286, #101390, #42477 ) ;
#2842 = ORIENTED_EDGE ( 'NONE', *, *, #51787, .F. ) ;
#2843 = DIRECTION ( 'NONE',  ( 0.000000000000000000, 1.000000000000000000, 0.000000000000000000 ) ) ;
#2844 = CARTESIAN_POINT ( 'NONE',  ( 8.949999999999919353, 2.500000000000000000, 2.511473670974873507 ) ) ;
#2845 = CONICAL_SURFACE ( 'NONE', #65529, 0.1000000000000002554, 0.003490658503988666988 ) ;
#2846 = EDGE_CURVE ( 'NONE', #103729, #127557, #17039, .T. ) ;
#2847 = CARTESIAN_POINT ( 'NONE',  ( 185.6718750003414016, 9.264065473108010111E-16, -7.564683531250000925 ) ) ;
#2848 = CARTESIAN_POINT ( 'NONE',  ( 2.949999999999946887, 2.500000000000000000, -6.595190528383302109 ) ) ;
#2849 = CARTESIAN_POINT ( 'NONE',  ( 5.399999999999934630, 2.500000000000000000, -0.6928203230275542523 ) ) ;
#2850 = CARTESIAN_POINT ( 'NONE',  ( -9.150000000000005684, 2.500000000000000000, 6.395190528383296602 ) ) ;
#2851 = AXIS2_PLACEMENT_3D ( 'NONE', #28162, #100745, #9809 ) ;
#2853 = VECTOR ( 'NONE', #71076, 1000.000000000000000 ) ;
#2852 = FACE_OUTER_BOUND ( 'NONE', #47678, .T. ) ;
#2854 = VERTEX_POINT ( 'NONE', #111645 ) ;
#2856 = EDGE_CURVE ( 'NONE', #125867, #129536, #86020, .T. ) ;
#2855 = CIRCLE ( 'NONE', #107312, 0.09999999999999982514 ) ;
#2857 = CIRCLE ( 'NONE', #36334, 0.1000000000000002554 ) ;
#2858 = DIRECTION ( 'NONE',  ( 0.000000000000000000, 0.000000000000000000, 1.000000000000000000 ) ) ;
#2859 = LINE ( 'NONE', #31677, #69334 ) ;
#2860 = DIRECTION ( 'NONE',  ( 0.000000000000000000, 0.000000000000000000, 1.000000000000000000 ) ) ;
#2861 = ORIENTED_EDGE ( 'NONE', *, *, #8471, .F. ) ;
#2862 = EDGE_CURVE ( 'NONE', #32372, #94541, #109009, .T. ) ;
#2863 = EDGE_CURVE ( 'NONE', #59036, #43078, #11504, .T. ) ;
#2864 = EDGE_CURVE ( 'NONE', #64833, #125995, #67522, .T. ) ;
#2866 = ADVANCED_FACE ( 'NONE', ( #99894 ), #117406, .T. ) ;
#2865 = VECTOR ( 'NONE', #65208, 1000.000000000000000 ) ;
#2867 = CARTESIAN_POINT ( 'NONE',  ( -0.8000000000000381251, 2.500000000000000000, 4.330127018922196314 ) ) ;
#2868 = VERTEX_POINT ( 'NONE', #9576 ) ;
#2869 = CONICAL_SURFACE ( 'NONE', #13315, 0.1000000000000000472, 0.003490658503988666988 ) ;
#2871 = EDGE_LOOP ( 'NONE', ( #39620, #38671 ) ) ;
#2870 = VECTOR ( 'NONE', #31644, 1000.000000000000000 ) ;
#2872 = AXIS2_PLACEMENT_3D ( 'NONE', #48187, #76367, #78954 ) ;
#2873 = CARTESIAN_POINT ( 'NONE',  ( -5.650000000000019895, 12.50000000000000000, 1.753560074763284016 ) ) ;
#2874 = EDGE_CURVE ( 'NONE', #102170, #108113, #49514, .T. ) ;
#2875 = EDGE_CURVE ( 'NONE', #86508, #71451, #27527, .T. ) ;
#2877 = ORIENTED_EDGE ( 'NONE', *, *, #55480, .T. ) ;
#2876 = VECTOR ( 'NONE', #127363, 1000.000000000000000 ) ;
#2878 = CARTESIAN_POINT ( 'NONE',  ( 19.51231976789051004, -0.5900868802302308147, -4.348342248683373157 ) ) ;
#2879 = CARTESIAN_POINT ( 'NONE',  ( 129.5000000000000000, 0.6250000000000025535, -6.000000000000000888 ) ) ;
#2880 = ADVANCED_FACE ( 'NONE', ( #20050 ), #31797, .T. ) ;
#2881 = DIRECTION ( 'NONE',  ( 0.000000000000000000, 1.000000000000000000, 0.000000000000000000 ) ) ;
#2882 = AXIS2_PLACEMENT_3D ( 'NONE', #45406, #23829, #104315 ) ;
#2883 = EDGE_LOOP ( 'NONE', ( #50197, #22597, #38292, #93513 ) ) ;
#2884 = EDGE_CURVE ( 'NONE', #117215, #36888, #46324, .T. ) ;
#2886 = ADVANCED_FACE ( 'NONE', ( #61911 ), #12133, .T. ) ;
#2885 = CARTESIAN_POINT ( 'NONE',  ( 4.599999999999940137, 12.50000000000000000, -4.330127018922201643 ) ) ;
#2887 = DIRECTION ( 'NONE',  ( 0.000000000000000000, -0.000000000000000000, 1.000000000000000000 ) ) ;
#2888 = EDGE_CURVE ( 'NONE', #110892, #7910, #345, .T. ) ;
#2889 = EDGE_LOOP ( 'NONE', ( #97506, #30568, #102218, #60719 ) ) ;
#2890 = VERTEX_POINT ( 'NONE', #101823 ) ;
#2891 = ORIENTED_EDGE ( 'NONE', *, *, #36717, .F. ) ;
#2892 = DIRECTION ( 'NONE',  ( 0.000000000000000000, 1.000000000000000000, 0.000000000000000000 ) ) ;
#2893 = CARTESIAN_POINT ( 'NONE',  ( 0.1999999999999562961, 2.500000000000000000, 4.776537180435972196 ) ) ;
#2895 = DIRECTION ( 'NONE',  ( 0.000000000000000000, 0.000000000000000000, 1.000000000000000000 ) ) ;
#2894 = AXIS2_PLACEMENT_3D ( 'NONE', #39859, #537, #69942 ) ;
#2896 = AXIS2_PLACEMENT_3D ( 'NONE', #37229, #48989, #86953 ) ;
#2897 = FACE_BOUND ( 'NONE', #83659, .T. ) ;
#2898 = ORIENTED_EDGE ( 'NONE', *, *, #88134, .F. ) ;
#2899 = DIRECTION ( 'NONE',  ( -0.000000000000000000, 1.000000000000000000, -0.000000000000000000 ) ) ;
#2900 = DIRECTION ( 'NONE',  ( 0.000000000000000000, 1.000000000000000000, 0.000000000000000000 ) ) ;
#2901 = ORIENTED_EDGE ( 'NONE', *, *, #54875, .F. ) ;
#2902 = CARTESIAN_POINT ( 'NONE',  ( -13.74999999999995381, 2.500000000000000000, -2.165063509461099489 ) ) ;
#2904 = DIRECTION ( 'NONE',  ( 0.000000000000000000, 0.000000000000000000, -1.000000000000000000 ) ) ;
#2903 = CONICAL_SURFACE ( 'NONE', #96982, 0.09999999999999982514, 0.003490658503988666988 ) ;
#2905 = CIRCLE ( 'NONE', #101097, 0.09999999999999999167 ) ;
#2906 = CONICAL_SURFACE ( 'NONE', #21791, 0.09999999999999982514, 0.003490658503988666988 ) ;
#2907 = AXIS2_PLACEMENT_3D ( 'NONE', #125304, #95204, #44823 ) ;
#2909 = CONICAL_SURFACE ( 'NONE', #65594, 0.1000000000000002554, 0.003490658503988666988 ) ;
#2908 = FACE_OUTER_BOUND ( 'NONE', #54465, .T. ) ;
#2910 = DIRECTION ( 'NONE',  ( 0.000000000000000000, 1.000000000000000000, 0.000000000000000000 ) ) ;
#2911 = DIRECTION ( 'NONE',  ( 0.000000000000000000, 0.000000000000000000, -1.000000000000000000 ) ) ;
#2912 = CARTESIAN_POINT ( 'NONE',  ( -13.34999999999999076, 12.50000000000000000, 2.230156782645138946 ) ) ;
#2913 = DIRECTION ( 'NONE',  ( 0.000000000000000000, 1.000000000000000000, 0.000000000000000000 ) ) ;
#2914 = CIRCLE ( 'NONE', #61508, 0.09999999999999999167 ) ;
#2915 = CIRCLE ( 'NONE', #92808, 0.1000000000000002554 ) ;
#2916 = AXIS2_PLACEMENT_3D ( 'NONE', #53932, #34307, #93855 ) ;
#2917 = ORIENTED_EDGE ( 'NONE', *, *, #98468, .F. ) ;
#2918 = ORIENTED_EDGE ( 'NONE', *, *, #82838, .T. ) ;
#2919 = EDGE_LOOP ( 'NONE', ( #31296, #7476, #64231, #72085 ) ) ;
#2920 = ORIENTED_EDGE ( 'NONE', *, *, #18343, .F. ) ;
#2921 = DIRECTION ( 'NONE',  ( 0.000000000000000000, 1.000000000000000000, 0.000000000000000000 ) ) ;
#2922 = CARTESIAN_POINT ( 'NONE',  ( 127.5000000000000000, 0.000000000000000000, 0.000000000000000000 ) ) ;
#2923 = CIRCLE ( 'NONE', #107370, 0.06509327318403745899 ) ;
#2924 = DIRECTION ( 'NONE',  ( 0.000000000000000000, 0.000000000000000000, -1.000000000000000000 ) ) ;
#2925 = EDGE_LOOP ( 'NONE', ( #125324, #46202, #20469, #66864 ) ) ;
#2926 = FACE_BOUND ( 'NONE', #55172, .T. ) ;
#2927 = CARTESIAN_POINT ( 'NONE',  ( -3.350000000000031619, 2.500000000000000000, -7.188010851410854052 ) ) ;
#2928 = DIRECTION ( 'NONE',  ( -0.000000000000000000, -1.000000000000000000, -0.000000000000000000 ) ) ;
#2929 = EDGE_CURVE ( 'NONE', #124072, #104109, #67218, .T. ) ;
#2930 = DIRECTION ( 'NONE',  ( -0.000000000000000000, -1.000000000000000000, -0.000000000000000000 ) ) ;
#2931 = FACE_OUTER_BOUND ( 'NONE', #11110, .T. ) ;
#2932 = EDGE_CURVE ( 'NONE', #74283, #269, #33102, .T. ) ;
#2933 = LINE ( 'NONE', #23195, #109876 ) ;
#2934 = CARTESIAN_POINT ( 'NONE',  ( -14.14999999999998614, 12.50000000000000000, -2.165063509461099489 ) ) ;
#2935 = CARTESIAN_POINT ( 'NONE',  ( 1.649999999999949729, 2.500000000000000000, 5.702370205355745014 ) ) ;
#2936 = CARTESIAN_POINT ( 'NONE',  ( -4.400000000000028777, 2.500000000000000000, -4.576537180435978236 ) ) ;
#2937 = CARTESIAN_POINT ( 'NONE',  ( 8.949999999999919353, 2.500000000000000000, 2.511473670974873507 ) ) ;
#2938 = VECTOR ( 'NONE', #127645, 1000.000000000000000 ) ;
#2939 = EDGE_CURVE ( 'NONE', #4198, #42202, #113221, .T. ) ;
#2940 = ORIENTED_EDGE ( 'NONE', *, *, #2076, .F. ) ;
#2941 = ORIENTED_EDGE ( 'NONE', *, *, #3346, .F. ) ;
#2942 = ORIENTED_EDGE ( 'NONE', *, *, #79157, .T. ) ;
#2943 = ORIENTED_EDGE ( 'NONE', *, *, #58252, .T. ) ;
#2944 = EDGE_LOOP ( 'NONE', ( #46310, #51820, #113043, #48664 ) ) ;
#2945 = VERTEX_POINT ( 'NONE', #4241 ) ;
#2946 = CARTESIAN_POINT ( 'NONE',  ( -14.14999999999998614, 2.500000000000000000, -2.857883832488651521 ) ) ;
#2947 = ORIENTED_EDGE ( 'NONE', *, *, #29388, .F. ) ;
#2948 = VERTEX_POINT ( 'NONE', #14058 ) ;
#2949 = CONICAL_SURFACE ( 'NONE', #76098, 0.1000000000000000472, 0.003490658503988666988 ) ;
#2950 = DIRECTION ( 'NONE',  ( 0.000000000000000000, 1.000000000000000000, 0.000000000000000000 ) ) ;
#2951 = LINE ( 'NONE', #102438, #12345 ) ;
#2952 = CARTESIAN_POINT ( 'NONE',  ( -2.100000000000033396, 2.500000000000000000, 0.5928203230275495006 ) ) ;
#2953 = AXIS2_PLACEMENT_3D ( 'NONE', #13504, #80976, #122195 ) ;
#2954 = VERTEX_POINT ( 'NONE', #32469 ) ;
#2955 = CARTESIAN_POINT ( 'NONE',  ( 187.5000000000000000, 9.429780353434619030E-16, -7.700000000000000178 ) ) ;
#2956 = AXIS2_PLACEMENT_3D ( 'NONE', #50760, #111609, #72348 ) ;
#2957 = EDGE_LOOP ( 'NONE', ( #63891, #4320, #122732, #39382 ) ) ;
#2958 = AXIS2_PLACEMENT_3D ( 'NONE', #114890, #114256, #34430 ) ;
#2959 = VERTEX_POINT ( 'NONE', #52714 ) ;
#2960 = LINE ( 'NONE', #1015, #126233 ) ;
#2961 = DIRECTION ( 'NONE',  ( -0.000000000000000000, -1.000000000000000000, -0.000000000000000000 ) ) ;
#2962 = ORIENTED_EDGE ( 'NONE', *, *, #66844, .F. ) ;
#2963 = VERTEX_POINT ( 'NONE', #14701 ) ;
#2964 = PLANE ( 'NONE',  #84041 ) ;
#2966 = AXIS2_PLACEMENT_3D ( 'NONE', #23650, #100281, #86426 ) ;
#2965 = DIRECTION ( 'NONE',  ( 0.000000000000000000, 0.000000000000000000, 1.000000000000000000 ) ) ;
#2968 = CIRCLE ( 'NONE', #76120, 0.09999999999999982514 ) ;
#2967 = CARTESIAN_POINT ( 'NONE',  ( 6.699999999999928235, 2.500000000000000000, -2.276824562219559311E-15 ) ) ;
#2969 = VECTOR ( 'NONE', #49915, 1000.000000000000000 ) ;
#2970 = DIRECTION ( 'NONE',  ( 0.000000000000000000, -0.9999939076577903929, 0.003490651415223739937 ) ) ;
#2971 = DIRECTION ( 'NONE',  ( 0.000000000000000000, 1.000000000000000000, 0.000000000000000000 ) ) ;
#2972 = VECTOR ( 'NONE', #65029, 1000.000000000000000 ) ;
#2973 = ORIENTED_EDGE ( 'NONE', *, *, #92624, .T. ) ;
#2974 = AXIS2_PLACEMENT_3D ( 'NONE', #52789, #122189, #92724 ) ;
#2975 = DIRECTION ( 'NONE',  ( -4.274815082592931898E-19, -0.9999939076577903929, -0.003490651415223739937 ) ) ;
#2976 = ORIENTED_EDGE ( 'NONE', *, *, #26758, .T. ) ;
#2977 = PLANE ( 'NONE',  #102632 ) ;
#2978 = ORIENTED_EDGE ( 'NONE', *, *, #44260, .F. ) ;
#2979 = FACE_OUTER_BOUND ( 'NONE', #124618, .T. ) ;
#2980 = DIRECTION ( 'NONE',  ( 0.000000000000000000, 0.000000000000000000, 1.000000000000000000 ) ) ;
#2981 = EDGE_CURVE ( 'NONE', #62375, #7926, #50525, .T. ) ;
#2982 = FACE_OUTER_BOUND ( 'NONE', #6815, .T. ) ;
#2983 = EDGE_CURVE ( 'NONE', #58412, #8031, #122747, .T. ) ;
#2984 = DIRECTION ( 'NONE',  ( 0.000000000000000000, -0.9999939076577903929, 0.003490651415223739937 ) ) ;
#2985 = VERTEX_POINT ( 'NONE', #35035 ) ;
#2986 = CARTESIAN_POINT ( 'NONE',  ( -5.650000000000023448, 12.50000000000000000, -2.511473670974877948 ) ) ;
#2988 = CARTESIAN_POINT ( 'NONE',  ( -6.450000000000014388, 2.500000000000000000, 1.818653347947321475 ) ) ;
#2987 = AXIS2_PLACEMENT_3D ( 'NONE', #52892, #111820, #73806 ) ;
#2989 = VERTEX_POINT ( 'NONE', #25181 ) ;
#2990 = VERTEX_POINT ( 'NONE', #83484 ) ;
#2991 = AXIS2_PLACEMENT_3D ( 'NONE', #119516, #88780, #128735 ) ;
#2993 = ORIENTED_EDGE ( 'NONE', *, *, #72344, .F. ) ;
#2992 = ADVANCED_FACE ( 'NONE', ( #24545 ), #69299, .T. ) ;
#2994 = CARTESIAN_POINT ( 'NONE',  ( 17.50000000000000000, -2.750000000000000444, 2.864912725862981624 ) ) ;
#2995 = CARTESIAN_POINT ( 'NONE',  ( -11.84999999999999609, 12.50000000000000000, 2.511473670974873507 ) ) ;
#2996 = CARTESIAN_POINT ( 'NONE',  ( 186.0260416670080588, -6.551208109652273848, -3.782341765625003571 ) ) ;
#2997 = DIRECTION ( 'NONE',  ( -4.274815082592931898E-19, -0.9999939076577903929, -0.003490651415223739937 ) ) ;
#2998 = DIRECTION ( 'NONE',  ( 0.000000000000000000, 0.000000000000000000, -1.000000000000000000 ) ) ;
#2999 = AXIS2_PLACEMENT_3D ( 'NONE', #115365, #67568, #8641 ) ;
#3000 = CIRCLE ( 'NONE', #76154, 0.1000000000000000472 ) ;
#3001 = CARTESIAN_POINT ( 'NONE',  ( 5.599999999999931255, 12.50000000000000000, 4.611443907251934426 ) ) ;
#3002 = CIRCLE ( 'NONE', #49075, 0.06509327318403745899 ) ;
#3004 = VECTOR ( 'NONE', #101494, 1000.000000000000000 ) ;
#3003 = DIRECTION ( 'NONE',  ( 0.000000000000000000, 0.000000000000000000, -1.000000000000000000 ) ) ;
#3005 = CIRCLE ( 'NONE', #59164, 0.09999999999999999167 ) ;
#3006 = VECTOR ( 'NONE', #128243, 1000.000000000000000 ) ;
#3007 = FACE_OUTER_BOUND ( 'NONE', #64248, .T. ) ;
#3008 = AXIS2_PLACEMENT_3D ( 'NONE', #89189, #19810, #28993 ) ;
#3009 = EDGE_LOOP ( 'NONE', ( #20545, #20901, #29975, #29772 ) ) ;
#3010 = CARTESIAN_POINT ( 'NONE',  ( 10.64999999999991331, 12.50000000000000000, 6.148780366869520897 ) ) ;
#3011 = AXIS2_PLACEMENT_3D ( 'NONE', #16316, #66718, #57568 ) ;
#3012 = FACE_OUTER_BOUND ( 'NONE', #114721, .T. ) ;
#3013 = DIRECTION ( 'NONE',  ( 0.000000000000000000, 1.000000000000000000, 0.000000000000000000 ) ) ;
#3014 = CARTESIAN_POINT ( 'NONE',  ( -12.89999999999999147, 2.500000000000000000, -4.430127018922199511 ) ) ;
#3015 = ORIENTED_EDGE ( 'NONE', *, *, #25209, .T. ) ;
#3016 = DIRECTION ( 'NONE',  ( 0.000000000000000000, 0.000000000000000000, -1.000000000000000000 ) ) ;
#3017 = EDGE_CURVE ( 'NONE', #116336, #76857, #102465, .T. ) ;
#3018 = DIRECTION ( 'NONE',  ( 0.000000000000000000, 1.000000000000000000, 0.000000000000000000 ) ) ;
#3020 = ORIENTED_EDGE ( 'NONE', *, *, #25234, .F. ) ;
#3019 = CARTESIAN_POINT ( 'NONE',  ( -4.550000000000022915, 2.500000000000000000, 2.065063509461097624 ) ) ;
#3021 = EDGE_CURVE ( 'NONE', #64709, #48204, #114844, .T. ) ;
#3022 = ADVANCED_FACE ( 'NONE', ( #65094 ), #7579, .T. ) ;
#3023 = EDGE_CURVE ( 'NONE', #116228, #101562, #107943, .T. ) ;
#3024 = EDGE_CURVE ( 'NONE', #82135, #52320, #124030, .T. ) ;
#3025 = AXIS2_PLACEMENT_3D ( 'NONE', #13275, #129391, #93151 ) ;
#3026 = ORIENTED_EDGE ( 'NONE', *, *, #45395, .T. ) ;
#3027 = CARTESIAN_POINT ( 'NONE',  ( 187.5000000000000000, 0.000000000000000000, 0.000000000000000000 ) ) ;
#3028 = ORIENTED_EDGE ( 'NONE', *, *, #25160, .T. ) ;
#3029 = ORIENTED_EDGE ( 'NONE', *, *, #63770, .F. ) ;
#3030 = DIRECTION ( 'NONE',  ( 0.000000000000000000, 0.000000000000000000, -1.000000000000000000 ) ) ;
#3031 = ADVANCED_FACE ( 'NONE', ( #74300 ), #24316, .T. ) ;
#3032 = EDGE_CURVE ( 'NONE', #54523, #77368, #112292, .T. ) ;
#3033 = FACE_OUTER_BOUND ( 'NONE', #126812, .T. ) ;
#3034 = CARTESIAN_POINT ( 'NONE',  ( 11.04999999999991189, 2.500000000000000000, -2.511473670974877948 ) ) ;
#3035 = CONICAL_SURFACE ( 'NONE', #76199, 0.09999999999999982514, 0.003490658503988666988 ) ;
#3036 = DIRECTION ( 'NONE',  ( -4.274815082592931898E-19, -0.9999939076577903929, -0.003490651415223739937 ) ) ;
#3037 = AXIS2_PLACEMENT_3D ( 'NONE', #117006, #94815, #95461 ) ;
#3038 = ORIENTED_EDGE ( 'NONE', *, *, #37626, .F. ) ;
#3039 = ADVANCED_FACE ( 'NONE', ( #2979 ), #120464, .T. ) ;
#3040 = DIRECTION ( 'NONE',  ( -0.000000000000000000, -1.000000000000000000, -0.000000000000000000 ) ) ;
#3042 = VERTEX_POINT ( 'NONE', #44844 ) ;
#3041 = DIRECTION ( 'NONE',  ( 0.000000000000000000, 0.000000000000000000, 1.000000000000000000 ) ) ;
#3043 = CARTESIAN_POINT ( 'NONE',  ( -4.400000000000025224, 2.500000000000000000, -0.3464101615137783474 ) ) ;
#3044 = EDGE_CURVE ( 'NONE', #6762, #4367, #57777, .T. ) ;
#3045 = PLANE ( 'NONE',  #46671 ) ;
#3046 = EDGE_CURVE ( 'NONE', #52919, #15089, #74493, .T. ) ;
#3047 = EDGE_LOOP ( 'NONE', ( #37865, #56529 ) ) ;
#3048 = CIRCLE ( 'NONE', #894, 0.1000000000000002554 ) ;
#3049 = EDGE_LOOP ( 'NONE', ( #103305, #32878, #103032, #76036 ) ) ;
#3051 = VERTEX_POINT ( 'NONE', #82843 ) ;
#3050 = AXIS2_PLACEMENT_3D ( 'NONE', #94328, #94996, #75989 ) ;
#3052 = ORIENTED_EDGE ( 'NONE', *, *, #92624, .F. ) ;
#3053 = FACE_OUTER_BOUND ( 'NONE', #37505, .T. ) ;
#3054 = CARTESIAN_POINT ( 'NONE',  ( 16.04744068708516025, 2.499999999999872546, 6.586254740842515609 ) ) ;
#3055 = CARTESIAN_POINT ( 'NONE',  ( -11.05000000000000071, 12.50000000000000000, -2.576566944158911188 ) ) ;
#3056 = FACE_BOUND ( 'NONE', #124023, .T. ) ;
#3057 = ORIENTED_EDGE ( 'NONE', *, *, #18254, .F. ) ;
#3058 = CARTESIAN_POINT ( 'NONE',  ( 185.7395833340161460, 4.445597072760117285, 7.699999999999999289 ) ) ;
#3059 = CARTESIAN_POINT ( 'NONE',  ( -2.300000000000032685, 2.500000000000000000, -0.3464101615137783474 ) ) ;
#3060 = CARTESIAN_POINT ( 'NONE',  ( -2.950000000000030376, 12.50000000000000000, 6.430097255199259010 ) ) ;
#3061 = AXIS2_PLACEMENT_3D ( 'NONE', #37978, #34461, #10451 ) ;
#3062 = AXIS2_PLACEMENT_3D ( 'NONE', #119924, #70185, #20434 ) ;
#3063 = DIRECTION ( 'NONE',  ( 0.000000000000000000, -0.9999939076577903929, 0.003490651415223739937 ) ) ;
#3064 = DIRECTION ( 'NONE',  ( 0.000000000000000000, -0.9999939076577903929, 0.003490651415223739937 ) ) ;
#3065 = AXIS2_PLACEMENT_3D ( 'NONE', #91139, #1457, #12561 ) ;
#3066 = FACE_OUTER_BOUND ( 'NONE', #14518, .T. ) ;
#3067 = AXIS2_PLACEMENT_3D ( 'NONE', #28494, #69048, #99815 ) ;
#3068 = DIRECTION ( 'NONE',  ( 0.000000000000000000, 1.000000000000000000, 0.000000000000000000 ) ) ;
#3069 = ORIENTED_EDGE ( 'NONE', *, *, #64210, .F. ) ;
#3070 = VERTEX_POINT ( 'NONE', #73004 ) ;
#3071 = VERTEX_POINT ( 'NONE', #94564 ) ;
#3072 = VERTEX_POINT ( 'NONE', #68334 ) ;
#3073 = ORIENTED_EDGE ( 'NONE', *, *, #99203, .F. ) ;
#3074 = DIRECTION ( 'NONE',  ( 0.000000000000000000, 1.000000000000000000, 0.000000000000000000 ) ) ;
#3075 = DIRECTION ( 'NONE',  ( 0.000000000000000000, 0.000000000000000000, 1.000000000000000000 ) ) ;
#3076 = VERTEX_POINT ( 'NONE', #46776 ) ;
#3077 = FACE_BOUND ( 'NONE', #112096, .T. ) ;
#3078 = FACE_OUTER_BOUND ( 'NONE', #69946, .T. ) ;
#3079 = EDGE_CURVE ( 'NONE', #29857, #85157, #97479, .T. ) ;
#3080 = AXIS2_PLACEMENT_3D ( 'NONE', #29399, #68662, #129548 ) ;
#3081 = AXIS2_PLACEMENT_3D ( 'NONE', #37127, #124854, #65920 ) ;
#3082 = ADVANCED_FACE ( 'NONE', ( #125325 ), #70299, .T. ) ;
#3084 = VERTEX_POINT ( 'NONE', #67025 ) ;
#3083 = AXIS2_PLACEMENT_3D ( 'NONE', #36324, #36955, #34392 ) ;
#3085 = AXIS2_PLACEMENT_3D ( 'NONE', #32267, #20012, #59958 ) ;
#3086 = CARTESIAN_POINT ( 'NONE',  ( -0.8500000000000382805, 2.500000000000000000, -5.802370205355749988 ) ) ;
#3087 = CARTESIAN_POINT ( 'NONE',  ( 14.14999999999989200, 2.500000000000000000, -2.165063509461101710 ) ) ;
#3088 = CARTESIAN_POINT ( 'NONE',  ( 3.549999999999944755, 2.500000000000000000, -2.411473670974877859 ) ) ;
#3089 = ORIENTED_EDGE ( 'NONE', *, *, #82819, .T. ) ;
#3090 = CARTESIAN_POINT ( 'NONE',  ( 9.349999999999916156, 12.50000000000000000, -2.576566944158915184 ) ) ;
#3091 = CONICAL_SURFACE ( 'NONE', #126331, 0.09999999999999982514, 0.003490658503988666988 ) ;
#3092 = ORIENTED_EDGE ( 'NONE', *, *, #13804, .T. ) ;
#3093 = CONICAL_SURFACE ( 'NONE', #99240, 0.09999999999999982514, 0.003490658503988666988 ) ;
#3094 = ORIENTED_EDGE ( 'NONE', *, *, #84045, .F. ) ;
#3095 = ORIENTED_EDGE ( 'NONE', *, *, #111499, .F. ) ;
#3096 = DIRECTION ( 'NONE',  ( 0.000000000000000000, 1.000000000000000000, 0.000000000000000000 ) ) ;
#3097 = DIRECTION ( 'NONE',  ( -0.000000000000000000, -1.000000000000000000, -0.000000000000000000 ) ) ;
#3098 = DIRECTION ( 'NONE',  ( -0.000000000000000000, -1.000000000000000000, -0.000000000000000000 ) ) ;
#3099 = EDGE_LOOP ( 'NONE', ( #37012, #43985 ) ) ;
#3100 = LINE ( 'NONE', #123496, #99753 ) ;
#3101 = CIRCLE ( 'NONE', #63737, 0.06509327318403743123 ) ;
#3102 = VECTOR ( 'NONE', #47038, 1000.000000000000000 ) ;
#3103 = CARTESIAN_POINT ( 'NONE',  ( 11.89999999999990798, 2.500000000000000000, 3.983716857408420964 ) ) ;
#3104 = FACE_OUTER_BOUND ( 'NONE', #129495, .T. ) ;
#3105 = CARTESIAN_POINT ( 'NONE',  ( 186.1145833340161175, 6.668395609140177704, -3.849999999999998312 ) ) ;
#3107 = VERTEX_POINT ( 'NONE', #57226 ) ;
#3106 = CONICAL_SURFACE ( 'NONE', #76263, 0.1000000000000002554, 0.003490658503988666988 ) ;
#3108 = DIRECTION ( 'NONE',  ( 0.000000000000000000, 1.000000000000000000, 0.000000000000000000 ) ) ;
#3109 = EDGE_LOOP ( 'NONE', ( #35902, #44593, #14054, #105016 ) ) ;
#3110 = CARTESIAN_POINT ( 'NONE',  ( 6.249999999999965361, 12.50000000000000000, 2.165063509461097713 ) ) ;
#3111 = EDGE_LOOP ( 'NONE', ( #75458, #9768 ) ) ;
#3112 = VERTEX_POINT ( 'NONE', #77510 ) ;
#3113 = CARTESIAN_POINT ( 'NONE',  ( 14.14999999999989733, 2.500000000000000000, 2.757883832488649656 ) ) ;
#3114 = DIRECTION ( 'NONE',  ( 0.000000000000000000, 0.000000000000000000, 1.000000000000000000 ) ) ;
#3115 = DIRECTION ( 'NONE',  ( 0.000000000000000000, -0.9999939076577903929, 0.003490651415223739937 ) ) ;
#3116 = DIRECTION ( 'NONE',  ( -0.000000000000000000, 1.000000000000000000, -0.000000000000000000 ) ) ;
#3117 = DIRECTION ( 'NONE',  ( 0.000000000000000000, 0.000000000000000000, 1.000000000000000000 ) ) ;
#3118 = CONICAL_SURFACE ( 'NONE', #80578, 0.09999999999999982514, 0.003490658503988666988 ) ;
#3119 = EDGE_LOOP ( 'NONE', ( #89447, #27038 ) ) ;
#3120 = VERTEX_POINT ( 'NONE', #95229 ) ;
#3121 = EDGE_CURVE ( 'NONE', #76595, #38808, #22287, .T. ) ;
#3122 = CARTESIAN_POINT ( 'NONE',  ( 12.69999999999990337, 2.500000000000000000, -4.776537180435978414 ) ) ;
#3123 = FACE_BOUND ( 'NONE', #89319, .T. ) ;
#3124 = FACE_OUTER_BOUND ( 'NONE', #45226, .T. ) ;
#3125 = VERTEX_POINT ( 'NONE', #38248 ) ;
#3126 = ORIENTED_EDGE ( 'NONE', *, *, #54598, .T. ) ;
#3127 = CARTESIAN_POINT ( 'NONE',  ( 10.84999999999990905, 2.500000000000000000, -5.702370205355749455 ) ) ;
#3128 = AXIS2_PLACEMENT_3D ( 'NONE', #80850, #53330, #120767 ) ;
#3129 = ORIENTED_EDGE ( 'NONE', *, *, #112470, .F. ) ;
#3131 = ADVANCED_FACE ( 'NONE', ( #127905 ), #85398, .T. ) ;
#3130 = CARTESIAN_POINT ( 'NONE',  ( 8.749999999999923617, 12.50000000000000000, 1.472243186433545459 ) ) ;
#3133 = CONICAL_SURFACE ( 'NONE', #53309, 0.1000000000000002554, 0.003490658503988666988 ) ;
#3132 = CARTESIAN_POINT ( 'NONE',  ( -6.650000000000018119, 12.50000000000000000, -2.165063509461101710 ) ) ;
#3134 = CARTESIAN_POINT ( 'NONE',  ( 2.899999999999944844, 2.500000000000000000, 3.737306695894644371 ) ) ;
#3135 = VERTEX_POINT ( 'NONE', #75569 ) ;
#3136 = PLANE ( 'NONE',  #92070 ) ;
#3137 = DIRECTION ( 'NONE',  ( 0.000000000000000000, 0.000000000000000000, -1.000000000000000000 ) ) ;
#3138 = CARTESIAN_POINT ( 'NONE',  ( 14.54999999999989591, 2.500000000000000000, 2.165063509461097713 ) ) ;
#3139 = CARTESIAN_POINT ( 'NONE',  ( 1.449999999999949551, 2.500000000000000000, 6.941600689897073018 ) ) ;
#3140 = ADVANCED_FACE ( 'NONE', ( #76235 ), #28528, .T. ) ;
#3141 = EDGE_CURVE ( 'NONE', #1889, #72667, #15996, .T. ) ;
#3142 = CARTESIAN_POINT ( 'NONE',  ( 5.799999999999931433, 2.500000000000000000, 4.330127018922196314 ) ) ;
#3143 = EDGE_LOOP ( 'NONE', ( #79118, #76165, #78870, #53190 ) ) ;
#3144 = AXIS2_PLACEMENT_3D ( 'NONE', #3514, #43453, #64357 ) ;
#3145 = DIRECTION ( 'NONE',  ( 0.000000000000000000, 0.000000000000000000, -1.000000000000000000 ) ) ;
#3147 = AXIS2_PLACEMENT_3D ( 'NONE', #40616, #32719, #100768 ) ;
#3146 = CARTESIAN_POINT ( 'NONE',  ( 81.97643238289522571, -3.858501988011899364, 6.173828414998187242 ) ) ;
#3148 = EDGE_LOOP ( 'NONE', ( #36468, #56392, #8981, #100650 ) ) ;
#3149 = ORIENTED_EDGE ( 'NONE', *, *, #1377, .F. ) ;
#3150 = EDGE_CURVE ( 'NONE', #46254, #96832, #45252, .T. ) ;
#3151 = CARTESIAN_POINT ( 'NONE',  ( 186.3385416670080872, 6.551208109652274736, 3.782341765625001351 ) ) ;
#3152 = DIRECTION ( 'NONE',  ( 0.000000000000000000, -0.000000000000000000, 1.000000000000000000 ) ) ;
#3153 = DIRECTION ( 'NONE',  ( 0.000000000000000000, 0.000000000000000000, 1.000000000000000000 ) ) ;
#3154 = PLANE ( 'NONE',  #84551 ) ;
#3155 = CARTESIAN_POINT ( 'NONE',  ( -0.8000000000000315747, 12.50000000000000000, 0.000000000000000000 ) ) ;
#3156 = VECTOR ( 'NONE', #88026, 1000.000000000000000 ) ;
#3157 = FACE_OUTER_BOUND ( 'NONE', #125977, .T. ) ;
#3158 = AXIS2_PLACEMENT_3D ( 'NONE', #12720, #52033, #51401 ) ;
#3159 = CARTESIAN_POINT ( 'NONE',  ( -0.2000000000000347888, 12.50000000000000000, 0.4115034346978132529 ) ) ;
#3160 = DIRECTION ( 'NONE',  ( -0.000000000000000000, 1.000000000000000000, -0.000000000000000000 ) ) ;
#3161 = DIRECTION ( 'NONE',  ( 0.000000000000000000, 0.000000000000000000, 1.000000000000000000 ) ) ;
#3162 = DIRECTION ( 'NONE',  ( 1.000000000000000000, 0.000000000000000000, 0.000000000000000000 ) ) ;
#3163 = ORIENTED_EDGE ( 'NONE', *, *, #14410, .T. ) ;
#3164 = VERTEX_POINT ( 'NONE', #27129 ) ;
#3165 = ORIENTED_EDGE ( 'NONE', *, *, #101283, .T. ) ;
#3166 = ORIENTED_EDGE ( 'NONE', *, *, #62858, .T. ) ;
#3167 = AXIS2_PLACEMENT_3D ( 'NONE', #106632, #17599, #57544 ) ;
#3168 = DIRECTION ( 'NONE',  ( 0.000000000000000000, 1.000000000000000000, 0.000000000000000000 ) ) ;
#3169 = DIRECTION ( 'NONE',  ( 0.000000000000000000, 0.000000000000000000, 1.000000000000000000 ) ) ;
#3170 = ORIENTED_EDGE ( 'NONE', *, *, #30964, .F. ) ;
#3171 = DIRECTION ( 'NONE',  ( 0.000000000000000000, 0.000000000000000000, 1.000000000000000000 ) ) ;
#3172 = ADVANCED_FACE ( 'NONE', ( #26489 ), #25838, .T. ) ;
#3173 = AXIS2_PLACEMENT_3D ( 'NONE', #121620, #113095, #92830 ) ;
#3174 = VECTOR ( 'NONE', #45511, 1000.000000000000000 ) ;
#3175 = CARTESIAN_POINT ( 'NONE',  ( -6.450000000000017941, 12.50000000000000000, -2.576566944158915184 ) ) ;
#3177 = ORIENTED_EDGE ( 'NONE', *, *, #33618, .T. ) ;
#3176 = DIRECTION ( 'NONE',  ( 0.000000000000000000, 0.000000000000000000, -1.000000000000000000 ) ) ;
#3178 = AXIS2_PLACEMENT_3D ( 'NONE', #34185, #119477, #62360 ) ;
#3179 = EDGE_CURVE ( 'NONE', #103010, #37632, #5519, .T. ) ;
#3180 = DIRECTION ( 'NONE',  ( -0.000000000000000000, -1.000000000000000000, -0.000000000000000000 ) ) ;
#3181 = EDGE_CURVE ( 'NONE', #66905, #53623, #78713, .T. ) ;
#3182 = FACE_OUTER_BOUND ( 'NONE', #27854, .T. ) ;
#3183 = EDGE_LOOP ( 'NONE', ( #31064, #3649 ) ) ;
#3184 = CONICAL_SURFACE ( 'NONE', #21976, 0.1000000000000000472, 0.003490658503988666988 ) ;
#3185 = AXIS2_PLACEMENT_3D ( 'NONE', #58803, #90164, #78459 ) ;
#3186 = VERTEX_POINT ( 'NONE', #6177 ) ;
#3187 = ORIENTED_EDGE ( 'NONE', *, *, #69092, .F. ) ;
#3188 = ORIENTED_EDGE ( 'NONE', *, *, #119566, .T. ) ;
#3189 = DIRECTION ( 'NONE',  ( -4.274815082592931898E-19, -0.9999939076577903929, -0.003490651415223739937 ) ) ;
#3190 = EDGE_CURVE ( 'NONE', #90210, #1124, #55934, .T. ) ;
#3191 = AXIS2_PLACEMENT_3D ( 'NONE', #54829, #84300, #112485 ) ;
#3192 = EDGE_CURVE ( 'NONE', #105778, #128794, #30601, .T. ) ;
#3193 = EDGE_CURVE ( 'NONE', #125237, #48297, #19068, .T. ) ;
#3194 = EDGE_CURVE ( 'NONE', #123846, #56415, #9651, .T. ) ;
#3195 = DIRECTION ( 'NONE',  ( 0.000000000000000000, 0.000000000000000000, 1.000000000000000000 ) ) ;
#3196 = DIRECTION ( 'NONE',  ( -0.000000000000000000, -1.000000000000000000, -0.000000000000000000 ) ) ;
#3197 = CIRCLE ( 'NONE', #65872, 0.1000000000000002554 ) ;
#3198 = FACE_OUTER_BOUND ( 'NONE', #16127, .T. ) ;
#3199 = ORIENTED_EDGE ( 'NONE', *, *, #101344, .T. ) ;
#3200 = EDGE_CURVE ( 'NONE', #28676, #68600, #73321, .T. ) ;
#3201 = CARTESIAN_POINT ( 'NONE',  ( -0.2000000000000347888, 12.50000000000000000, 0.3464101615137758494 ) ) ;
#3202 = EDGE_LOOP ( 'NONE', ( #2920, #95882 ) ) ;
#3203 = DIRECTION ( 'NONE',  ( -1.000000000000000000, 0.000000000000000000, 1.224646799147352221E-16 ) ) ;
#3204 = CARTESIAN_POINT ( 'NONE',  ( 10.19999999999991402, 2.500000000000000000, 0.2464101615137735679 ) ) ;
#3205 = DIRECTION ( 'NONE',  ( 0.000000000000000000, 1.000000000000000000, 0.000000000000000000 ) ) ;
#3206 = DIRECTION ( 'NONE',  ( 0.000000000000000000, -0.000000000000000000, 1.000000000000000000 ) ) ;
#3207 = EDGE_CURVE ( 'NONE', #46500, #62111, #76554, .T. ) ;
#3208 = ORIENTED_EDGE ( 'NONE', *, *, #10125, .F. ) ;
#3209 = ORIENTED_EDGE ( 'NONE', *, *, #101429, .T. ) ;
#3210 = ORIENTED_EDGE ( 'NONE', *, *, #6742, .F. ) ;
#3211 = LINE ( 'NONE', #72593, #63639 ) ;
#3212 = DIRECTION ( 'NONE',  ( 0.000000000000000000, 0.000000000000000000, -1.000000000000000000 ) ) ;
#3213 = CARTESIAN_POINT ( 'NONE',  ( -8.150000000000014566, 12.50000000000000000, -6.841600689897073373 ) ) ;
#3214 = FACE_BOUND ( 'NONE', #48634, .T. ) ;
#3215 = DIRECTION ( 'NONE',  ( 0.000000000000000000, -0.000000000000000000, 1.000000000000000000 ) ) ;
#3216 = CIRCLE ( 'NONE', #84775, 0.06509327318403745899 ) ;
#3217 = CARTESIAN_POINT ( 'NONE',  ( 4.149999999999938183, 2.500000000000000000, 2.165063509461097713 ) ) ;
#3218 = DIRECTION ( 'NONE',  ( 0.000000000000000000, 0.000000000000000000, 1.000000000000000000 ) ) ;
#3219 = DIRECTION ( 'NONE',  ( 0.000000000000000000, -0.9999939076577903929, 0.003490651415223739937 ) ) ;
#3220 = CIRCLE ( 'NONE', #76379, 0.1000000000000000472 ) ;
#3221 = CARTESIAN_POINT ( 'NONE',  ( 9.349999999999919709, 2.500000000000000000, 2.511473670974873507 ) ) ;
#3222 = DIRECTION ( 'NONE',  ( 0.000000000000000000, -0.000000000000000000, 1.000000000000000000 ) ) ;
#3223 = ORIENTED_EDGE ( 'NONE', *, *, #98933, .T. ) ;
#3224 = AXIS2_PLACEMENT_3D ( 'NONE', #41557, #22562, #33027 ) ;
#3225 = AXIS2_PLACEMENT_3D ( 'NONE', #95306, #24634, #65830 ) ;
#3226 = LINE ( 'NONE', #33969, #39176 ) ;
#3227 = ORIENTED_EDGE ( 'NONE', *, *, #117370, .F. ) ;
#3228 = ORIENTED_EDGE ( 'NONE', *, *, #82126, .F. ) ;
#3229 = CARTESIAN_POINT ( 'NONE',  ( -0.8500000000000390576, 12.50000000000000000, -6.560283801567339701 ) ) ;
#3230 = CARTESIAN_POINT ( 'NONE',  ( 11.64999999999990798, 12.50000000000000000, -1.472243186433550122 ) ) ;
#3231 = FACE_BOUND ( 'NONE', #114809, .T. ) ;
#3232 = DIRECTION ( 'NONE',  ( 0.000000000000000000, 0.000000000000000000, -1.000000000000000000 ) ) ;
#3233 = AXIS2_PLACEMENT_3D ( 'NONE', #32196, #44570, #22370 ) ;
#3234 = EDGE_CURVE ( 'NONE', #108123, #128150, #14120, .T. ) ;
#3235 = CONICAL_SURFACE ( 'NONE', #32500, 0.1000000000000000472, 0.003490658503988666988 ) ;
#3236 = ORIENTED_EDGE ( 'NONE', *, *, #104536, .F. ) ;
#3237 = CARTESIAN_POINT ( 'NONE',  ( 76.40063402955621541, 3.742348971392434720, 5.987205606707019179 ) ) ;
#3238 = CARTESIAN_POINT ( 'NONE',  ( 12.94999999999990337, 12.50000000000000000, 2.230156782645134950 ) ) ;
#3239 = EDGE_LOOP ( 'NONE', ( #95473, #118055, #106806, #110930 ) ) ;
#3240 = PLANE ( 'NONE',  #49084 ) ;
#3241 = PLANE ( 'NONE',  #1070 ) ;
#3242 = EDGE_CURVE ( 'NONE', #66905, #32401, #48712, .T. ) ;
#3243 = AXIS2_PLACEMENT_3D ( 'NONE', #124759, #114922, #6246 ) ;
#3244 = CIRCLE ( 'NONE', #128659, 0.06509327318403745899 ) ;
#3245 = VERTEX_POINT ( 'NONE', #1521 ) ;
#3246 = DIRECTION ( 'NONE',  ( 0.000000000000000000, 0.000000000000000000, -1.000000000000000000 ) ) ;
#3247 = DIRECTION ( 'NONE',  ( 0.000000000000000000, 0.000000000000000000, 1.000000000000000000 ) ) ;
#3248 = VERTEX_POINT ( 'NONE', #39559 ) ;
#3249 = CARTESIAN_POINT ( 'NONE',  ( -7.700000000000016165, 2.500000000000000000, 0.4464101615137735513 ) ) ;
#3250 = FACE_OUTER_BOUND ( 'NONE', #34596, .T. ) ;
#3251 = DIRECTION ( 'NONE',  ( -0.000000000000000000, -1.000000000000000000, -0.000000000000000000 ) ) ;
#3252 = VERTEX_POINT ( 'NONE', #110830 ) ;
#3253 = ORIENTED_EDGE ( 'NONE', *, *, #121232, .T. ) ;
#3254 = DIRECTION ( 'NONE',  ( 0.000000000000000000, 0.000000000000000000, 1.000000000000000000 ) ) ;
#3255 = VECTOR ( 'NONE', #99409, 1000.000000000000000 ) ;
#3256 = VERTEX_POINT ( 'NONE', #61098 ) ;
#3257 = CARTESIAN_POINT ( 'NONE',  ( 7.499999999999961808, 2.500000000000000000, -4.330127018922201643 ) ) ;
#3258 = DIRECTION ( 'NONE',  ( 0.000000000000000000, 0.000000000000000000, 1.000000000000000000 ) ) ;
#3259 = AXIS2_PLACEMENT_3D ( 'NONE', #22590, #93245, #23862 ) ;
#3260 = EDGE_LOOP ( 'NONE', ( #11597, #49169, #79485, #33805 ) ) ;
#3261 = CIRCLE ( 'NONE', #118266, 0.06509327318403745899 ) ;
#3262 = DIRECTION ( 'NONE',  ( 0.000000000000000000, 0.000000000000000000, 1.000000000000000000 ) ) ;
#3263 = CARTESIAN_POINT ( 'NONE',  ( 8.949999999999919353, 2.500000000000000000, -6.148780366869526226 ) ) ;
#3264 = DIRECTION ( 'NONE',  ( 0.000000000000000000, 0.000000000000000000, 1.000000000000000000 ) ) ;
#3265 = CARTESIAN_POINT ( 'NONE',  ( 11.69999999999990514, 12.50000000000000000, -0.06509327318403970719 ) ) ;
#3266 = CARTESIAN_POINT ( 'NONE',  ( 6.699999999999928235, 12.50000000000000000, 0.06509327318403515528 ) ) ;
#3267 = EDGE_LOOP ( 'NONE', ( #60453, #36787 ) ) ;
#3269 = ORIENTED_EDGE ( 'NONE', *, *, #78576, .T. ) ;
#3268 = ADVANCED_FACE ( 'NONE', ( #59842 ), #85140, .T. ) ;
#3270 = FACE_OUTER_BOUND ( 'NONE', #73156, .T. ) ;
#3271 = ORIENTED_EDGE ( 'NONE', *, *, #84429, .F. ) ;
#3272 = CARTESIAN_POINT ( 'NONE',  ( -9.550000000000006040, 2.500000000000000000, -2.065063509461102065 ) ) ;
#3274 = ORIENTED_EDGE ( 'NONE', *, *, #57367, .T. ) ;
#3273 = ORIENTED_EDGE ( 'NONE', *, *, #8608, .T. ) ;
#3275 = ORIENTED_EDGE ( 'NONE', *, *, #29635, .T. ) ;
#3276 = CARTESIAN_POINT ( 'NONE',  ( -0.2000000000000404232, 2.500000000000000000, 3.983716857408420964 ) ) ;
#3277 = AXIS2_PLACEMENT_3D ( 'NONE', #31653, #10079, #71568 ) ;
#3279 = EDGE_CURVE ( 'NONE', #44934, #5550, #68415, .T. ) ;
#3278 = PLANE ( 'NONE',  #6707 ) ;
#3280 = PLANE ( 'NONE',  #89438 ) ;
#3281 = VECTOR ( 'NONE', #67002, 1000.000000000000000 ) ;
#3282 = CARTESIAN_POINT ( 'NONE',  ( -2.300000000000033573, 2.500000000000000000, 0.3464101615137735735 ) ) ;
#3283 = CARTESIAN_POINT ( 'NONE',  ( -10.65000000000000213, 12.50000000000000000, 6.148780366869520009 ) ) ;
#3284 = DIRECTION ( 'NONE',  ( 0.000000000000000000, 1.000000000000000000, 0.000000000000000000 ) ) ;
#3285 = CIRCLE ( 'NONE', #53466, 0.1000000000000002554 ) ;
#3286 = DIRECTION ( 'NONE',  ( -4.274815082592931898E-19, -0.9999939076577903929, -0.003490651415223739937 ) ) ;
#3287 = CARTESIAN_POINT ( 'NONE',  ( -5.450000000000023270, 2.500000000000000000, -6.395190528383301931 ) ) ;
#3288 = ADVANCED_FACE ( 'NONE', ( #78825 ), #87288, .T. ) ;
#3289 = EDGE_CURVE ( 'NONE', #79919, #64213, #9935, .T. ) ;
#3290 = DIRECTION ( 'NONE',  ( -0.000000000000000000, -1.000000000000000000, -0.000000000000000000 ) ) ;
#3291 = EDGE_LOOP ( 'NONE', ( #19664, #66763, #117659, #25180 ) ) ;
#3292 = EDGE_CURVE ( 'NONE', #25992, #65903, #30888, .T. ) ;
#3293 = DIRECTION ( 'NONE',  ( 0.000000000000000000, -0.000000000000000000, 1.000000000000000000 ) ) ;
#3294 = VERTEX_POINT ( 'NONE', #23582 ) ;
#3295 = VERTEX_POINT ( 'NONE', #24236 ) ;
#3296 = ADVANCED_FACE ( 'NONE', ( #113913 ), #93558, .T. ) ;
#3297 = FACE_OUTER_BOUND ( 'NONE', #59393, .T. ) ;
#3298 = DIRECTION ( 'NONE',  ( 0.000000000000000000, 1.000000000000000000, 0.000000000000000000 ) ) ;
#3299 = CARTESIAN_POINT ( 'NONE',  ( 11.89999999999990443, 2.500000000000000000, -0.3464101615137782364 ) ) ;
#3300 = FACE_OUTER_BOUND ( 'NONE', #67755, .T. ) ;
#3301 = CARTESIAN_POINT ( 'NONE',  ( 8.949999999999915801, 2.500000000000000000, 6.741600689897071952 ) ) ;
#3302 = CARTESIAN_POINT ( 'NONE',  ( 3.099999999999945022, 2.500000000000000000, -4.676537180435978769 ) ) ;
#3303 = LINE ( 'NONE', #44509, #82355 ) ;
#3304 = ORIENTED_EDGE ( 'NONE', *, *, #31227, .T. ) ;
#3305 = AXIS2_PLACEMENT_3D ( 'NONE', #96929, #7249, #47204 ) ;
#3306 = CONICAL_SURFACE ( 'NONE', #61904, 0.1000000000000002554, 0.003490658503988666988 ) ;
#3307 = AXIS2_PLACEMENT_3D ( 'NONE', #51382, #91282, #41560 ) ;
#3308 = CARTESIAN_POINT ( 'NONE',  ( -9.400000000000007461, 2.500000000000000000, 0.3464101615137735735 ) ) ;
#3309 = VERTEX_POINT ( 'NONE', #34058 ) ;
#3310 = VERTEX_POINT ( 'NONE', #45173 ) ;
#3311 = AXIS2_PLACEMENT_3D ( 'NONE', #15755, #46508, #5925 ) ;
#3312 = ORIENTED_EDGE ( 'NONE', *, *, #13815, .T. ) ;
#3313 = ORIENTED_EDGE ( 'NONE', *, *, #12967, .T. ) ;
#3314 = DIRECTION ( 'NONE',  ( 0.000000000000000000, 0.000000000000000000, -1.000000000000000000 ) ) ;
#3315 = DIRECTION ( 'NONE',  ( 0.000000000000000000, 1.000000000000000000, 0.000000000000000000 ) ) ;
#3316 = AXIS2_PLACEMENT_3D ( 'NONE', #100120, #81130, #29447 ) ;
#3317 = DIRECTION ( 'NONE',  ( 0.000000000000000000, 0.000000000000000000, -1.000000000000000000 ) ) ;
#3318 = DIRECTION ( 'NONE',  ( 0.000000000000000000, 0.000000000000000000, 1.000000000000000000 ) ) ;
#3320 = VECTOR ( 'NONE', #123485, 1000.000000000000000 ) ;
#3319 = CONICAL_SURFACE ( 'NONE', #76487, 0.1000000000000000056, 0.003490658503988666988 ) ;
#3321 = DIRECTION ( 'NONE',  ( 0.000000000000000000, 1.000000000000000000, 0.000000000000000000 ) ) ;
#3322 = ORIENTED_EDGE ( 'NONE', *, *, #48692, .T. ) ;
#3323 = DIRECTION ( 'NONE',  ( 0.000000000000000000, 0.000000000000000000, 1.000000000000000000 ) ) ;
#3324 = DIRECTION ( 'NONE',  ( 0.000000000000000000, 0.000000000000000000, -1.000000000000000000 ) ) ;
#3325 = CARTESIAN_POINT ( 'NONE',  ( -9.150000000000005684, 2.500000000000000000, 7.088010851410848190 ) ) ;
#3326 = CARTESIAN_POINT ( 'NONE',  ( -2.900000000000029221, 2.500000000000000000, -4.330127018922201643 ) ) ;
#3327 = EDGE_LOOP ( 'NONE', ( #24274, #100808 ) ) ;
#3328 = AXIS2_PLACEMENT_3D ( 'NONE', #73554, #113487, #123947 ) ;
#3329 = CIRCLE ( 'NONE', #86945, 0.1000000000000002554 ) ;
#3330 = ORIENTED_EDGE ( 'NONE', *, *, #128664, .T. ) ;
#3331 = VERTEX_POINT ( 'NONE', #56263 ) ;
#3332 = EDGE_CURVE ( 'NONE', #74337, #37904, #82828, .T. ) ;
#3333 = CARTESIAN_POINT ( 'NONE',  ( 4.999999999999936939, 12.50000000000000000, -3.702399969078687292 ) ) ;
#3334 = EDGE_CURVE ( 'NONE', #129288, #48344, #110009, .T. ) ;
#3335 = ADVANCED_FACE ( 'NONE', ( #35350 ), #66078, .T. ) ;
#3336 = EDGE_CURVE ( 'NONE', #106026, #55502, #20118, .T. ) ;
#3337 = LINE ( 'NONE', #123728, #92547 ) ;
#3338 = CARTESIAN_POINT ( 'NONE',  ( -1.450000000000035039, 2.500000000000000000, -6.941600689897077459 ) ) ;
#3339 = ADVANCED_FACE ( 'NONE', ( #24879 ), #89359, .T. ) ;
#3340 = ORIENTED_EDGE ( 'NONE', *, *, #86447, .T. ) ;
#3341 = DIRECTION ( 'NONE',  ( -4.274815082592931898E-19, -0.9999939076577903929, -0.003490651415223739937 ) ) ;
#3342 = DIRECTION ( 'NONE',  ( 0.000000000000000000, 0.000000000000000000, -1.000000000000000000 ) ) ;
#3343 = LINE ( 'NONE', #54370, #62995 ) ;
#3344 = CARTESIAN_POINT ( 'NONE',  ( 8.149999999999920419, 12.50000000000000000, 6.213873640053559022 ) ) ;
#3345 = EDGE_CURVE ( 'NONE', #112688, #120493, #76845, .T. ) ;
#3346 = EDGE_CURVE ( 'NONE', #39693, #3135, #108131, .T. ) ;
#3347 = CIRCLE ( 'NONE', #99504, 0.06509327318403745899 ) ;
#3348 = CARTESIAN_POINT ( 'NONE',  ( 4.599999999999936584, 12.50000000000000000, 3.637306695894644726 ) ) ;
#3349 = AXIS2_PLACEMENT_3D ( 'NONE', #98292, #89769, #78685 ) ;
#3350 = ORIENTED_EDGE ( 'NONE', *, *, #72062, .F. ) ;
#3351 = ORIENTED_EDGE ( 'NONE', *, *, #38316, .F. ) ;
#3352 = DIRECTION ( 'NONE',  ( 0.000000000000000000, 0.000000000000000000, 1.000000000000000000 ) ) ;
#3353 = CARTESIAN_POINT ( 'NONE',  ( -0.8500000000000382805, 2.500000000000000000, -1.472243186433550122 ) ) ;
#3354 = DIRECTION ( 'NONE',  ( 0.000000000000000000, 0.000000000000000000, 1.000000000000000000 ) ) ;
#3355 = FACE_OUTER_BOUND ( 'NONE', #62813, .T. ) ;
#3356 = CIRCLE ( 'NONE', #108096, 0.06509327318403745899 ) ;
#3357 = DIRECTION ( 'NONE',  ( -0.000000000000000000, 1.000000000000000000, -0.000000000000000000 ) ) ;
#3358 = EDGE_LOOP ( 'NONE', ( #37425, #31143, #33559, #129211 ) ) ;
#3359 = VERTEX_POINT ( 'NONE', #84444 ) ;
#3360 = CARTESIAN_POINT ( 'NONE',  ( -6.650000000000018119, 12.50000000000000000, -6.495190528383302464 ) ) ;
#3361 = CARTESIAN_POINT ( 'NONE',  ( 3.149999999999942624, 12.50000000000000000, 6.841600689897072485 ) ) ;
#3362 = DIRECTION ( 'NONE',  ( -0.000000000000000000, -1.000000000000000000, -0.000000000000000000 ) ) ;
#3363 = FACE_OUTER_BOUND ( 'NONE', #99898, .T. ) ;
#3364 = CARTESIAN_POINT ( 'NONE',  ( 175.5000000000000000, 0.000000000000000000, 0.000000000000000000 ) ) ;
#3365 = VERTEX_POINT ( 'NONE', #6483 ) ;
#3366 = DIRECTION ( 'NONE',  ( 0.000000000000000000, 0.000000000000000000, 1.000000000000000000 ) ) ;
#3367 = CONICAL_SURFACE ( 'NONE', #34780, 0.09999999999999982514, 0.003490658503988666988 ) ;
#3368 = FACE_OUTER_BOUND ( 'NONE', #92228, .T. ) ;
#3369 = ORIENTED_EDGE ( 'NONE', *, *, #104376, .T. ) ;
#3370 = CARTESIAN_POINT ( 'NONE',  ( 12.09999999999990195, 2.500000000000000000, -0.5928203230275541635 ) ) ;
#3371 = ORIENTED_EDGE ( 'NONE', *, *, #112669, .F. ) ;
#3372 = DIRECTION ( 'NONE',  ( 0.000000000000000000, 0.000000000000000000, 1.000000000000000000 ) ) ;
#3373 = ORIENTED_EDGE ( 'NONE', *, *, #128523, .T. ) ;
#3374 = DIRECTION ( 'NONE',  ( 0.000000000000000000, 1.000000000000000000, 0.000000000000000000 ) ) ;
#3375 = CARTESIAN_POINT ( 'NONE',  ( 8.099999999999923261, 2.500000000000000000, 4.676537180435972552 ) ) ;
#3376 = ORIENTED_EDGE ( 'NONE', *, *, #118536, .F. ) ;
#3377 = ORIENTED_EDGE ( 'NONE', *, *, #95198, .T. ) ;
#3378 = CARTESIAN_POINT ( 'NONE',  ( 185.1718750003414016, 9.264065473108010111E-16, -7.564683531250000925 ) ) ;
#3379 = DIRECTION ( 'NONE',  ( 0.000000000000000000, 0.000000000000000000, -1.000000000000000000 ) ) ;
#3380 = CARTESIAN_POINT ( 'NONE',  ( 186.4635416670080872, -4.367472073101520635, 7.564683531249999149 ) ) ;
#3381 = CARTESIAN_POINT ( 'NONE',  ( 184.4843750003414016, -8.734944146203032389, -1.604583208406767949E-15 ) ) ;
#3382 = EDGE_CURVE ( 'NONE', #68225, #79959, #32949, .T. ) ;
#3383 = AXIS2_PLACEMENT_3D ( 'NONE', #7151, #39241, #49693 ) ;
#3384 = DIRECTION ( 'NONE',  ( 0.000000000000000000, 1.000000000000000000, 0.000000000000000000 ) ) ;
#3385 = DIRECTION ( 'NONE',  ( 0.000000000000000000, 0.000000000000000000, -1.000000000000000000 ) ) ;
#3386 = EDGE_CURVE ( 'NONE', #127025, #98360, #116247, .T. ) ;
#3387 = CARTESIAN_POINT ( 'NONE',  ( 1.649999999999951505, 12.50000000000000000, 1.472243186433545459 ) ) ;
#3388 = CONICAL_SURFACE ( 'NONE', #57779, 0.1000000000000000472, 0.003490658503988666988 ) ;
#3389 = CARTESIAN_POINT ( 'NONE',  ( -9.600000000000008527, 2.500000000000000000, -0.1000000000000023925 ) ) ;
#3390 = AXIS2_PLACEMENT_3D ( 'NONE', #55704, #85802, #45254 ) ;
#3391 = AXIS2_PLACEMENT_3D ( 'NONE', #88541, #49939, #47994 ) ;
#3392 = EDGE_LOOP ( 'NONE', ( #67767, #117672 ) ) ;
#3393 = AXIS2_PLACEMENT_3D ( 'NONE', #23661, #63591, #103513 ) ;
#3394 = VERTEX_POINT ( 'NONE', #14393 ) ;
#3395 = DIRECTION ( 'NONE',  ( 0.000000000000000000, 0.000000000000000000, -1.000000000000000000 ) ) ;
#3396 = ORIENTED_EDGE ( 'NONE', *, *, #93946, .T. ) ;
#3397 = LINE ( 'NONE', #44614, #60100 ) ;
#3398 = DIRECTION ( 'NONE',  ( 0.000000000000000000, 0.000000000000000000, 1.000000000000000000 ) ) ;
#3399 = CARTESIAN_POINT ( 'NONE',  ( -6.249999999999981348, 12.50000000000000000, 2.099970236277060032 ) ) ;
#3401 = EDGE_LOOP ( 'NONE', ( #97852, #102026 ) ) ;
#3400 = VERTEX_POINT ( 'NONE', #105373 ) ;
#3402 = FACE_BOUND ( 'NONE', #64250, .T. ) ;
#3403 = ORIENTED_EDGE ( 'NONE', *, *, #97045, .T. ) ;
#3404 = DIRECTION ( 'NONE',  ( 0.000000000000000000, 0.000000000000000000, -1.000000000000000000 ) ) ;
#3405 = CARTESIAN_POINT ( 'NONE',  ( -8.150000000000014566, 2.500000000000000000, -6.148780366869520897 ) ) ;
#3406 = AXIS2_PLACEMENT_3D ( 'NONE', #54867, #94806, #86909 ) ;
#3407 = DIRECTION ( 'NONE',  ( -4.274815082592931898E-19, -0.9999939076577903929, -0.003490651415223739937 ) ) ;
#3408 = CARTESIAN_POINT ( 'NONE',  ( -3.350000000000032507, 12.50000000000000000, -6.560283801567339701 ) ) ;
#3409 = DIRECTION ( 'NONE',  ( -0.000000000000000000, 1.000000000000000000, -0.000000000000000000 ) ) ;
#3411 = VECTOR ( 'NONE', #65548, 1000.000000000000000 ) ;
#3410 = AXIS2_PLACEMENT_3D ( 'NONE', #12274, #63973, #4370 ) ;
#3412 = CARTESIAN_POINT ( 'NONE',  ( 9.599999999999914380, 2.500000000000000000, 4.230127018922196669 ) ) ;
#3413 = CARTESIAN_POINT ( 'NONE',  ( -2.499999999999996003, 2.500000000000000000, -4.330127018922201643 ) ) ;
#3414 = FACE_OUTER_BOUND ( 'NONE', #56837, .T. ) ;
#3415 = CARTESIAN_POINT ( 'NONE',  ( 10.39999999999990976, 12.50000000000000000, -4.330127018922201643 ) ) ;
#3416 = DIRECTION ( 'NONE',  ( 0.000000000000000000, 0.000000000000000000, 1.000000000000000000 ) ) ;
#3417 = CARTESIAN_POINT ( 'NONE',  ( -2.100000000000034728, 2.500000000000000000, 4.330127018922196314 ) ) ;
#3418 = ORIENTED_EDGE ( 'NONE', *, *, #79445, .T. ) ;
#3419 = ORIENTED_EDGE ( 'NONE', *, *, #16024, .F. ) ;
#3420 = ORIENTED_EDGE ( 'NONE', *, *, #31519, .T. ) ;
#3421 = CARTESIAN_POINT ( 'NONE',  ( -4.600000000000024514, 2.500000000000000000, 3.537306695894645081 ) ) ;
#3422 = ORIENTED_EDGE ( 'NONE', *, *, #86612, .T. ) ;
#3423 = LINE ( 'NONE', #23718, #56991 ) ;
#3425 = ORIENTED_EDGE ( 'NONE', *, *, #99659, .F. ) ;
#3424 = ORIENTED_EDGE ( 'NONE', *, *, #33121, .F. ) ;
#3426 = ORIENTED_EDGE ( 'NONE', *, *, #115420, .F. ) ;
#3427 = EDGE_CURVE ( 'NONE', #59532, #121105, #49385, .T. ) ;
#3428 = DIRECTION ( 'NONE',  ( 0.000000000000000000, 1.000000000000000000, 0.000000000000000000 ) ) ;
#3429 = EDGE_CURVE ( 'NONE', #67593, #79758, #78909, .T. ) ;
#3430 = DIRECTION ( 'NONE',  ( 0.000000000000000000, 1.000000000000000000, 0.000000000000000000 ) ) ;
#3431 = CARTESIAN_POINT ( 'NONE',  ( -10.85000000000000142, 2.500000000000000000, -1.472243186433546125 ) ) ;
#3432 = CARTESIAN_POINT ( 'NONE',  ( -10.85000000000000142, 2.500000000000000000, -7.188010851410850499 ) ) ;
#3433 = DIRECTION ( 'NONE',  ( -0.000000000000000000, 1.000000000000000000, -0.000000000000000000 ) ) ;
#3434 = EDGE_CURVE ( 'NONE', #17761, #23241, #124867, .T. ) ;
#3435 = VERTEX_POINT ( 'NONE', #93618 ) ;
#3436 = EDGE_CURVE ( 'NONE', #27815, #11046, #99831, .T. ) ;
#3437 = CARTESIAN_POINT ( 'NONE',  ( -13.09999999999999254, 12.50000000000000000, -4.048810130592460865 ) ) ;
#3438 = EDGE_LOOP ( 'NONE', ( #36438, #19297 ) ) ;
#3440 = EDGE_LOOP ( 'NONE', ( #39912, #43577, #78100, #124381 ) ) ;
#3439 = VECTOR ( 'NONE', #96293, 1000.000000000000000 ) ;
#3441 = ORIENTED_EDGE ( 'NONE', *, *, #101429, .F. ) ;
#3442 = AXIS2_PLACEMENT_3D ( 'NONE', #37941, #117763, #7176 ) ;
#3443 = EDGE_CURVE ( 'NONE', #45043, #117937, #4553, .T. ) ;
#3445 = EDGE_CURVE ( 'NONE', #83081, #46534, #122522, .T. ) ;
#3444 = FACE_OUTER_BOUND ( 'NONE', #77319, .T. ) ;
#3447 = ORIENTED_EDGE ( 'NONE', *, *, #3382, .F. ) ;
#3446 = ADVANCED_FACE ( 'NONE', ( #45816 ), #85718, .T. ) ;
#3448 = EDGE_LOOP ( 'NONE', ( #37278, #76317, #63856, #57143 ) ) ;
#3449 = EDGE_CURVE ( 'NONE', #127462, #21944, #87648, .T. ) ;
#3451 = EDGE_LOOP ( 'NONE', ( #102852, #27685 ) ) ;
#3450 = EDGE_CURVE ( 'NONE', #97893, #38892, #99550, .T. ) ;
#3452 = PRESENTATION_STYLE_ASSIGNMENT (( #104230 ) ) ;
#3453 = VECTOR ( 'NONE', #10303, 1000.000000000000000 ) ;
#3454 = CARTESIAN_POINT ( 'NONE',  ( 14.79999999999989413, 2.500000000000000000, -0.3464101615137782364 ) ) ;
#3455 = CARTESIAN_POINT ( 'NONE',  ( -3.950000000000025491, 12.50000000000000000, 6.148780366869520897 ) ) ;
#3456 = DIRECTION ( 'NONE',  ( -0.000000000000000000, -1.000000000000000000, -0.000000000000000000 ) ) ;
#3457 = DIRECTION ( 'NONE',  ( -4.274815082592931898E-19, -0.9999939076577903929, -0.003490651415223739937 ) ) ;
#3458 = CARTESIAN_POINT ( 'NONE',  ( 2.500000000000002220, 1.499999999999999334, 10.00000000000000178 ) ) ;
#3459 = EDGE_CURVE ( 'NONE', #43141, #22334, #5714, .T. ) ;
#3460 = PLANE ( 'NONE',  #124454 ) ;
#3462 = CIRCLE ( 'NONE', #105866, 0.09999999999999999167 ) ;
#3461 = AXIS2_PLACEMENT_3D ( 'NONE', #38769, #80604, #101528 ) ;
#3463 = ORIENTED_EDGE ( 'NONE', *, *, #1351, .T. ) ;
#3464 = CARTESIAN_POINT ( 'NONE',  ( -12.89999999999999147, 2.500000000000000000, -5.122947341949751987 ) ) ;
#3465 = AXIS2_PLACEMENT_3D ( 'NONE', #68798, #59659, #99562 ) ;
#3466 = ORIENTED_EDGE ( 'NONE', *, *, #104129, .F. ) ;
#3467 = CARTESIAN_POINT ( 'NONE',  ( 184.8333333333333144, 6.668395609140177704, -3.849999999999998312 ) ) ;
#3468 = ORIENTED_EDGE ( 'NONE', *, *, #15008, .T. ) ;
#3469 = VERTEX_POINT ( 'NONE', #127591 ) ;
#3470 = DIRECTION ( 'NONE',  ( 0.000000000000000000, -0.9999939076577903929, 0.003490651415223739937 ) ) ;
#3471 = FACE_OUTER_BOUND ( 'NONE', #18024, .T. ) ;
#3472 = DIRECTION ( 'NONE',  ( 0.000000000000000000, -0.9999939076577903929, 0.003490651415223739937 ) ) ;
#3473 = ORIENTED_EDGE ( 'NONE', *, *, #99194, .F. ) ;
#3474 = ORIENTED_EDGE ( 'NONE', *, *, #52438, .F. ) ;
#3475 = DIRECTION ( 'NONE',  ( 0.000000000000000000, 0.000000000000000000, 1.000000000000000000 ) ) ;
#3476 = DIRECTION ( 'NONE',  ( 0.000000000000000000, 1.000000000000000000, 0.000000000000000000 ) ) ;
#3477 = DIRECTION ( 'NONE',  ( -0.000000000000000000, -1.000000000000000000, -0.000000000000000000 ) ) ;
#3478 = CIRCLE ( 'NONE', #101687, 0.1000000000000000472 ) ;
#3479 = CARTESIAN_POINT ( 'NONE',  ( 0.1999999999999576006, 2.500000000000000000, -4.776537180435978414 ) ) ;
#3480 = AXIS2_PLACEMENT_3D ( 'NONE', #19845, #40123, #8698 ) ;
#3481 = DIRECTION ( 'NONE',  ( 0.000000000000000000, 1.000000000000000000, 0.000000000000000000 ) ) ;
#3482 = ORIENTED_EDGE ( 'NONE', *, *, #121427, .F. ) ;
#3483 = VECTOR ( 'NONE', #75617, 1000.000000000000000 ) ;
#3484 = DIRECTION ( 'NONE',  ( 0.000000000000000000, 0.000000000000000000, -1.000000000000000000 ) ) ;
#3485 = ADVANCED_FACE ( 'NONE', ( #116465 ), #45461, .T. ) ;
#3486 = EDGE_CURVE ( 'NONE', #39867, #75029, #66520, .T. ) ;
#3487 = AXIS2_PLACEMENT_3D ( 'NONE', #88045, #95324, #76972 ) ;
#3488 = EDGE_CURVE ( 'NONE', #1760, #96273, #24776, .T. ) ;
#3489 = ORIENTED_EDGE ( 'NONE', *, *, #86026, .F. ) ;
#3490 = CIRCLE ( 'NONE', #22379, 0.06509327318403745899 ) ;
#3491 = PLANE ( 'NONE',  #77873 ) ;
#3492 = CARTESIAN_POINT ( 'NONE',  ( -8.350000000000008527, 2.500000000000000000, 7.188010851410848723 ) ) ;
#3493 = AXIS2_PLACEMENT_3D ( 'NONE', #86272, #56807, #96740 ) ;
#3494 = EDGE_CURVE ( 'NONE', #24755, #48591, #64470, .T. ) ;
#3495 = CARTESIAN_POINT ( 'NONE',  ( 185.5052083336747444, -6.551208109652278289, 3.782341765624995134 ) ) ;
#3497 = VECTOR ( 'NONE', #55590, 1000.000000000000000 ) ;
#3496 = DIRECTION ( 'NONE',  ( 0.000000000000000000, -0.9999939076577903929, 0.003490651415223739937 ) ) ;
#3498 = DIRECTION ( 'NONE',  ( 0.000000000000000000, 1.000000000000000000, 0.000000000000000000 ) ) ;
#3499 = EDGE_CURVE ( 'NONE', #7675, #58472, #107946, .T. ) ;
#3500 = CARTESIAN_POINT ( 'NONE',  ( 5.449999999999937117, 2.500000000000000000, -6.495190528383302464 ) ) ;
#3501 = DIRECTION ( 'NONE',  ( 0.000000000000000000, 1.000000000000000000, 0.000000000000000000 ) ) ;
#3502 = ORIENTED_EDGE ( 'NONE', *, *, #121383, .F. ) ;
#3503 = CONICAL_SURFACE ( 'NONE', #22306, 0.1000000000000002554, 0.003490658503988666988 ) ;
#3504 = EDGE_CURVE ( 'NONE', #37160, #18098, #14287, .T. ) ;
#3505 = EDGE_CURVE ( 'NONE', #23967, #2289, #122975, .T. ) ;
#3506 = FACE_OUTER_BOUND ( 'NONE', #122936, .T. ) ;
#3509 = EDGE_CURVE ( 'NONE', #18231, #108081, #10100, .T. ) ;
#3508 = CIRCLE ( 'NONE', #51636, 0.06509327318403745899 ) ;
#3507 = CIRCLE ( 'NONE', #20233, 0.1000000000000002554 ) ;
#3510 = DIRECTION ( 'NONE',  ( 0.000000000000000000, 0.000000000000000000, 1.000000000000000000 ) ) ;
#3511 = DIRECTION ( 'NONE',  ( -0.000000000000000000, 1.000000000000000000, -0.000000000000000000 ) ) ;
#3512 = EDGE_LOOP ( 'NONE', ( #121905, #118922, #119382, #22083 ) ) ;
#3513 = EDGE_CURVE ( 'NONE', #67817, #57536, #39376, .T. ) ;
#3514 = CARTESIAN_POINT ( 'NONE',  ( -5.600000000000020073, 12.50000000000000000, 0.3464101615137736845 ) ) ;
#3515 = ORIENTED_EDGE ( 'NONE', *, *, #7885, .T. ) ;
#3516 = LINE ( 'NONE', #24444, #34309 ) ;
#3517 = ORIENTED_EDGE ( 'NONE', *, *, #98379, .T. ) ;
#3518 = CARTESIAN_POINT ( 'NONE',  ( 17.17161331426590820, -0.4678040054246333512, -5.513957101014161921 ) ) ;
#3519 = CARTESIAN_POINT ( 'NONE',  ( -8.749999999999975131, 2.500000000000000000, -2.065063509461102065 ) ) ;
#3520 = VECTOR ( 'NONE', #97276, 1000.000000000000000 ) ;
#3521 = DIRECTION ( 'NONE',  ( 1.000000000000000000, 0.000000000000000000, 0.000000000000000000 ) ) ;
#3522 = VERTEX_POINT ( 'NONE', #9749 ) ;
#3523 = FACE_OUTER_BOUND ( 'NONE', #122181, .T. ) ;
#3524 = CARTESIAN_POINT ( 'NONE',  ( -3.000000000000000000, 3.673940397442059868E-16, 6.000000000000005329 ) ) ;
#3525 = ADVANCED_FACE ( 'NONE', ( #128250 ), #67340, .T. ) ;
#3526 = ORIENTED_EDGE ( 'NONE', *, *, #20363, .F. ) ;
#3527 = VECTOR ( 'NONE', #69254, 1000.000000000000000 ) ;
#3528 = VERTEX_POINT ( 'NONE', #39874 ) ;
#3529 = AXIS2_PLACEMENT_3D ( 'NONE', #14265, #36984, #54210 ) ;
#3530 = ORIENTED_EDGE ( 'NONE', *, *, #60954, .T. ) ;
#3531 = CARTESIAN_POINT ( 'NONE',  ( 4.149999999999938183, 2.500000000000000000, 7.188010851410848723 ) ) ;
#3532 = DIRECTION ( 'NONE',  ( 0.000000000000000000, -0.000000000000000000, 1.000000000000000000 ) ) ;
#3533 = DIRECTION ( 'NONE',  ( 0.000000000000000000, 1.000000000000000000, 0.000000000000000000 ) ) ;
#3534 = ORIENTED_EDGE ( 'NONE', *, *, #22511, .T. ) ;
#3535 = CARTESIAN_POINT ( 'NONE',  ( -10.00000000000000533, 12.50000000000000000, 0.6928203230275494784 ) ) ;
#3536 = CYLINDRICAL_SURFACE ( 'NONE', #4210, 7.699999999999999289 ) ;
#3537 = EDGE_LOOP ( 'NONE', ( #83480, #102530 ) ) ;
#3539 = AXIS2_PLACEMENT_3D ( 'NONE', #112059, #32871, #120585 ) ;
#3538 = VECTOR ( 'NONE', #68697, 1000.000000000000000 ) ;
#3540 = DIRECTION ( 'NONE',  ( -0.000000000000000000, -1.000000000000000000, -0.000000000000000000 ) ) ;
#3541 = CARTESIAN_POINT ( 'NONE',  ( 12.49999999999990408, 2.500000000000000000, -3.637306695894650055 ) ) ;
#3542 = EDGE_CURVE ( 'NONE', #80322, #120641, #114641, .T. ) ;
#3543 = PLANE ( 'NONE',  #82141 ) ;
#3544 = DIRECTION ( 'NONE',  ( 0.000000000000000000, -0.000000000000000000, 1.000000000000000000 ) ) ;
#3545 = DIRECTION ( 'NONE',  ( 0.000000000000000000, 0.000000000000000000, 1.000000000000000000 ) ) ;
#3546 = CARTESIAN_POINT ( 'NONE',  ( 4.549999999999939426, 12.50000000000000000, -6.495190528383302464 ) ) ;
#3547 = CARTESIAN_POINT ( 'NONE',  ( 4.999999999999969802, 12.50000000000000000, 4.330127018922196314 ) ) ;
#3548 = CONICAL_SURFACE ( 'NONE', #18117, 0.09999999999999982514, 0.003490658503988666988 ) ;
#3549 = VECTOR ( 'NONE', #2247, 1000.000000000000000 ) ;
#3550 = ORIENTED_EDGE ( 'NONE', *, *, #28438, .T. ) ;
#3551 = ORIENTED_EDGE ( 'NONE', *, *, #59969, .T. ) ;
#3552 = ORIENTED_EDGE ( 'NONE', *, *, #80457, .F. ) ;
#3553 = ORIENTED_EDGE ( 'NONE', *, *, #8226, .F. ) ;
#3554 = LINE ( 'NONE', #4823, #108100 ) ;
#3555 = DIRECTION ( 'NONE',  ( 0.000000000000000000, -0.9999939076577903929, 0.003490651415223739937 ) ) ;
#3556 = CARTESIAN_POINT ( 'NONE',  ( 4.599999999999936584, 2.500000000000000000, 4.230127018922196669 ) ) ;
#3557 = ORIENTED_EDGE ( 'NONE', *, *, #95557, .T. ) ;
#3558 = EDGE_CURVE ( 'NONE', #127371, #111304, #79150, .T. ) ;
#3559 = FACE_BOUND ( 'NONE', #123016, .T. ) ;
#3560 = DIRECTION ( 'NONE',  ( -0.000000000000000000, 1.000000000000000000, -0.000000000000000000 ) ) ;
#3561 = FACE_OUTER_BOUND ( 'NONE', #121386, .T. ) ;
#3562 = CARTESIAN_POINT ( 'NONE',  ( 8.949999999999915801, 12.50000000000000000, -1.818653347947326138 ) ) ;
#3563 = DIRECTION ( 'NONE',  ( -0.000000000000000000, -1.000000000000000000, -0.000000000000000000 ) ) ;
#3564 = DIRECTION ( 'NONE',  ( 0.000000000000000000, 0.000000000000000000, -1.000000000000000000 ) ) ;
#3565 = DIRECTION ( 'NONE',  ( 0.000000000000000000, 1.000000000000000000, 0.000000000000000000 ) ) ;
#3566 = PLANE ( 'NONE',  #68491 ) ;
#3567 = CARTESIAN_POINT ( 'NONE',  ( -3.350000000000031619, 12.50000000000000000, -7.188010851410854052 ) ) ;
#3568 = CARTESIAN_POINT ( 'NONE',  ( -0.6000000000000383915, 2.500000000000000000, -4.776537180435977525 ) ) ;
#3569 = CONICAL_SURFACE ( 'NONE', #91304, 0.1000000000000002554, 0.003490658503988666988 ) ;
#3570 = AXIS2_PLACEMENT_3D ( 'NONE', #63472, #1315, #32740 ) ;
#3571 = VECTOR ( 'NONE', #20329, 1000.000000000000000 ) ;
#3572 = EDGE_LOOP ( 'NONE', ( #126726, #6009 ) ) ;
#3573 = ORIENTED_EDGE ( 'NONE', *, *, #18938, .F. ) ;
#3575 = VERTEX_POINT ( 'NONE', #48384 ) ;
#3574 = CONICAL_SURFACE ( 'NONE', #103929, 0.1000000000000002554, 0.003490658503988666988 ) ;
#3576 = ORIENTED_EDGE ( 'NONE', *, *, #104827, .T. ) ;
#3577 = ORIENTED_EDGE ( 'NONE', *, *, #75925, .F. ) ;
#3578 = ORIENTED_EDGE ( 'NONE', *, *, #74897, .F. ) ;
#3579 = DIRECTION ( 'NONE',  ( 0.000000000000000000, 0.000000000000000000, 1.000000000000000000 ) ) ;
#3580 = ORIENTED_EDGE ( 'NONE', *, *, #45192, .F. ) ;
#3582 = EDGE_LOOP ( 'NONE', ( #58539, #96317, #11080, #105455 ) ) ;
#3581 = CIRCLE ( 'NONE', #105986, 0.06509327318403745899 ) ;
#3583 = CIRCLE ( 'NONE', #112340, 0.1000000000000002554 ) ;
#3584 = CONICAL_SURFACE ( 'NONE', #53667, 0.1000000000000000472, 0.003490658503988666988 ) ;
#3585 = EDGE_CURVE ( 'NONE', #69257, #94819, #68675, .T. ) ;
#3586 = DIRECTION ( 'NONE',  ( 0.000000000000000000, 1.000000000000000000, 0.000000000000000000 ) ) ;
#3587 = CARTESIAN_POINT ( 'NONE',  ( -10.65000000000000391, 2.500000000000000000, -6.841600689897075149 ) ) ;
#3588 = AXIS2_PLACEMENT_3D ( 'NONE', #42405, #90849, #92793 ) ;
#3589 = EDGE_LOOP ( 'NONE', ( #73522, #101539, #87655, #12064 ) ) ;
#3590 = DIRECTION ( 'NONE',  ( -0.000000000000000000, -1.000000000000000000, -0.000000000000000000 ) ) ;
#3591 = ADVANCED_FACE ( 'NONE', ( #89600 ), #5872, .T. ) ;
#3592 = EDGE_LOOP ( 'NONE', ( #92258, #106785, #77770, #120453 ) ) ;
#3594 = CIRCLE ( 'NONE', #76758, 0.06509327318403741736 ) ;
#3593 = CIRCLE ( 'NONE', #95626, 0.1000000000000000472 ) ;
#3595 = ORIENTED_EDGE ( 'NONE', *, *, #42802, .T. ) ;
#3596 = DIRECTION ( 'NONE',  ( 1.000000000000000000, 0.000000000000000000, -0.000000000000000000 ) ) ;
#3597 = ADVANCED_FACE ( 'NONE', ( #109219 ), #129550, .T. ) ;
#3599 = EDGE_CURVE ( 'NONE', #33854, #88432, #70603, .T. ) ;
#3598 = CARTESIAN_POINT ( 'NONE',  ( -9.600000000000008527, 2.500000000000000000, -2.385244779468109755E-15 ) ) ;
#3600 = EDGE_CURVE ( 'NONE', #77153, #67249, #16332, .T. ) ;
#3601 = EDGE_CURVE ( 'NONE', #28402, #45029, #22171, .T. ) ;
#3602 = ORIENTED_EDGE ( 'NONE', *, *, #128653, .T. ) ;
#3603 = ORIENTED_EDGE ( 'NONE', *, *, #57412, .F. ) ;
#3604 = CARTESIAN_POINT ( 'NONE',  ( 11.44999999999990870, 12.50000000000000000, -1.818653347947326138 ) ) ;
#3605 = CARTESIAN_POINT ( 'NONE',  ( -13.29999999999999005, 2.500000000000000000, -4.330127018922198978 ) ) ;
#3606 = DIRECTION ( 'NONE',  ( 0.000000000000000000, 0.000000000000000000, 1.000000000000000000 ) ) ;
#3607 = DIRECTION ( 'NONE',  ( 0.000000000000000000, 1.000000000000000000, 0.000000000000000000 ) ) ;
#3608 = CARTESIAN_POINT ( 'NONE',  ( -8.350000000000013856, 2.500000000000000000, -5.802370205355744659 ) ) ;
#3610 = EDGE_CURVE ( 'NONE', #117538, #114610, #30045, .T. ) ;
#3609 = CIRCLE ( 'NONE', #124888, 0.06509327318403745899 ) ;
#3611 = EDGE_LOOP ( 'NONE', ( #86232, #86347 ) ) ;
#3612 = CARTESIAN_POINT ( 'NONE',  ( 11.69999999999990870, 12.50000000000000000, -4.265033745738164406 ) ) ;
#3613 = ADVANCED_FACE ( 'NONE', ( #80433 ), #8026, .T. ) ;
#3614 = ADVANCED_FACE ( 'NONE', ( #2486 ), #81213, .T. ) ;
#3615 = ORIENTED_EDGE ( 'NONE', *, *, #109543, .T. ) ;
#3616 = DIRECTION ( 'NONE',  ( 0.000000000000000000, 0.000000000000000000, 1.000000000000000000 ) ) ;
#3617 = VERTEX_POINT ( 'NONE', #12317 ) ;
#3618 = DIRECTION ( 'NONE',  ( 0.000000000000000000, -0.9999939076577903929, 0.003490651415223739937 ) ) ;
#3619 = CARTESIAN_POINT ( 'NONE',  ( 13.74999999999993072, 12.50000000000000000, -2.099970236277064473 ) ) ;
#3620 = DIRECTION ( 'NONE',  ( -4.274815082592931898E-19, -0.9999939076577903929, -0.003490651415223739937 ) ) ;
#3621 = CARTESIAN_POINT ( 'NONE',  ( 10.39999999999991331, 12.50000000000000000, -2.385244779468109755E-15 ) ) ;
#3622 = VERTEX_POINT ( 'NONE', #69965 ) ;
#3623 = DIRECTION ( 'NONE',  ( 0.000000000000000000, -0.000000000000000000, 1.000000000000000000 ) ) ;
#3624 = AXIS2_PLACEMENT_3D ( 'NONE', #119018, #91485, #110482 ) ;
#3625 = CARTESIAN_POINT ( 'NONE',  ( 1.249999999999953815, 12.50000000000000000, 1.472243186433545459 ) ) ;
#3626 = EDGE_LOOP ( 'NONE', ( #90392, #112551, #68546, #57210 ) ) ;
#3627 = VERTEX_POINT ( 'NONE', #90884 ) ;
#3628 = ORIENTED_EDGE ( 'NONE', *, *, #49397, .F. ) ;
#3629 = CARTESIAN_POINT ( 'NONE',  ( 14.54999999999989235, 2.500000000000000000, -2.165063509461101710 ) ) ;
#3630 = CARTESIAN_POINT ( 'NONE',  ( 12.89999999999989733, 12.50000000000000000, -0.06509327318403980434 ) ) ;
#3631 = CARTESIAN_POINT ( 'NONE',  ( 185.2760416670080588, 6.551208109652274736, 3.782341765625001351 ) ) ;
#3632 = CARTESIAN_POINT ( 'NONE',  ( -17.50000000000000000, 1.500000000000000000, 10.00000000000000178 ) ) ;
#3634 = CARTESIAN_POINT ( 'NONE',  ( 186.1666666666666856, -6.668395609140176816, -3.850000000000003642 ) ) ;
#3633 = AXIS2_PLACEMENT_3D ( 'NONE', #128285, #78547, #9780 ) ;
#3635 = CIRCLE ( 'NONE', #68468, 0.06509327318403745899 ) ;
#3636 = CARTESIAN_POINT ( 'NONE',  ( 12.29999999999990123, 2.500000000000000000, 0.3464101615137735735 ) ) ;
#3637 = CARTESIAN_POINT ( 'NONE',  ( 11.89999999999990798, 2.500000000000000000, -3.983716857408426293 ) ) ;
#3639 = AXIS2_PLACEMENT_3D ( 'NONE', #12384, #42518, #20925 ) ;
#3638 = VECTOR ( 'NONE', #125353, 1000.000000000000000 ) ;
#3640 = ORIENTED_EDGE ( 'NONE', *, *, #37311, .F. ) ;
#3641 = DIRECTION ( 'NONE',  ( 0.000000000000000000, 0.000000000000000000, 1.000000000000000000 ) ) ;
#3642 = CIRCLE ( 'NONE', #20376, 0.09999999999999982514 ) ;
#3643 = ORIENTED_EDGE ( 'NONE', *, *, #119168, .T. ) ;
#3644 = DIRECTION ( 'NONE',  ( 0.000000000000000000, 0.000000000000000000, 1.000000000000000000 ) ) ;
#3645 = CARTESIAN_POINT ( 'NONE',  ( 12.49999999999990408, 12.50000000000000000, -3.702399969078687292 ) ) ;
#3646 = CARTESIAN_POINT ( 'NONE',  ( 13.74999999999989342, 2.500000000000000000, -1.472243186433550122 ) ) ;
#3647 = EDGE_CURVE ( 'NONE', #73941, #33867, #37300, .T. ) ;
#3648 = CARTESIAN_POINT ( 'NONE',  ( 6.449999999999930012, 2.500000000000000000, 1.718653347947321386 ) ) ;
#3649 = ORIENTED_EDGE ( 'NONE', *, *, #122494, .T. ) ;
#3650 = EDGE_CURVE ( 'NONE', #80364, #85528, #76997, .T. ) ;
#3651 = ADVANCED_FACE ( 'NONE', ( #109887 ), #41519, .T. ) ;
#3652 = CARTESIAN_POINT ( 'NONE',  ( 14.99999999999989164, 2.500000000000000000, 0.5928203230275495006 ) ) ;
#3654 = EDGE_LOOP ( 'NONE', ( #31160, #87146, #118674, #110661 ) ) ;
#3653 = CARTESIAN_POINT ( 'NONE',  ( 12.49999999999993605, 2.500000000000000000, -0.1000000000000022815 ) ) ;
#3655 = VECTOR ( 'NONE', #11620, 1000.000000000000000 ) ;
#3656 = AXIS2_PLACEMENT_3D ( 'NONE', #34358, #114819, #71191 ) ;
#3657 = VERTEX_POINT ( 'NONE', #60785 ) ;
#3658 = EDGE_CURVE ( 'NONE', #18238, #102257, #20570, .T. ) ;
#3659 = CARTESIAN_POINT ( 'NONE',  ( 1.249999999999953815, 2.500000000000000000, 1.472243186433545459 ) ) ;
#3660 = AXIS2_PLACEMENT_3D ( 'NONE', #23948, #16670, #96522 ) ;
#3661 = EDGE_LOOP ( 'NONE', ( #104647, #108613 ) ) ;
#3662 = VERTEX_POINT ( 'NONE', #120992 ) ;
#3663 = DIRECTION ( 'NONE',  ( 0.000000000000000000, 0.000000000000000000, -1.000000000000000000 ) ) ;
#3664 = AXIS2_PLACEMENT_3D ( 'NONE', #73580, #21935, #12092 ) ;
#3665 = ORIENTED_EDGE ( 'NONE', *, *, #128331, .T. ) ;
#3666 = CARTESIAN_POINT ( 'NONE',  ( 17.84432265422998043, 2.533187527836770148, -5.021315468708433372 ) ) ;
#3667 = CARTESIAN_POINT ( 'NONE',  ( 105.6184301395928031, 8.500000000000000000, -1.375000000000000888 ) ) ;
#3668 = AXIS2_PLACEMENT_3D ( 'NONE', #67791, #19998, #59938 ) ;
#3669 = DIRECTION ( 'NONE',  ( 0.000000000000000000, 1.000000000000000000, 0.000000000000000000 ) ) ;
#3670 = EDGE_LOOP ( 'NONE', ( #4354, #86300, #85356, #6712 ) ) ;
#3671 = CIRCLE ( 'NONE', #53857, 0.1000000000000000472 ) ;
#3672 = CARTESIAN_POINT ( 'NONE',  ( -11.25000000000000178, 2.500000000000000000, -1.472243186433546125 ) ) ;
#3674 = ORIENTED_EDGE ( 'NONE', *, *, #120514, .T. ) ;
#3673 = CARTESIAN_POINT ( 'NONE',  ( 12.89999999999990088, 2.500000000000000000, -4.430127018922202176 ) ) ;
#3675 = CARTESIAN_POINT ( 'NONE',  ( 179.5000000000000000, 0.6250000000000000000, 7.634788798650556707 ) ) ;
#3676 = CIRCLE ( 'NONE', #106086, 0.1000000000000000472 ) ;
#3677 = CARTESIAN_POINT ( 'NONE',  ( 17.34778429999909122, -2.317753570193370027, 4.873671836816545699 ) ) ;
#3678 = EDGE_CURVE ( 'NONE', #17419, #41508, #122294, .T. ) ;
#3679 = VERTEX_POINT ( 'NONE', #1212 ) ;
#3680 = ORIENTED_EDGE ( 'NONE', *, *, #111499, .T. ) ;
#3681 = VERTEX_POINT ( 'NONE', #31980 ) ;
#3682 = ORIENTED_EDGE ( 'NONE', *, *, #103804, .F. ) ;
#3683 = CARTESIAN_POINT ( 'NONE',  ( -13.29999999999999005, 2.500000000000000000, 0.1000000000000018513 ) ) ;
#3684 = DIRECTION ( 'NONE',  ( -0.000000000000000000, -1.000000000000000000, -0.000000000000000000 ) ) ;
#3685 = CARTESIAN_POINT ( 'NONE',  ( -8.100000000000013856, 12.50000000000000000, -4.676537180435977881 ) ) ;
#3686 = FACE_BOUND ( 'NONE', #27157, .T. ) ;
#3687 = ORIENTED_EDGE ( 'NONE', *, *, #24270, .F. ) ;
#3688 = CARTESIAN_POINT ( 'NONE',  ( 184.4062500006828316, -8.891194145520236347, -1.633285867636356693E-15 ) ) ;
#3689 = CARTESIAN_POINT ( 'NONE',  ( -7.499999999999976907, 2.500000000000000000, 4.330127018922196314 ) ) ;
#3690 = LINE ( 'NONE', #124105, #43775 ) ;
#3691 = EDGE_CURVE ( 'NONE', #91731, #88053, #12949, .T. ) ;
#3692 = FACE_OUTER_BOUND ( 'NONE', #84321, .T. ) ;
#3693 = CARTESIAN_POINT ( 'NONE',  ( 13.34999999999990017, 2.500000000000000000, 1.372243186433545370 ) ) ;
#3694 = CIRCLE ( 'NONE', #76867, 0.06509327318403745899 ) ;
#3695 = DIRECTION ( 'NONE',  ( -0.000000000000000000, -1.000000000000000000, -0.000000000000000000 ) ) ;
#3696 = CARTESIAN_POINT ( 'NONE',  ( 8.749999999999918288, 2.500000000000000000, 7.188010851410848723 ) ) ;
#3697 = ORIENTED_EDGE ( 'NONE', *, *, #53423, .F. ) ;
#3698 = ORIENTED_EDGE ( 'NONE', *, *, #124964, .T. ) ;
#3699 = EDGE_LOOP ( 'NONE', ( #11441, #94975, #65024, #118324 ) ) ;
#3700 = EDGE_LOOP ( 'NONE', ( #99315, #7947, #516, #125987 ) ) ;
#3701 = ORIENTED_EDGE ( 'NONE', *, *, #2633, .F. ) ;
#3702 = CARTESIAN_POINT ( 'NONE',  ( -4.350000000000023626, 2.500000000000000000, -2.411473670974877859 ) ) ;
#3703 = CARTESIAN_POINT ( 'NONE',  ( -1.700000000000035261, 2.500000000000000000, 4.330127018922196314 ) ) ;
#3704 = ORIENTED_EDGE ( 'NONE', *, *, #13493, .T. ) ;
#3705 = ADVANCED_FACE ( 'NONE', ( #91533 ), #71236, .T. ) ;
#3706 = FACE_BOUND ( 'NONE', #49713, .T. ) ;
#3707 = CARTESIAN_POINT ( 'NONE',  ( -10.40000000000000213, 12.50000000000000000, 0.6928203230275494784 ) ) ;
#3708 = CIRCLE ( 'NONE', #37084, 0.1000000000000002554 ) ;
#3709 = CIRCLE ( 'NONE', #41386, 0.06509327318403745899 ) ;
#3710 = EDGE_LOOP ( 'NONE', ( #1834, #128726 ) ) ;
#3711 = FACE_OUTER_BOUND ( 'NONE', #44079, .T. ) ;
#3712 = EDGE_CURVE ( 'NONE', #111704, #110043, #22812, .T. ) ;
#3713 = CARTESIAN_POINT ( 'NONE',  ( 13.74999999999993427, 2.500000000000000000, 2.065063509461097624 ) ) ;
#3714 = CARTESIAN_POINT ( 'NONE',  ( -3.150000000000029221, 12.50000000000000000, 2.511473670974873507 ) ) ;
#3715 = ORIENTED_EDGE ( 'NONE', *, *, #67545, .F. ) ;
#3716 = FACE_OUTER_BOUND ( 'NONE', #51286, .T. ) ;
#3717 = CONICAL_SURFACE ( 'NONE', #127071, 0.09999999999999982514, 0.003490658503988666988 ) ;
#3718 = ORIENTED_EDGE ( 'NONE', *, *, #81749, .T. ) ;
#3719 = CIRCLE ( 'NONE', #64358, 0.09999999999999982514 ) ;
#3720 = AXIS2_PLACEMENT_3D ( 'NONE', #118679, #117360, #8078 ) ;
#3721 = EDGE_LOOP ( 'NONE', ( #14930, #97877, #94219, #80001 ) ) ;
#3722 = ORIENTED_EDGE ( 'NONE', *, *, #66414, .F. ) ;
#3723 = LINE ( 'NONE', #33829, #25467 ) ;
#3724 = FACE_OUTER_BOUND ( 'NONE', #67466, .T. ) ;
#3725 = DIRECTION ( 'NONE',  ( 0.000000000000000000, 0.000000000000000000, -1.000000000000000000 ) ) ;
#3726 = ORIENTED_EDGE ( 'NONE', *, *, #79808, .F. ) ;
#3727 = CARTESIAN_POINT ( 'NONE',  ( 4.999999999999935163, 2.500000000000000000, 3.637306695894644726 ) ) ;
#3728 = AXIS2_PLACEMENT_3D ( 'NONE', #121084, #90313, #32081 ) ;
#3729 = LINE ( 'NONE', #73124, #94928 ) ;
#3730 = ADVANCED_FACE ( 'NONE', ( #71904 ), #82373, .T. ) ;
#3731 = DIRECTION ( 'NONE',  ( 0.000000000000000000, 0.000000000000000000, 1.000000000000000000 ) ) ;
#3732 = CARTESIAN_POINT ( 'NONE',  ( 187.2812500006828031, 0.000000000000000000, 7.700000000000000178 ) ) ;
#3733 = ORIENTED_EDGE ( 'NONE', *, *, #54546, .F. ) ;
#3734 = CONICAL_SURFACE ( 'NONE', #118655, 0.1000000000000000472, 0.003490658503988666988 ) ;
#3735 = DIRECTION ( 'NONE',  ( 0.000000000000000000, 0.000000000000000000, 1.000000000000000000 ) ) ;
#3736 = ORIENTED_EDGE ( 'NONE', *, *, #125313, .T. ) ;
#3737 = DIRECTION ( 'NONE',  ( 0.000000000000000000, 0.000000000000000000, 1.000000000000000000 ) ) ;
#3738 = EDGE_CURVE ( 'NONE', #19521, #87479, #72551, .T. ) ;
#3739 = AXIS2_PLACEMENT_3D ( 'NONE', #21719, #29598, #69513 ) ;
#3740 = ORIENTED_EDGE ( 'NONE', *, *, #99667, .F. ) ;
#3741 = VERTEX_POINT ( 'NONE', #15529 ) ;
#3742 = CARTESIAN_POINT ( 'NONE',  ( 5.449999999999936229, 12.50000000000000000, -2.165063509461101710 ) ) ;
#3743 = CIRCLE ( 'NONE', #28896, 0.09999999999999999167 ) ;
#3744 = DIRECTION ( 'NONE',  ( -0.000000000000000000, 1.000000000000000000, -0.000000000000000000 ) ) ;
#3745 = ADVANCED_FACE ( 'NONE', ( #104567 ), #51972, .T. ) ;
#3746 = DIRECTION ( 'NONE',  ( 0.000000000000000000, -0.000000000000000000, 1.000000000000000000 ) ) ;
#3748 = EDGE_CURVE ( 'NONE', #87862, #69423, #122934, .T. ) ;
#3747 = DIRECTION ( 'NONE',  ( -0.000000000000000000, 1.000000000000000000, -0.000000000000000000 ) ) ;
#3749 = ADVANCED_FACE ( 'NONE', ( #85573 ), #33279, .F. ) ;
#3751 = AXIS2_PLACEMENT_3D ( 'NONE', #118047, #78143, #26462 ) ;
#3750 = CARTESIAN_POINT ( 'NONE',  ( 106.0514428414850272, 8.500000000000000000, -1.125000000000000222 ) ) ;
#3752 = ADVANCED_FACE ( 'NONE', ( #45663 ), #103932, .T. ) ;
#3753 = VERTEX_POINT ( 'NONE', #43105 ) ;
#3754 = ORIENTED_EDGE ( 'NONE', *, *, #119805, .T. ) ;
#3755 = CARTESIAN_POINT ( 'NONE',  ( -12.94999999999999218, 2.500000000000000000, 2.265063509461101354 ) ) ;
#3756 = CIRCLE ( 'NONE', #16249, 0.09999999999999982514 ) ;
#3757 = CARTESIAN_POINT ( 'NONE',  ( -14.14999999999998614, 2.500000000000000000, 1.372243186433549367 ) ) ;
#3758 = EDGE_CURVE ( 'NONE', #8949, #106738, #56052, .T. ) ;
#3759 = CARTESIAN_POINT ( 'NONE',  ( -12.09999999999999609, 12.50000000000000000, -4.957854068765714217 ) ) ;
#3760 = ORIENTED_EDGE ( 'NONE', *, *, #90054, .F. ) ;
#3761 = EDGE_LOOP ( 'NONE', ( #59190, #119473, #24482, #32735 ) ) ;
#3762 = EDGE_CURVE ( 'NONE', #92740, #119776, #93726, .T. ) ;
#3763 = DIRECTION ( 'NONE',  ( 0.000000000000000000, 0.000000000000000000, 1.000000000000000000 ) ) ;
#3764 = AXIS2_PLACEMENT_3D ( 'NONE', #90489, #1469, #108842 ) ;
#3765 = VERTEX_POINT ( 'NONE', #114380 ) ;
#3766 = DIRECTION ( 'NONE',  ( 0.000000000000000000, 0.000000000000000000, 1.000000000000000000 ) ) ;
#3767 = EDGE_CURVE ( 'NONE', #110204, #88926, #129260, .T. ) ;
#3768 = CIRCLE ( 'NONE', #112447, 0.1000000000000000472 ) ;
#3769 = ADVANCED_FACE ( 'NONE', ( #3794 ), #79166, .T. ) ;
#3770 = CARTESIAN_POINT ( 'NONE',  ( -12.89999999999999147, 2.500000000000000000, 5.022947341949748790 ) ) ;
#3771 = ORIENTED_EDGE ( 'NONE', *, *, #91696, .T. ) ;
#3772 = DIRECTION ( 'NONE',  ( 0.000000000000000000, 0.000000000000000000, -1.000000000000000000 ) ) ;
#3773 = DIRECTION ( 'NONE',  ( 0.000000000000000000, 0.000000000000000000, -1.000000000000000000 ) ) ;
#3774 = DIRECTION ( 'NONE',  ( -0.000000000000000000, -1.000000000000000000, -0.000000000000000000 ) ) ;
#3775 = CIRCLE ( 'NONE', #120754, 0.09999999999999982514 ) ;
#3776 = ADVANCED_FACE ( 'NONE', ( #73813 ), #129350, .T. ) ;
#3778 = EDGE_CURVE ( 'NONE', #77998, #16575, #75115, .T. ) ;
#3777 = DIRECTION ( 'NONE',  ( 0.000000000000000000, 0.000000000000000000, -1.000000000000000000 ) ) ;
#3779 = ORIENTED_EDGE ( 'NONE', *, *, #70904, .F. ) ;
#3780 = LINE ( 'NONE', #52883, #15250 ) ;
#3782 = AXIS2_PLACEMENT_3D ( 'NONE', #3353, #13148, #84495 ) ;
#3781 = CIRCLE ( 'NONE', #91605, 0.06509327318403741736 ) ;
#3783 = CARTESIAN_POINT ( 'NONE',  ( 87.50000000000001421, -3.974992050023846257, 6.359987280038161828 ) ) ;
#3784 = ORIENTED_EDGE ( 'NONE', *, *, #101609, .F. ) ;
#3785 = ORIENTED_EDGE ( 'NONE', *, *, #45553, .F. ) ;
#3786 = CARTESIAN_POINT ( 'NONE',  ( 186.0052083336747444, -6.551208109652278289, 3.782341765624995134 ) ) ;
#3787 = DIRECTION ( 'NONE',  ( 0.000000000000000000, 0.000000000000000000, -1.000000000000000000 ) ) ;
#3788 = DIRECTION ( 'NONE',  ( 0.000000000000000000, 0.000000000000000000, -1.000000000000000000 ) ) ;
#3789 = DIRECTION ( 'NONE',  ( -0.000000000000000000, -1.000000000000000000, -0.000000000000000000 ) ) ;
#3790 = LINE ( 'NONE', #52252, #2527 ) ;
#3791 = DIRECTION ( 'NONE',  ( -4.274815082592931898E-19, -0.9999939076577903929, -0.003490651415223739937 ) ) ;
#3792 = CARTESIAN_POINT ( 'NONE',  ( -0.6500000000000398792, 2.500000000000000000, -6.841600689897078702 ) ) ;
#3793 = CARTESIAN_POINT ( 'NONE',  ( 5.449999999999934452, 2.500000000000000000, 2.165063509461097713 ) ) ;
#3794 = FACE_OUTER_BOUND ( 'NONE', #102990, .T. ) ;
#3795 = FACE_OUTER_BOUND ( 'NONE', #13437, .T. ) ;
#3796 = DIRECTION ( 'NONE',  ( 0.000000000000000000, 1.000000000000000000, 0.000000000000000000 ) ) ;
#3797 = ORIENTED_EDGE ( 'NONE', *, *, #63918, .F. ) ;
#3798 = VERTEX_POINT ( 'NONE', #95397 ) ;
#3799 = ORIENTED_EDGE ( 'NONE', *, *, #41172, .T. ) ;
#3800 = AXIS2_PLACEMENT_3D ( 'NONE', #89704, #39971, #122400 ) ;
#3801 = AXIS2_PLACEMENT_3D ( 'NONE', #92100, #3097, #50910 ) ;
#3802 = ORIENTED_EDGE ( 'NONE', *, *, #74124, .F. ) ;
#3803 = CARTESIAN_POINT ( 'NONE',  ( -13.74999999999998934, 12.50000000000000000, 2.857883832488652853 ) ) ;
#3804 = DIRECTION ( 'NONE',  ( 0.000000000000000000, 0.000000000000000000, 1.000000000000000000 ) ) ;
#3805 = EDGE_LOOP ( 'NONE', ( #88306, #97818 ) ) ;
#3806 = AXIS2_PLACEMENT_3D ( 'NONE', #44021, #74125, #76049 ) ;
#3807 = DIRECTION ( 'NONE',  ( 0.000000000000000000, 0.000000000000000000, -1.000000000000000000 ) ) ;
#3808 = EDGE_CURVE ( 'NONE', #948, #47249, #39464, .T. ) ;
#3809 = EDGE_CURVE ( 'NONE', #49723, #50793, #53548, .T. ) ;
#3810 = DIRECTION ( 'NONE',  ( -0.000000000000000000, -1.000000000000000000, -0.000000000000000000 ) ) ;
#3812 = ORIENTED_EDGE ( 'NONE', *, *, #27823, .T. ) ;
#3811 = PLANE ( 'NONE',  #51676 ) ;
#3813 = CARTESIAN_POINT ( 'NONE',  ( -9.400000000000009237, 12.50000000000000000, -4.048810130592459089 ) ) ;
#3814 = AXIS2_PLACEMENT_3D ( 'NONE', #77719, #67233, #39773 ) ;
#3815 = CYLINDRICAL_SURFACE ( 'NONE', #8172, 7.700000000000000178 ) ;
#3816 = ORIENTED_EDGE ( 'NONE', *, *, #65092, .F. ) ;
#3817 = CIRCLE ( 'NONE', #110424, 0.1000000000000002554 ) ;
#3818 = ORIENTED_EDGE ( 'NONE', *, *, #108538, .T. ) ;
#3819 = ORIENTED_EDGE ( 'NONE', *, *, #38635, .F. ) ;
#3820 = ORIENTED_EDGE ( 'NONE', *, *, #112260, .F. ) ;
#3821 = DIRECTION ( 'NONE',  ( 0.000000000000000000, -0.9999939076577903929, 0.003490651415223739937 ) ) ;
#3822 = DIRECTION ( 'NONE',  ( 0.000000000000000000, 0.000000000000000000, -1.000000000000000000 ) ) ;
#3823 = DIRECTION ( 'NONE',  ( -4.274815082592931898E-19, -0.9999939076577903929, -0.003490651415223739937 ) ) ;
#3824 = DIRECTION ( 'NONE',  ( 0.000000000000000000, 0.000000000000000000, 1.000000000000000000 ) ) ;
#3825 = CIRCLE ( 'NONE', #16322, 0.09999999999999982514 ) ;
#3826 = ORIENTED_EDGE ( 'NONE', *, *, #27112, .F. ) ;
#3827 = CARTESIAN_POINT ( 'NONE',  ( 13.74999999999989342, 2.500000000000000000, -1.372243186433550033 ) ) ;
#3828 = ORIENTED_EDGE ( 'NONE', *, *, #65772, .F. ) ;
#3829 = VECTOR ( 'NONE', #31652, 1000.000000000000000 ) ;
#3830 = DIRECTION ( 'NONE',  ( -1.224646799147352221E-16, 0.000000000000000000, -1.000000000000000000 ) ) ;
#3831 = CARTESIAN_POINT ( 'NONE',  ( -2.100000000000034284, 12.50000000000000000, -4.265033745738164406 ) ) ;
#3832 = DIRECTION ( 'NONE',  ( 0.000000000000000000, 0.000000000000000000, 1.000000000000000000 ) ) ;
#3833 = DIRECTION ( 'NONE',  ( 0.000000000000000000, 0.000000000000000000, -1.000000000000000000 ) ) ;
#3834 = EDGE_LOOP ( 'NONE', ( #21102, #73586 ) ) ;
#3835 = AXIS2_PLACEMENT_3D ( 'NONE', #110524, #30698, #20857 ) ;
#3836 = ORIENTED_EDGE ( 'NONE', *, *, #495, .T. ) ;
#3837 = VERTEX_POINT ( 'NONE', #33900 ) ;
#3838 = DIRECTION ( 'NONE',  ( 0.000000000000000000, 0.000000000000000000, 1.000000000000000000 ) ) ;
#3839 = DIRECTION ( 'NONE',  ( 0.000000000000000000, 1.000000000000000000, 0.000000000000000000 ) ) ;
#3840 = CARTESIAN_POINT ( 'NONE',  ( 5.199999999999933564, 2.500000000000000000, 3.883716857408420431 ) ) ;
#3841 = FACE_BOUND ( 'NONE', #38528, .T. ) ;
#3842 = DIRECTION ( 'NONE',  ( -0.000000000000000000, 1.000000000000000000, -0.000000000000000000 ) ) ;
#3843 = FACE_OUTER_BOUND ( 'NONE', #17918, .T. ) ;
#3844 = VECTOR ( 'NONE', #11494, 1000.000000000000000 ) ;
#3845 = DIRECTION ( 'NONE',  ( 0.000000000000000000, 1.000000000000000000, 0.000000000000000000 ) ) ;
#3846 = EDGE_CURVE ( 'NONE', #89337, #99110, #33198, .T. ) ;
#3847 = AXIS2_PLACEMENT_3D ( 'NONE', #81887, #102204, #61635 ) ;
#3848 = PLANE ( 'NONE',  #86042 ) ;
#3849 = DIRECTION ( 'NONE',  ( 0.000000000000000000, 0.000000000000000000, 1.000000000000000000 ) ) ;
#3850 = CIRCLE ( 'NONE', #77014, 0.06509327318403745899 ) ;
#3851 = DIRECTION ( 'NONE',  ( -0.000000000000000000, -1.000000000000000000, -0.000000000000000000 ) ) ;
#3852 = EDGE_LOOP ( 'NONE', ( #13495, #15911 ) ) ;
#3853 = FACE_OUTER_BOUND ( 'NONE', #7082, .T. ) ;
#3854 = VERTEX_POINT ( 'NONE', #14241 ) ;
#3855 = VERTEX_POINT ( 'NONE', #54192 ) ;
#3856 = ORIENTED_EDGE ( 'NONE', *, *, #12301, .T. ) ;
#3857 = ORIENTED_EDGE ( 'NONE', *, *, #115140, .T. ) ;
#3858 = EDGE_CURVE ( 'NONE', #129477, #96927, #124932, .T. ) ;
#3859 = CIRCLE ( 'NONE', #79093, 0.06509327318403745899 ) ;
#3861 = EDGE_CURVE ( 'NONE', #39180, #29091, #50734, .T. ) ;
#3860 = CARTESIAN_POINT ( 'NONE',  ( 6.049999999999932321, 12.50000000000000000, 1.818653347947321475 ) ) ;
#3862 = FACE_BOUND ( 'NONE', #66098, .T. ) ;
#3863 = CARTESIAN_POINT ( 'NONE',  ( -8.750000000000010658, 12.50000000000000000, -1.472243186433550122 ) ) ;
#3865 = AXIS2_PLACEMENT_3D ( 'NONE', #54842, #113130, #3824 ) ;
#3864 = CIRCLE ( 'NONE', #6001, 0.1000000000000002554 ) ;
#3866 = EDGE_LOOP ( 'NONE', ( #80262, #68192, #74858, #27927 ) ) ;
#3867 = CARTESIAN_POINT ( 'NONE',  ( -10.40000000000000213, 12.50000000000000000, 5.022947341949748790 ) ) ;
#3868 = EDGE_CURVE ( 'NONE', #40568, #79650, #11451, .T. ) ;
#3869 = DIRECTION ( 'NONE',  ( 0.000000000000000000, 1.000000000000000000, 0.000000000000000000 ) ) ;
#3870 = ORIENTED_EDGE ( 'NONE', *, *, #80627, .T. ) ;
#3871 = FACE_OUTER_BOUND ( 'NONE', #119901, .T. ) ;
#3872 = DIRECTION ( 'NONE',  ( 0.000000000000000000, 0.000000000000000000, -1.000000000000000000 ) ) ;
#3873 = EDGE_LOOP ( 'NONE', ( #36112, #11181, #64218, #103097 ) ) ;
#3874 = VECTOR ( 'NONE', #31558, 1000.000000000000000 ) ;
#3875 = CARTESIAN_POINT ( 'NONE',  ( -13.74999999999998757, 2.500000000000000000, 1.472243186433549456 ) ) ;
#3876 = CARTESIAN_POINT ( 'NONE',  ( 8.549999999999924327, 12.50000000000000000, 1.883746621131358934 ) ) ;
#3877 = ORIENTED_EDGE ( 'NONE', *, *, #112479, .F. ) ;
#3878 = CIRCLE ( 'NONE', #62396, 0.1000000000000000472 ) ;
#3879 = FACE_OUTER_BOUND ( 'NONE', #50222, .T. ) ;
#3880 = CIRCLE ( 'NONE', #6023, 0.5000000000000004441 ) ;
#3881 = CARTESIAN_POINT ( 'NONE',  ( 127.5000000000000000, 2.000000000000000000, -1.999999999999998224 ) ) ;
#3882 = AXIS2_PLACEMENT_3D ( 'NONE', #124833, #73784, #33860 ) ;
#3883 = DIRECTION ( 'NONE',  ( 0.000000000000000000, -0.9999939076577903929, 0.003490651415223739937 ) ) ;
#3884 = ORIENTED_EDGE ( 'NONE', *, *, #43676, .T. ) ;
#3885 = EDGE_LOOP ( 'NONE', ( #5495, #46002 ) ) ;
#3886 = FACE_OUTER_BOUND ( 'NONE', #124097, .T. ) ;
#3888 = ORIENTED_EDGE ( 'NONE', *, *, #106009, .T. ) ;
#3887 = AXIS2_PLACEMENT_3D ( 'NONE', #58649, #77618, #67808 ) ;
#3889 = PLANE ( 'NONE',  #42915 ) ;
#3890 = CARTESIAN_POINT ( 'NONE',  ( 10.79999999999991367, 12.50000000000000000, -2.385244779468109755E-15 ) ) ;
#3891 = EDGE_CURVE ( 'NONE', #108508, #7948, #21937, .T. ) ;
#3892 = VERTEX_POINT ( 'NONE', #110299 ) ;
#3893 = CIRCLE ( 'NONE', #100055, 0.1000000000000000472 ) ;
#3894 = CARTESIAN_POINT ( 'NONE',  ( 0.8499999999999536815, 2.500000000000000000, 6.395190528383296602 ) ) ;
#3895 = CARTESIAN_POINT ( 'NONE',  ( 6.899999999999928413, 12.50000000000000000, 4.741630453620009789 ) ) ;
#3896 = CARTESIAN_POINT ( 'NONE',  ( -3.350000000000029399, 12.50000000000000000, 6.495190528383297135 ) ) ;
#3897 = LINE ( 'NONE', #14979, #96754 ) ;
#3898 = ADVANCED_FACE ( 'NONE', ( #81490 ), #101127, .T. ) ;
#3899 = DIRECTION ( 'NONE',  ( -0.000000000000000000, -1.000000000000000000, -0.000000000000000000 ) ) ;
#3901 = EDGE_CURVE ( 'NONE', #18217, #5550, #32418, .T. ) ;
#3900 = CONICAL_SURFACE ( 'NONE', #77068, 0.1000000000000002554, 0.003490658503988666988 ) ;
#3902 = VERTEX_POINT ( 'NONE', #43514 ) ;
#3904 = ORIENTED_EDGE ( 'NONE', *, *, #36602, .F. ) ;
#3903 = VECTOR ( 'NONE', #107310, 1000.000000000000000 ) ;
#3905 = DIRECTION ( 'NONE',  ( -0.000000000000000000, -1.000000000000000000, -0.000000000000000000 ) ) ;
#3906 = CARTESIAN_POINT ( 'NONE',  ( -8.950000000000009948, 2.500000000000000000, -6.941600689897073018 ) ) ;
#3907 = ADVANCED_FACE ( 'NONE', ( #22592 ), #3566, .T. ) ;
#3909 = ORIENTED_EDGE ( 'NONE', *, *, #54295, .F. ) ;
#3908 = ORIENTED_EDGE ( 'NONE', *, *, #129083, .F. ) ;
#3910 = EDGE_CURVE ( 'NONE', #14174, #79060, #82793, .T. ) ;
#3911 = ORIENTED_EDGE ( 'NONE', *, *, #25247, .F. ) ;
#3912 = ADVANCED_FACE ( 'NONE', ( #2260 ), #89336, .T. ) ;
#3913 = FACE_OUTER_BOUND ( 'NONE', #29405, .T. ) ;
#3914 = CARTESIAN_POINT ( 'NONE',  ( 5.649999999999932854, 2.500000000000000000, 2.511473670974873507 ) ) ;
#3915 = LINE ( 'NONE', #83769, #106167 ) ;
#3916 = SHAPE_REPRESENTATION_RELATIONSHIP ( 'NONE' , 'NONE' ,  #71195, #50879 ) ;
#3917 = EDGE_CURVE ( 'NONE', #101225, #114688, #108197, .T. ) ;
#3918 = CARTESIAN_POINT ( 'NONE',  ( -6.250000000000017764, 12.50000000000000000, 7.122917578226811486 ) ) ;
#3919 = CARTESIAN_POINT ( 'NONE',  ( 6.899999999999928413, 2.500000000000000000, 4.676537180435972552 ) ) ;
#3920 = DIRECTION ( 'NONE',  ( -4.274815082592931898E-19, -0.9999939076577903929, -0.003490651415223739937 ) ) ;
#3921 = DIRECTION ( 'NONE',  ( 0.000000000000000000, 0.000000000000000000, 1.000000000000000000 ) ) ;
#3922 = AXIS2_PLACEMENT_3D ( 'NONE', #51784, #9919, #19753 ) ;
#3923 = DIRECTION ( 'NONE',  ( 0.000000000000000000, 0.000000000000000000, 1.000000000000000000 ) ) ;
#3925 = ADVANCED_FACE ( 'NONE', ( #112238 ), #26642, .T. ) ;
#3924 = DIRECTION ( 'NONE',  ( -0.000000000000000000, 1.000000000000000000, -0.000000000000000000 ) ) ;
#3926 = EDGE_LOOP ( 'NONE', ( #49968, #127080 ) ) ;
#3927 = LINE ( 'NONE', #123070, #48573 ) ;
#3928 = ORIENTED_EDGE ( 'NONE', *, *, #21995, .F. ) ;
#3929 = ORIENTED_EDGE ( 'NONE', *, *, #57386, .T. ) ;
#3930 = CARTESIAN_POINT ( 'NONE',  ( -9.150000000000009237, 2.500000000000000000, 1.472243186433545459 ) ) ;
#3931 = DIRECTION ( 'NONE',  ( -0.000000000000000000, -1.000000000000000000, -0.000000000000000000 ) ) ;
#3932 = CIRCLE ( 'NONE', #98022, 0.1000000000000002554 ) ;
#3933 = DIRECTION ( 'NONE',  ( 0.000000000000000000, 0.000000000000000000, 1.000000000000000000 ) ) ;
#3935 = AXIS2_PLACEMENT_3D ( 'NONE', #84489, #85759, #54372 ) ;
#3934 = FACE_OUTER_BOUND ( 'NONE', #103769, .T. ) ;
#3936 = DIRECTION ( 'NONE',  ( -4.274815082592931898E-19, -0.9999939076577903929, -0.003490651415223739937 ) ) ;
#3937 = DIRECTION ( 'NONE',  ( 0.000000000000000000, 0.000000000000000000, 1.000000000000000000 ) ) ;
#3938 = DIRECTION ( 'NONE',  ( 0.000000000000000000, -0.000000000000000000, 1.000000000000000000 ) ) ;
#3939 = VERTEX_POINT ( 'NONE', #82129 ) ;
#3940 = DIRECTION ( 'NONE',  ( 0.000000000000000000, -1.000000000000000000, 0.000000000000000000 ) ) ;
#3941 = CIRCLE ( 'NONE', #108491, 0.06509327318403745899 ) ;
#3942 = LINE ( 'NONE', #43892, #106478 ) ;
#3943 = VERTEX_POINT ( 'NONE', #100476 ) ;
#3944 = ORIENTED_EDGE ( 'NONE', *, *, #101444, .F. ) ;
#3946 = CIRCLE ( 'NONE', #81322, 0.06509327318403745899 ) ;
#3945 = AXIS2_PLACEMENT_3D ( 'NONE', #72081, #86212, #111317 ) ;
#3947 = EDGE_LOOP ( 'NONE', ( #28074, #39248 ) ) ;
#3948 = AXIS2_PLACEMENT_3D ( 'NONE', #90804, #60077, #1134 ) ;
#3949 = ORIENTED_EDGE ( 'NONE', *, *, #129074, .T. ) ;
#3950 = LINE ( 'NONE', #14405, #21060 ) ;
#3951 = CARTESIAN_POINT ( 'NONE',  ( 4.599999999999940137, 2.500000000000000000, -4.330127018922201643 ) ) ;
#3953 = CIRCLE ( 'NONE', #66643, 0.06509327318403745899 ) ;
#3952 = CIRCLE ( 'NONE', #54137, 0.09999999999999982514 ) ;
#3954 = CARTESIAN_POINT ( 'NONE',  ( -1.650000000000034328, 2.500000000000000000, -6.595190528383302109 ) ) ;
#3955 = EDGE_CURVE ( 'NONE', #112224, #100139, #74765, .T. ) ;
#3956 = CARTESIAN_POINT ( 'NONE',  ( 4.549999999999937650, 2.500000000000000000, 2.165063509461097713 ) ) ;
#3957 = DIRECTION ( 'NONE',  ( 0.000000000000000000, 0.000000000000000000, 1.000000000000000000 ) ) ;
#3958 = ORIENTED_EDGE ( 'NONE', *, *, #53560, .F. ) ;
#3959 = DIRECTION ( 'NONE',  ( 0.000000000000000000, -0.000000000000000000, 1.000000000000000000 ) ) ;
#3960 = DIRECTION ( 'NONE',  ( 0.000000000000000000, 1.000000000000000000, 0.000000000000000000 ) ) ;
#3961 = CARTESIAN_POINT ( 'NONE',  ( -2.300000000000033129, 2.500000000000000000, 3.883716857408420431 ) ) ;
#3963 = EDGE_CURVE ( 'NONE', #13704, #125289, #12093, .T. ) ;
#3962 = CARTESIAN_POINT ( 'NONE',  ( 179.5000000000000000, 0.9999999999999985567, -7.634788798650556707 ) ) ;
#3964 = ORIENTED_EDGE ( 'NONE', *, *, #9519, .T. ) ;
#3965 = VERTEX_POINT ( 'NONE', #12723 ) ;
#3966 = ORIENTED_EDGE ( 'NONE', *, *, #49932, .T. ) ;
#3967 = CIRCLE ( 'NONE', #56190, 0.06509327318403745899 ) ;
#3968 = CARTESIAN_POINT ( 'NONE',  ( -13.34999999999999076, 2.500000000000000000, 1.472243186433549456 ) ) ;
#3969 = CARTESIAN_POINT ( 'NONE',  ( 4.799999999999935874, 2.500000000000000000, 3.883716857408421319 ) ) ;
#3970 = CARTESIAN_POINT ( 'NONE',  ( 13.54999999999990123, 12.50000000000000000, 1.753560074763284016 ) ) ;
#3971 = CONICAL_SURFACE ( 'NONE', #85448, 0.1000000000000000472, 0.003490658503988666988 ) ;
#3972 = AXIS2_PLACEMENT_3D ( 'NONE', #22173, #119691, #31983 ) ;
#3973 = ORIENTED_EDGE ( 'NONE', *, *, #3234, .T. ) ;
#3974 = FACE_OUTER_BOUND ( 'NONE', #25334, .T. ) ;
#3975 = DIRECTION ( 'NONE',  ( -0.000000000000000000, 1.000000000000000000, -0.000000000000000000 ) ) ;
#3976 = CARTESIAN_POINT ( 'NONE',  ( 5.649999999999934630, 12.50000000000000000, -2.446380397790840266 ) ) ;
#3977 = CARTESIAN_POINT ( 'NONE',  ( -9.999999999999969802, 12.50000000000000000, -0.06509327318403970719 ) ) ;
#3978 = CARTESIAN_POINT ( 'NONE',  ( 0.000000000000000000, 12.50000000000000000, 0.000000000000000000 ) ) ;
#3979 = ORIENTED_EDGE ( 'NONE', *, *, #107477, .T. ) ;
#3980 = ORIENTED_EDGE ( 'NONE', *, *, #112367, .T. ) ;
#3981 = DIRECTION ( 'NONE',  ( 0.000000000000000000, -0.9999939076577903929, 0.003490651415223739937 ) ) ;
#3982 = PLANE ( 'NONE',  #123004 ) ;
#3983 = CIRCLE ( 'NONE', #8191, 0.09999999999999982514 ) ;
#3984 = DIRECTION ( 'NONE',  ( -0.000000000000000000, 1.000000000000000000, -0.000000000000000000 ) ) ;
#3985 = CARTESIAN_POINT ( 'NONE',  ( -12.94999999999999218, 2.500000000000000000, -2.165063509461099489 ) ) ;
#3986 = DIRECTION ( 'NONE',  ( -0.000000000000000000, 1.000000000000000000, -0.000000000000000000 ) ) ;
#3988 = EDGE_CURVE ( 'NONE', #17860, #112869, #52036, .T. ) ;
#3987 = CIRCLE ( 'NONE', #66686, 0.1000000000000002554 ) ;
#3989 = ORIENTED_EDGE ( 'NONE', *, *, #102534, .F. ) ;
#3990 = ORIENTED_EDGE ( 'NONE', *, *, #102157, .T. ) ;
#3992 = ADVANCED_FACE ( 'NONE', ( #52663 ), #92595, .T. ) ;
#3991 = CARTESIAN_POINT ( 'NONE',  ( 179.5000000000000000, 0.6250000000000000000, 7.634788798650556707 ) ) ;
#3993 = CARTESIAN_POINT ( 'NONE',  ( -1.450000000000035927, 12.50000000000000000, -6.148780366869526226 ) ) ;
#3994 = CARTESIAN_POINT ( 'NONE',  ( 16.56576425165007294, -2.500000000000000000, -6.084390597445819893 ) ) ;
#3995 = DIRECTION ( 'NONE',  ( -0.000000000000000000, 1.000000000000000000, -0.000000000000000000 ) ) ;
#3996 = ORIENTED_EDGE ( 'NONE', *, *, #58573, .F. ) ;
#3997 = EDGE_CURVE ( 'NONE', #70661, #49409, #28796, .T. ) ;
#3998 = DIRECTION ( 'NONE',  ( 0.000000000000000000, 1.000000000000000000, 0.000000000000000000 ) ) ;
#3999 = DIRECTION ( 'NONE',  ( 0.000000000000000000, 0.000000000000000000, 1.000000000000000000 ) ) ;
#4000 = VECTOR ( 'NONE', #10247, 1000.000000000000000 ) ;
#4001 = ORIENTED_EDGE ( 'NONE', *, *, #123718, .T. ) ;
#4002 = EDGE_CURVE ( 'NONE', #54614, #97758, #112884, .T. ) ;
#4003 = CARTESIAN_POINT ( 'NONE',  ( 8.099999999999923261, 2.500000000000000000, 3.983716857408420076 ) ) ;
#4004 = EDGE_CURVE ( 'NONE', #26833, #81036, #85220, .T. ) ;
#4005 = ORIENTED_EDGE ( 'NONE', *, *, #110608, .T. ) ;
#4006 = CARTESIAN_POINT ( 'NONE',  ( -12.69999999999999218, 12.50000000000000000, -4.676537180435975216 ) ) ;
#4007 = ORIENTED_EDGE ( 'NONE', *, *, #99264, .F. ) ;
#4008 = CARTESIAN_POINT ( 'NONE',  ( 4.149999999999938183, 12.50000000000000000, 2.099970236277060032 ) ) ;
#4009 = DIRECTION ( 'NONE',  ( 0.000000000000000000, 1.000000000000000000, 0.000000000000000000 ) ) ;
#4010 = EDGE_CURVE ( 'NONE', #49054, #40465, #60395, .T. ) ;
#4011 = ORIENTED_EDGE ( 'NONE', *, *, #52884, .F. ) ;
#4012 = ORIENTED_EDGE ( 'NONE', *, *, #66461, .T. ) ;
#4013 = ADVANCED_FACE ( 'NONE', ( #113515 ), #126991, .T. ) ;
#4014 = CARTESIAN_POINT ( 'NONE',  ( 186.4635416670080872, -4.367472073101519747, 7.564683531249999149 ) ) ;
#4015 = CARTESIAN_POINT ( 'NONE',  ( 14.59999999999989484, 2.500000000000000000, -2.276824562219559311E-15 ) ) ;
#4016 = VECTOR ( 'NONE', #879, 1000.000000000000000 ) ;
#4017 = DIRECTION ( 'NONE',  ( 0.000000000000000000, 1.000000000000000000, 0.000000000000000000 ) ) ;
#4018 = CARTESIAN_POINT ( 'NONE',  ( 186.3593750003414016, 0.000000000000000000, 7.564683531250000925 ) ) ;
#4019 = CARTESIAN_POINT ( 'NONE',  ( 8.749999999999918288, 12.50000000000000000, -1.407149913249512663 ) ) ;
#4020 = DIRECTION ( 'NONE',  ( 0.000000000000000000, 1.000000000000000000, 0.000000000000000000 ) ) ;
#4021 = DIRECTION ( 'NONE',  ( 0.000000000000000000, 0.000000000000000000, 1.000000000000000000 ) ) ;
#4022 = CARTESIAN_POINT ( 'NONE',  ( -1.050000000000038236, 2.500000000000000000, -1.718653347947326049 ) ) ;
#4023 = AXIS2_PLACEMENT_3D ( 'NONE', #81368, #71521, #10037 ) ;
#4024 = VERTEX_POINT ( 'NONE', #16587 ) ;
#4025 = EDGE_LOOP ( 'NONE', ( #2773, #92321, #102969, #50377 ) ) ;
#4026 = DIRECTION ( 'NONE',  ( 0.000000000000000000, 0.000000000000000000, 1.000000000000000000 ) ) ;
#4027 = CIRCLE ( 'NONE', #54225, 0.1000000000000000472 ) ;
#4028 = ORIENTED_EDGE ( 'NONE', *, *, #106933, .T. ) ;
#4029 = CARTESIAN_POINT ( 'NONE',  ( -2.300000000000032685, 12.50000000000000000, -0.2813168883297409439 ) ) ;
#4030 = DIRECTION ( 'NONE',  ( 0.000000000000000000, 0.000000000000000000, 1.000000000000000000 ) ) ;
#4031 = CARTESIAN_POINT ( 'NONE',  ( -1.450000000000035039, 12.50000000000000000, -6.841600689897077814 ) ) ;
#4032 = CIRCLE ( 'NONE', #58357, 0.1000000000000002554 ) ;
#4034 = ORIENTED_EDGE ( 'NONE', *, *, #25162, .F. ) ;
#4033 = ORIENTED_EDGE ( 'NONE', *, *, #125096, .F. ) ;
#4035 = FACE_BOUND ( 'NONE', #85849, .T. ) ;
#4036 = ORIENTED_EDGE ( 'NONE', *, *, #102433, .F. ) ;
#4037 = CARTESIAN_POINT ( 'NONE',  ( 6.699999999999928235, 2.500000000000000000, -2.276824562219559311E-15 ) ) ;
#4038 = DIRECTION ( 'NONE',  ( 0.4999999999999471534, 0.000000000000000000, 0.8660254037844692387 ) ) ;
#4039 = ORIENTED_EDGE ( 'NONE', *, *, #91263, .T. ) ;
#4040 = CARTESIAN_POINT ( 'NONE',  ( 3.149999999999944400, 2.500000000000000000, 1.918653347947321564 ) ) ;
#4043 = DIRECTION ( 'NONE',  ( 0.000000000000000000, 0.000000000000000000, -1.000000000000000000 ) ) ;
#4042 = AXIS2_PLACEMENT_3D ( 'NONE', #120863, #71118, #118933 ) ;
#4041 = AXIS2_PLACEMENT_3D ( 'NONE', #26014, #73175, #85564 ) ;
#4044 = EDGE_CURVE ( 'NONE', #62105, #10563, #70544, .T. ) ;
#4045 = DIRECTION ( 'NONE',  ( 0.000000000000000000, -0.000000000000000000, 1.000000000000000000 ) ) ;
#4046 = DIRECTION ( 'NONE',  ( 0.000000000000000000, 1.000000000000000000, 0.000000000000000000 ) ) ;
#4047 = CARTESIAN_POINT ( 'NONE',  ( -9.150000000000005684, 12.50000000000000000, 7.188010851410848723 ) ) ;
#4048 = FACE_OUTER_BOUND ( 'NONE', #73324, .T. ) ;
#4049 = CARTESIAN_POINT ( 'NONE',  ( 185.9843750003414016, -8.734944146203032389, -1.604583208406767949E-15 ) ) ;
#4050 = CARTESIAN_POINT ( 'NONE',  ( -7.900000000000014566, 2.500000000000000000, -5.022947341949754119 ) ) ;
#4051 = DIRECTION ( 'NONE',  ( 0.000000000000000000, 1.000000000000000000, 0.000000000000000000 ) ) ;
#4052 = ADVANCED_FACE ( 'NONE', ( #14013 ), #26927, .T. ) ;
#4053 = ORIENTED_EDGE ( 'NONE', *, *, #111507, .T. ) ;
#4054 = ORIENTED_EDGE ( 'NONE', *, *, #59311, .F. ) ;
#4055 = VERTEX_POINT ( 'NONE', #44136 ) ;
#4056 = DIRECTION ( 'NONE',  ( 0.000000000000000000, 1.000000000000000000, 0.000000000000000000 ) ) ;
#4057 = ORIENTED_EDGE ( 'NONE', *, *, #38524, .T. ) ;
#4058 = EDGE_CURVE ( 'NONE', #14402, #40007, #122785, .T. ) ;
#4060 = VERTEX_POINT ( 'NONE', #5481 ) ;
#4059 = ORIENTED_EDGE ( 'NONE', *, *, #105278, .F. ) ;
#4061 = ORIENTED_EDGE ( 'NONE', *, *, #128557, .T. ) ;
#4062 = EDGE_CURVE ( 'NONE', #75765, #89533, #37117, .T. ) ;
#4063 = CARTESIAN_POINT ( 'NONE',  ( 8.349999999999919709, 2.500000000000000000, 7.188010851410848723 ) ) ;
#4064 = EDGE_CURVE ( 'NONE', #95559, #31928, #64417, .T. ) ;
#4065 = CIRCLE ( 'NONE', #129584, 0.1000000000000002554 ) ;
#4066 = CONICAL_SURFACE ( 'NONE', #8266, 0.1000000000000000472, 0.003490658503988666988 ) ;
#4067 = CARTESIAN_POINT ( 'NONE',  ( 4.349999999999941025, 12.50000000000000000, -1.818653347947326138 ) ) ;
#4068 = ADVANCED_FACE ( 'NONE', ( #114800 ), #18310, .T. ) ;
#4069 = CARTESIAN_POINT ( 'NONE',  ( 76.44836599025838098, -3.583082431487559560, -6.086789564813110509 ) ) ;
#4070 = DIRECTION ( 'NONE',  ( 0.000000000000000000, -0.000000000000000000, 1.000000000000000000 ) ) ;
#4071 = FACE_OUTER_BOUND ( 'NONE', #75868, .T. ) ;
#4072 = ORIENTED_EDGE ( 'NONE', *, *, #56547, .F. ) ;
#4075 = EDGE_CURVE ( 'NONE', #79185, #78982, #85349, .T. ) ;
#4074 = LINE ( 'NONE', #23735, #18374 ) ;
#4073 = AXIS2_PLACEMENT_3D ( 'NONE', #33259, #64622, #84909 ) ;
#4076 = ORIENTED_EDGE ( 'NONE', *, *, #124165, .T. ) ;
#4077 = CIRCLE ( 'NONE', #125075, 0.1000000000000002554 ) ;
#4078 = ADVANCED_FACE ( 'NONE', ( #35615 ), #95596, .T. ) ;
#4079 = ORIENTED_EDGE ( 'NONE', *, *, #21227, .T. ) ;
#4080 = ORIENTED_EDGE ( 'NONE', *, *, #78238, .F. ) ;
#4081 = CARTESIAN_POINT ( 'NONE',  ( 11.84999999999990372, 2.500000000000000000, -6.841600689897078702 ) ) ;
#4082 = ORIENTED_EDGE ( 'NONE', *, *, #63387, .T. ) ;
#4083 = ORIENTED_EDGE ( 'NONE', *, *, #120492, .F. ) ;
#4084 = ORIENTED_EDGE ( 'NONE', *, *, #34946, .F. ) ;
#4085 = CIRCLE ( 'NONE', #20821, 0.1000000000000002554 ) ;
#4086 = CIRCLE ( 'NONE', #98174, 0.1000000000000002554 ) ;
#4087 = CARTESIAN_POINT ( 'NONE',  ( 13.74999999999989342, 12.50000000000000000, -1.472243186433550122 ) ) ;
#4088 = PLANE ( 'NONE',  #87641 ) ;
#4089 = FACE_OUTER_BOUND ( 'NONE', #29347, .T. ) ;
#4090 = DIRECTION ( 'NONE',  ( -0.000000000000000000, 1.000000000000000000, -0.000000000000000000 ) ) ;
#4091 = CARTESIAN_POINT ( 'NONE',  ( -3.100000000000028511, 2.500000000000000000, -4.083716857408426826 ) ) ;
#4092 = CARTESIAN_POINT ( 'NONE',  ( 10.39999999999991509, 2.500000000000000000, -0.7928203230275543412 ) ) ;
#4093 = ORIENTED_EDGE ( 'NONE', *, *, #92540, .T. ) ;
#4094 = CARTESIAN_POINT ( 'NONE',  ( 10.79999999999991012, 2.500000000000000000, 4.230127018922196669 ) ) ;
#4095 = ORIENTED_EDGE ( 'NONE', *, *, #99675, .T. ) ;
#4096 = DIRECTION ( 'NONE',  ( -0.000000000000000000, -1.000000000000000000, -0.000000000000000000 ) ) ;
#4097 = AXIS2_PLACEMENT_3D ( 'NONE', #10032, #70886, #21131 ) ;
#4098 = EDGE_LOOP ( 'NONE', ( #47396, #72839 ) ) ;
#4099 = ORIENTED_EDGE ( 'NONE', *, *, #122595, .T. ) ;
#4100 = DIRECTION ( 'NONE',  ( 0.000000000000000000, 0.000000000000000000, 1.000000000000000000 ) ) ;
#4101 = PLANE ( 'NONE',  #86081 ) ;
#4102 = DIRECTION ( 'NONE',  ( 0.000000000000000000, -0.000000000000000000, 1.000000000000000000 ) ) ;
#4103 = VERTEX_POINT ( 'NONE', #4835 ) ;
#4104 = ORIENTED_EDGE ( 'NONE', *, *, #25081, .T. ) ;
#4105 = DIRECTION ( 'NONE',  ( 0.000000000000000000, 0.000000000000000000, 1.000000000000000000 ) ) ;
#4106 = CARTESIAN_POINT ( 'NONE',  ( -10.40000000000000213, 2.500000000000000000, -0.7928203230275542301 ) ) ;
#4107 = FACE_OUTER_BOUND ( 'NONE', #44945, .T. ) ;
#4108 = CARTESIAN_POINT ( 'NONE',  ( 12.09999999999990195, 12.50000000000000000, -0.06509327318403970719 ) ) ;
#4110 = ADVANCED_FACE ( 'NONE', ( #65705 ), #54581, .T. ) ;
#4109 = DIRECTION ( 'NONE',  ( 0.000000000000000000, 0.000000000000000000, 1.000000000000000000 ) ) ;
#4111 = ORIENTED_EDGE ( 'NONE', *, *, #2262, .T. ) ;
#4112 = AXIS2_PLACEMENT_3D ( 'NONE', #119029, #29370, #67979 ) ;
#4113 = ORIENTED_EDGE ( 'NONE', *, *, #98594, .F. ) ;
#4114 = CARTESIAN_POINT ( 'NONE',  ( 9.149999999999916866, 12.50000000000000000, 5.802370205355744659 ) ) ;
#4115 = DIRECTION ( 'NONE',  ( -0.000000000000000000, 1.000000000000000000, -0.000000000000000000 ) ) ;
#4117 = CIRCLE ( 'NONE', #58535, 0.06509327318403745899 ) ;
#4116 = AXIS2_PLACEMENT_3D ( 'NONE', #115513, #15379, #53404 ) ;
#4118 = CONICAL_SURFACE ( 'NONE', #77292, 0.1000000000000000056, 0.003490658503988666988 ) ;
#4119 = CARTESIAN_POINT ( 'NONE',  ( 184.5885416670080872, -6.551208109652273848, -3.782341765625003571 ) ) ;
#4120 = LINE ( 'NONE', #104275, #101288 ) ;
#4121 = DIRECTION ( 'NONE',  ( 0.000000000000000000, 1.000000000000000000, 0.000000000000000000 ) ) ;
#4122 = FACE_OUTER_BOUND ( 'NONE', #118413, .T. ) ;
#4123 = DIRECTION ( 'NONE',  ( 0.000000000000000000, 0.000000000000000000, 1.000000000000000000 ) ) ;
#4124 = VERTEX_POINT ( 'NONE', #105643 ) ;
#4126 = CIRCLE ( 'NONE', #6186, 0.06509327318403745899 ) ;
#4125 = AXIS2_PLACEMENT_3D ( 'NONE', #108901, #88638, #109573 ) ;
#4127 = DIRECTION ( 'NONE',  ( -0.000000000000000000, -1.000000000000000000, -0.000000000000000000 ) ) ;
#4128 = DIRECTION ( 'NONE',  ( -0.000000000000000000, 1.000000000000000000, -0.000000000000000000 ) ) ;
#4129 = CARTESIAN_POINT ( 'NONE',  ( 5.849999999999933920, 12.50000000000000000, -2.099970236277064473 ) ) ;
#4130 = VERTEX_POINT ( 'NONE', #55881 ) ;
#4131 = CARTESIAN_POINT ( 'NONE',  ( -10.40000000000000213, 2.500000000000000000, 4.330127018922196314 ) ) ;
#4132 = EDGE_LOOP ( 'NONE', ( #107418, #65072 ) ) ;
#4133 = FACE_OUTER_BOUND ( 'NONE', #85494, .T. ) ;
#4134 = VERTEX_POINT ( 'NONE', #6130 ) ;
#4135 = LINE ( 'NONE', #55203, #110696 ) ;
#4136 = CARTESIAN_POINT ( 'NONE',  ( -2.950000000000029932, 12.50000000000000000, -2.165063509461101710 ) ) ;
#4137 = LINE ( 'NONE', #93199, #27645 ) ;
#4138 = ORIENTED_EDGE ( 'NONE', *, *, #105334, .F. ) ;
#4139 = AXIS2_PLACEMENT_3D ( 'NONE', #103644, #4765, #93187 ) ;
#4140 = ADVANCED_FACE ( 'NONE', ( #33677 ), #93539, .T. ) ;
#4141 = DIRECTION ( 'NONE',  ( 0.000000000000000000, 0.000000000000000000, -1.000000000000000000 ) ) ;
#4142 = CIRCLE ( 'NONE', #108714, 0.06509327318403745899 ) ;
#4143 = DIRECTION ( 'NONE',  ( 0.000000000000000000, 1.000000000000000000, 0.000000000000000000 ) ) ;
#4144 = EDGE_CURVE ( 'NONE', #33469, #22448, #49642, .T. ) ;
#4145 = ADVANCED_FACE ( 'NONE', ( #76181 ), #76820, .T. ) ;
#4146 = ORIENTED_EDGE ( 'NONE', *, *, #13081, .F. ) ;
#4147 = CIRCLE ( 'NONE', #18748, 0.09999999999999999167 ) ;
#4148 = DIRECTION ( 'NONE',  ( -4.274815082592931898E-19, -0.9999939076577903929, -0.003490651415223739937 ) ) ;
#4149 = ORIENTED_EDGE ( 'NONE', *, *, #6410, .T. ) ;
#4150 = VERTEX_POINT ( 'NONE', #53962 ) ;
#4151 = CARTESIAN_POINT ( 'NONE',  ( 7.949999999999925571, 2.500000000000000000, -6.495190528383302464 ) ) ;
#4152 = FACE_OUTER_BOUND ( 'NONE', #108400, .T. ) ;
#4153 = ADVANCED_FACE ( 'NONE', ( #93888 ), #123973, .T. ) ;
#4154 = ADVANCED_FACE ( 'NONE', ( #90430 ), #40072, .T. ) ;
#4155 = CARTESIAN_POINT ( 'NONE',  ( -9.550000000000007816, 2.500000000000000000, -6.495190528383297135 ) ) ;
#4156 = EDGE_CURVE ( 'NONE', #73914, #2455, #79986, .T. ) ;
#4157 = EDGE_LOOP ( 'NONE', ( #44282, #80842 ) ) ;
#4158 = EDGE_CURVE ( 'NONE', #28402, #33970, #24580, .T. ) ;
#4159 = DIRECTION ( 'NONE',  ( 0.000000000000000000, 0.000000000000000000, 1.000000000000000000 ) ) ;
#4160 = DIRECTION ( 'NONE',  ( 0.000000000000000000, 1.000000000000000000, 0.000000000000000000 ) ) ;
#4161 = EDGE_LOOP ( 'NONE', ( #113793, #119172 ) ) ;
#4163 = FACE_OUTER_BOUND ( 'NONE', #57142, .T. ) ;
#4162 = VECTOR ( 'NONE', #127772, 1000.000000000000000 ) ;
#4164 = DIRECTION ( 'NONE',  ( -0.000000000000000000, -1.000000000000000000, -0.000000000000000000 ) ) ;
#4165 = CIRCLE ( 'NONE', #94074, 0.1000000000000000472 ) ;
#4166 = CARTESIAN_POINT ( 'NONE',  ( -2.950000000000030376, 2.500000000000000000, 6.595190528383296780 ) ) ;
#4167 = DIRECTION ( 'NONE',  ( 0.000000000000000000, 0.000000000000000000, 1.000000000000000000 ) ) ;
#4168 = CARTESIAN_POINT ( 'NONE',  ( 9.149999999999916866, 12.50000000000000000, -1.472243186433550122 ) ) ;
#4169 = AXIS2_PLACEMENT_3D ( 'NONE', #78619, #38026, #117198 ) ;
#4170 = PLANE ( 'NONE',  #24238 ) ;
#4171 = DIRECTION ( 'NONE',  ( -0.000000000000000000, 1.000000000000000000, -0.000000000000000000 ) ) ;
#4172 = AXIS2_PLACEMENT_3D ( 'NONE', #93028, #43934, #3352 ) ;
#4173 = ORIENTED_EDGE ( 'NONE', *, *, #38049, .T. ) ;
#4174 = EDGE_LOOP ( 'NONE', ( #84363, #39397, #101141, #45765 ) ) ;
#4175 = EDGE_LOOP ( 'NONE', ( #125051, #72045 ) ) ;
#4176 = VERTEX_POINT ( 'NONE', #110095 ) ;
#4177 = AXIS2_PLACEMENT_3D ( 'NONE', #96245, #74046, #44589 ) ;
#4178 = DIRECTION ( 'NONE',  ( 0.000000000000000000, 0.000000000000000000, 1.000000000000000000 ) ) ;
#4179 = CARTESIAN_POINT ( 'NONE',  ( -10.45000000000000462, 12.50000000000000000, -2.165063509461097713 ) ) ;
#4180 = LINE ( 'NONE', #36894, #55201 ) ;
#4181 = ORIENTED_EDGE ( 'NONE', *, *, #61194, .T. ) ;
#4182 = FACE_BOUND ( 'NONE', #25201, .T. ) ;
#4183 = CARTESIAN_POINT ( 'NONE',  ( 4.999999999999936939, 12.50000000000000000, -0.6928203230275541413 ) ) ;
#4184 = DIRECTION ( 'NONE',  ( -0.000000000000000000, -1.000000000000000000, -0.000000000000000000 ) ) ;
#4185 = DIRECTION ( 'NONE',  ( -0.000000000000000000, 1.000000000000000000, -0.000000000000000000 ) ) ;
#4186 = DIRECTION ( 'NONE',  ( 0.000000000000000000, 1.000000000000000000, 0.000000000000000000 ) ) ;
#4187 = DIRECTION ( 'NONE',  ( 0.000000000000000000, 0.000000000000000000, -1.000000000000000000 ) ) ;
#4188 = FACE_OUTER_BOUND ( 'NONE', #71687, .T. ) ;
#4189 = DIRECTION ( 'NONE',  ( 0.000000000000000000, 0.000000000000000000, 1.000000000000000000 ) ) ;
#4190 = DIRECTION ( 'NONE',  ( 0.000000000000000000, 1.000000000000000000, 0.000000000000000000 ) ) ;
#4191 = EDGE_CURVE ( 'NONE', #67661, #66137, #774, .T. ) ;
#4192 = CARTESIAN_POINT ( 'NONE',  ( -8.350000000000013856, 12.50000000000000000, -7.188010851410848723 ) ) ;
#4193 = DIRECTION ( 'NONE',  ( 0.000000000000000000, 0.000000000000000000, -1.000000000000000000 ) ) ;
#4194 = ORIENTED_EDGE ( 'NONE', *, *, #91505, .F. ) ;
#4195 = ORIENTED_EDGE ( 'NONE', *, *, #62156, .T. ) ;
#4196 = ORIENTED_EDGE ( 'NONE', *, *, #18388, .T. ) ;
#4197 = ORIENTED_EDGE ( 'NONE', *, *, #40606, .T. ) ;
#4198 = VERTEX_POINT ( 'NONE', #32203 ) ;
#4199 = EDGE_LOOP ( 'NONE', ( #79139, #116545, #27547, #82547 ) ) ;
#4201 = ADVANCED_FACE ( 'NONE', ( #70809 ), #72705, .T. ) ;
#4200 = VECTOR ( 'NONE', #72995, 1000.000000000000000 ) ;
#4202 = DIRECTION ( 'NONE',  ( 0.000000000000000000, 1.000000000000000000, 0.000000000000000000 ) ) ;
#4203 = ADVANCED_FACE ( 'NONE', ( #51190 ), #91575, .T. ) ;
#4204 = AXIS2_PLACEMENT_3D ( 'NONE', #1181, #122259, #91494 ) ;
#4205 = ORIENTED_EDGE ( 'NONE', *, *, #29732, .F. ) ;
#4206 = ORIENTED_EDGE ( 'NONE', *, *, #1401, .T. ) ;
#4207 = EDGE_CURVE ( 'NONE', #95831, #57530, #10010, .T. ) ;
#4208 = ADVANCED_FACE ( 'NONE', ( #50520 ), #66432, .T. ) ;
#4210 = AXIS2_PLACEMENT_3D ( 'NONE', #73550, #21906, #33647 ) ;
#4209 = VECTOR ( 'NONE', #13300, 1000.000000000000000 ) ;
#4211 = CARTESIAN_POINT ( 'NONE',  ( 12.07106445316801846, -2.499999999999745981, 8.629160867383669498 ) ) ;
#4212 = LINE ( 'NONE', #123997, #16533 ) ;
#4213 = DIRECTION ( 'NONE',  ( -4.274815082592931898E-19, -0.9999939076577903929, -0.003490651415223739937 ) ) ;
#4214 = EDGE_CURVE ( 'NONE', #16687, #89315, #60989, .T. ) ;
#4215 = ADVANCED_FACE ( 'NONE', ( #112032 ), #60201, .T. ) ;
#4216 = EDGE_LOOP ( 'NONE', ( #23715, #93666 ) ) ;
#4217 = DIRECTION ( 'NONE',  ( -0.000000000000000000, 1.000000000000000000, -0.000000000000000000 ) ) ;
#4218 = EDGE_CURVE ( 'NONE', #64387, #112983, #87352, .T. ) ;
#4219 = CONICAL_SURFACE ( 'NONE', #16726, 0.1000000000000000056, 0.003490658503988666988 ) ;
#4220 = ADVANCED_FACE ( 'NONE', ( #99638 ), #39453, .T. ) ;
#4221 = EDGE_LOOP ( 'NONE', ( #55316, #97115 ) ) ;
#4222 = EDGE_CURVE ( 'NONE', #41353, #123277, #11233, .T. ) ;
#4223 = ORIENTED_EDGE ( 'NONE', *, *, #40290, .F. ) ;
#4225 = EDGE_LOOP ( 'NONE', ( #113010, #83024, #74227, #78648 ) ) ;
#4224 = CARTESIAN_POINT ( 'NONE',  ( -2.050000000000033129, 12.50000000000000000, 6.495190528383297135 ) ) ;
#4226 = DIRECTION ( 'NONE',  ( 0.000000000000000000, 0.000000000000000000, 1.000000000000000000 ) ) ;
#4227 = ORIENTED_EDGE ( 'NONE', *, *, #73166, .F. ) ;
#4228 = EDGE_CURVE ( 'NONE', #123416, #62801, #114543, .T. ) ;
#4229 = DIRECTION ( 'NONE',  ( 0.000000000000000000, -0.000000000000000000, 1.000000000000000000 ) ) ;
#4230 = CARTESIAN_POINT ( 'NONE',  ( 11.84999999999990727, 2.500000000000000000, -2.511473670974877948 ) ) ;
#4231 = CARTESIAN_POINT ( 'NONE',  ( -11.04999999999999893, 2.500000000000000000, 6.248780366869520542 ) ) ;
#4232 = DIRECTION ( 'NONE',  ( -4.274815082592931898E-19, -0.9999939076577903929, -0.003490651415223739937 ) ) ;
#4233 = DIRECTION ( 'NONE',  ( -0.000000000000000000, 1.000000000000000000, -0.000000000000000000 ) ) ;
#4234 = ORIENTED_EDGE ( 'NONE', *, *, #126215, .T. ) ;
#4235 = DIRECTION ( 'NONE',  ( 0.000000000000000000, 0.000000000000000000, 1.000000000000000000 ) ) ;
#4236 = VECTOR ( 'NONE', #5837, 1000.000000000000000 ) ;
#4237 = AXIS2_PLACEMENT_3D ( 'NONE', #71882, #98734, #30025 ) ;
#4238 = ORIENTED_EDGE ( 'NONE', *, *, #68714, .T. ) ;
#4239 = CARTESIAN_POINT ( 'NONE',  ( -2.700000000000030376, 2.500000000000000000, 3.983716857408420964 ) ) ;
#4240 = VERTEX_POINT ( 'NONE', #31537 ) ;
#4241 = CARTESIAN_POINT ( 'NONE',  ( -4.600000000000028066, 2.500000000000000000, -3.537306695894649966 ) ) ;
#4242 = LINE ( 'NONE', #44181, #55314 ) ;
#4243 = FACE_OUTER_BOUND ( 'NONE', #97825, .T. ) ;
#4244 = DIRECTION ( 'NONE',  ( 0.000000000000000000, 1.000000000000000000, 0.000000000000000000 ) ) ;
#4245 = ORIENTED_EDGE ( 'NONE', *, *, #8216, .F. ) ;
#4246 = DIRECTION ( 'NONE',  ( 0.000000000000000000, -0.000000000000000000, 1.000000000000000000 ) ) ;
#4247 = VERTEX_POINT ( 'NONE', #71443 ) ;
#4248 = ORIENTED_EDGE ( 'NONE', *, *, #106557, .T. ) ;
#4249 = VERTEX_POINT ( 'NONE', #111359 ) ;
#4250 = CARTESIAN_POINT ( 'NONE',  ( -6.050000000000022027, 2.500000000000000000, -1.818653347947326138 ) ) ;
#4251 = DIRECTION ( 'NONE',  ( 0.000000000000000000, 1.000000000000000000, 0.000000000000000000 ) ) ;
#4252 = CARTESIAN_POINT ( 'NONE',  ( 184.5677083336747444, -4.367472073101514418, -7.564683531250002702 ) ) ;
#4253 = DIRECTION ( 'NONE',  ( 0.000000000000000000, 0.000000000000000000, 1.000000000000000000 ) ) ;
#4254 = CONICAL_SURFACE ( 'NONE', #60722, 0.09999999999999999167, 0.003490658503988666988 ) ;
#4255 = CIRCLE ( 'NONE', #31476, 0.06509327318403745899 ) ;
#4257 = EDGE_CURVE ( 'NONE', #84067, #50060, #76906, .T. ) ;
#4256 = CARTESIAN_POINT ( 'NONE',  ( -1.850000000000033396, 2.500000000000000000, -6.148780366869526226 ) ) ;
#4258 = CARTESIAN_POINT ( 'NONE',  ( -3.150000000000030109, 2.500000000000000000, -2.511473670974877948 ) ) ;
#4259 = AXIS2_PLACEMENT_3D ( 'NONE', #32039, #111201, #73872 ) ;
#4260 = VERTEX_POINT ( 'NONE', #109449 ) ;
#4261 = DIRECTION ( 'NONE',  ( -0.000000000000000000, 1.000000000000000000, -0.000000000000000000 ) ) ;
#4262 = VERTEX_POINT ( 'NONE', #59732 ) ;
#4263 = CONICAL_SURFACE ( 'NONE', #58679, 0.1000000000000002554, 0.003490658503988666988 ) ;
#4264 = DIRECTION ( 'NONE',  ( 0.000000000000000000, 1.000000000000000000, 0.000000000000000000 ) ) ;
#4265 = EDGE_CURVE ( 'NONE', #41760, #70628, #62250, .T. ) ;
#4266 = CARTESIAN_POINT ( 'NONE',  ( 1.049999999999954525, 2.500000000000000000, 1.918653347947321564 ) ) ;
#4267 = PLANE ( 'NONE',  #15048 ) ;
#4268 = CARTESIAN_POINT ( 'NONE',  ( -7.700000000000010836, 12.50000000000000000, 4.048810130592458201 ) ) ;
#4269 = ORIENTED_EDGE ( 'NONE', *, *, #43968, .F. ) ;
#4270 = CARTESIAN_POINT ( 'NONE',  ( -3.950000000000028155, 2.500000000000000000, -6.741600689897077281 ) ) ;
#4272 = ORIENTED_EDGE ( 'NONE', *, *, #82245, .F. ) ;
#4271 = CARTESIAN_POINT ( 'NONE',  ( -10.40000000000000213, 2.500000000000000000, -2.276824562219559311E-15 ) ) ;
#4273 = EDGE_LOOP ( 'NONE', ( #110406, #64430 ) ) ;
#4274 = DIRECTION ( 'NONE',  ( -0.000000000000000000, -1.000000000000000000, -0.000000000000000000 ) ) ;
#4275 = VERTEX_POINT ( 'NONE', #117001 ) ;
#4276 = EDGE_LOOP ( 'NONE', ( #96480, #68958 ) ) ;
#4277 = CARTESIAN_POINT ( 'NONE',  ( -2.300000000000033573, 2.500000000000000000, 4.676537180435972552 ) ) ;
#4278 = CIRCLE ( 'NONE', #113058, 0.1000000000000002554 ) ;
#4279 = CIRCLE ( 'NONE', #18965, 0.06509327318403745899 ) ;
#4280 = ORIENTED_EDGE ( 'NONE', *, *, #128761, .T. ) ;
#4281 = CARTESIAN_POINT ( 'NONE',  ( -7.950000000000016165, 12.50000000000000000, -6.495190528383297135 ) ) ;
#4282 = DIRECTION ( 'NONE',  ( 0.000000000000000000, 1.000000000000000000, 0.000000000000000000 ) ) ;
#4283 = CARTESIAN_POINT ( 'NONE',  ( 5.399999999999933742, 2.500000000000000000, -0.1000000000000023925 ) ) ;
#4284 = VERTEX_POINT ( 'NONE', #65987 ) ;
#4285 = EDGE_CURVE ( 'NONE', #54835, #43630, #45620, .T. ) ;
#4286 = AXIS2_PLACEMENT_3D ( 'NONE', #68856, #60351, #108773 ) ;
#4287 = CARTESIAN_POINT ( 'NONE',  ( -8.550000000000013145, 2.500000000000000000, -1.918653347947326004 ) ) ;
#4289 = VERTEX_POINT ( 'NONE', #115725 ) ;
#4288 = LINE ( 'NONE', #104450, #3483 ) ;
#4290 = DIRECTION ( 'NONE',  ( 0.000000000000000000, -0.9999939076577903929, 0.003490651415223739937 ) ) ;
#4291 = FACE_OUTER_BOUND ( 'NONE', #120303, .T. ) ;
#4292 = EDGE_CURVE ( 'NONE', #115818, #119776, #26075, .T. ) ;
#4293 = EDGE_LOOP ( 'NONE', ( #6740, #126868, #41678, #103241 ) ) ;
#4294 = ORIENTED_EDGE ( 'NONE', *, *, #57130, .T. ) ;
#4295 = ORIENTED_EDGE ( 'NONE', *, *, #4356, .T. ) ;
#4296 = PLANE ( 'NONE',  #108997 ) ;
#4297 = CARTESIAN_POINT ( 'NONE',  ( 4.913542845176413820, 1.499999999999745981, 9.942462991075640133 ) ) ;
#4298 = EDGE_CURVE ( 'NONE', #55110, #22492, #5776, .T. ) ;
#4299 = ADVANCED_FACE ( 'NONE', ( #96724 ), #58137, .T. ) ;
#4300 = CARTESIAN_POINT ( 'NONE',  ( -13.54999999999999005, 2.500000000000000000, -1.718653347947323828 ) ) ;
#4301 = EDGE_CURVE ( 'NONE', #122300, #10500, #33486, .T. ) ;
#4302 = FACE_BOUND ( 'NONE', #108885, .T. ) ;
#4304 = ADVANCED_FACE ( 'NONE', ( #16220 ), #106551, .T. ) ;
#4303 = ORIENTED_EDGE ( 'NONE', *, *, #4156, .T. ) ;
#4305 = CARTESIAN_POINT ( 'NONE',  ( 186.3593750003414016, 0.000000000000000000, 7.564683531250000925 ) ) ;
#4306 = EDGE_CURVE ( 'NONE', #116514, #30053, #112420, .T. ) ;
#4307 = DIRECTION ( 'NONE',  ( 0.000000000000000000, 0.000000000000000000, 1.000000000000000000 ) ) ;
#4308 = CARTESIAN_POINT ( 'NONE',  ( 6.249999999999930722, 2.500000000000000000, 1.472243186433545459 ) ) ;
#4309 = CARTESIAN_POINT ( 'NONE',  ( -6.450000000000017941, 2.500000000000000000, -6.741600689897077281 ) ) ;
#4310 = DIRECTION ( 'NONE',  ( 0.000000000000000000, 1.000000000000000000, 0.000000000000000000 ) ) ;
#4311 = EDGE_CURVE ( 'NONE', #128555, #22839, #53116, .T. ) ;
#4312 = DIRECTION ( 'NONE',  ( -4.274815082592931898E-19, -0.9999939076577903929, -0.003490651415223739937 ) ) ;
#4313 = EDGE_CURVE ( 'NONE', #30210, #33390, #129168, .T. ) ;
#4314 = AXIS2_PLACEMENT_3D ( 'NONE', #31490, #32795, #110050 ) ;
#4315 = ADVANCED_FACE ( 'NONE', ( #3363 ), #122883, .T. ) ;
#4316 = VECTOR ( 'NONE', #129530, 1000.000000000000000 ) ;
#4317 = FACE_OUTER_BOUND ( 'NONE', #42845, .T. ) ;
#4318 = ORIENTED_EDGE ( 'NONE', *, *, #127317, .F. ) ;
#4319 = EDGE_LOOP ( 'NONE', ( #124447, #94891, #76695, #79785 ) ) ;
#4320 = ORIENTED_EDGE ( 'NONE', *, *, #74363, .T. ) ;
#4321 = ORIENTED_EDGE ( 'NONE', *, *, #36425, .T. ) ;
#4322 = ORIENTED_EDGE ( 'NONE', *, *, #108668, .T. ) ;
#4323 = DIRECTION ( 'NONE',  ( 0.000000000000000000, 1.000000000000000000, 0.000000000000000000 ) ) ;
#4324 = DIRECTION ( 'NONE',  ( 0.000000000000000000, 0.000000000000000000, 1.000000000000000000 ) ) ;
#4325 = EDGE_LOOP ( 'NONE', ( #10689, #112272, #51009, #44829 ) ) ;
#4326 = FACE_BOUND ( 'NONE', #14880, .T. ) ;
#4327 = AXIS2_PLACEMENT_3D ( 'NONE', #44232, #52769, #64520 ) ;
#4328 = DIRECTION ( 'NONE',  ( 0.000000000000000000, 0.000000000000000000, 1.000000000000000000 ) ) ;
#4329 = DIRECTION ( 'NONE',  ( -0.000000000000000000, 1.000000000000000000, -0.000000000000000000 ) ) ;
#4330 = ORIENTED_EDGE ( 'NONE', *, *, #114609, .T. ) ;
#4331 = CARTESIAN_POINT ( 'NONE',  ( 4.799999999999935874, 12.50000000000000000, 0.4115034346978109769 ) ) ;
#4332 = FACE_OUTER_BOUND ( 'NONE', #78132, .T. ) ;
#4333 = CARTESIAN_POINT ( 'NONE',  ( -6.850000000000017408, 12.50000000000000000, -2.511473670974877948 ) ) ;
#4334 = ORIENTED_EDGE ( 'NONE', *, *, #60248, .T. ) ;
#4335 = CARTESIAN_POINT ( 'NONE',  ( -1.900000000000034994, 2.500000000000000000, -0.3464101615137783474 ) ) ;
#4336 = CIRCLE ( 'NONE', #94249, 0.06509327318403741736 ) ;
#4337 = VERTEX_POINT ( 'NONE', #72751 ) ;
#4338 = AXIS2_PLACEMENT_3D ( 'NONE', #107187, #77098, #129449 ) ;
#4339 = ORIENTED_EDGE ( 'NONE', *, *, #88997, .T. ) ;
#4340 = VERTEX_POINT ( 'NONE', #105272 ) ;
#4341 = CARTESIAN_POINT ( 'NONE',  ( 12.89999999999990266, 12.50000000000000000, -5.022947341949754119 ) ) ;
#4342 = CARTESIAN_POINT ( 'NONE',  ( 1.249999999999950262, 2.500000000000000000, 7.288010851410849256 ) ) ;
#4343 = DIRECTION ( 'NONE',  ( -4.274815082592931898E-19, -0.9999939076577903929, -0.003490651415223739937 ) ) ;
#4344 = ORIENTED_EDGE ( 'NONE', *, *, #27666, .T. ) ;
#4345 = FACE_OUTER_BOUND ( 'NONE', #102561, .T. ) ;
#4346 = CIRCLE ( 'NONE', #123497, 0.1000000000000002554 ) ;
#4347 = DIRECTION ( 'NONE',  ( 0.000000000000000000, 1.000000000000000000, 0.000000000000000000 ) ) ;
#4348 = CARTESIAN_POINT ( 'NONE',  ( 8.749999999999918288, 2.500000000000000000, -1.372243186433550033 ) ) ;
#4349 = CIRCLE ( 'NONE', #75475, 0.1000000000000002554 ) ;
#4350 = CARTESIAN_POINT ( 'NONE',  ( 186.2395833340161460, 4.445597072760117285, 7.699999999999999289 ) ) ;
#4351 = VERTEX_POINT ( 'NONE', #36552 ) ;
#4352 = DIRECTION ( 'NONE',  ( 0.000000000000000000, -0.9999939076577903929, 0.003490651415223739937 ) ) ;
#4353 = EDGE_CURVE ( 'NONE', #96180, #83282, #14190, .T. ) ;
#4354 = ORIENTED_EDGE ( 'NONE', *, *, #267, .F. ) ;
#4355 = DIRECTION ( 'NONE',  ( 0.000000000000000000, -0.9999939076577903929, 0.003490651415223739937 ) ) ;
#4356 = EDGE_CURVE ( 'NONE', #94541, #32372, #37210, .T. ) ;
#4357 = EDGE_LOOP ( 'NONE', ( #61401, #44400, #67231, #106963 ) ) ;
#4358 = EDGE_CURVE ( 'NONE', #76656, #82327, #70642, .T. ) ;
#4359 = EDGE_LOOP ( 'NONE', ( #62859, #24151, #94788, #123351 ) ) ;
#4360 = CARTESIAN_POINT ( 'NONE',  ( 6.249999999999932498, 2.500000000000000000, -5.802370205355749988 ) ) ;
#4361 = CARTESIAN_POINT ( 'NONE',  ( -1.250000000000035749, 12.50000000000000000, -7.188010851410854052 ) ) ;
#4362 = FACE_OUTER_BOUND ( 'NONE', #11896, .T. ) ;
#4363 = DIRECTION ( 'NONE',  ( 0.000000000000000000, 0.000000000000000000, 1.000000000000000000 ) ) ;
#4364 = CARTESIAN_POINT ( 'NONE',  ( 184.5000000000000000, -2.986254062820097310, -7.097343634930640022 ) ) ;
#4365 = ORIENTED_EDGE ( 'NONE', *, *, #44552, .F. ) ;
#4366 = EDGE_CURVE ( 'NONE', #122261, #70779, #49735, .T. ) ;
#4367 = VERTEX_POINT ( 'NONE', #95456 ) ;
#4368 = DIRECTION ( 'NONE',  ( -0.000000000000000000, -1.000000000000000000, -0.000000000000000000 ) ) ;
#4369 = B_SPLINE_CURVE_WITH_KNOTS ( 'NONE', 3,
 ( #24216, #111960, #44489, #71361 ),
 .UNSPECIFIED., .F., .F.,
 ( 4, 4 ),
 ( 0.001845843513054588620, 0.003313552284081257640 ),
 .UNSPECIFIED. ) ;
#4370 = DIRECTION ( 'NONE',  ( 0.000000000000000000, 0.000000000000000000, 1.000000000000000000 ) ) ;
#4372 = CARTESIAN_POINT ( 'NONE',  ( -7.300000000000014921, 2.500000000000000000, 4.776537180435972196 ) ) ;
#4371 = CIRCLE ( 'NONE', #108852, 0.1000000000000002554 ) ;
#4373 = EDGE_LOOP ( 'NONE', ( #80647, #126471 ) ) ;
#4374 = EDGE_LOOP ( 'NONE', ( #94410, #100301, #71815, #118820 ) ) ;
#4375 = AXIS2_PLACEMENT_3D ( 'NONE', #64314, #73480, #83942 ) ;
#4376 = CARTESIAN_POINT ( 'NONE',  ( -8.550000000000013145, 12.50000000000000000, -1.818653347947326138 ) ) ;
#4377 = EDGE_LOOP ( 'NONE', ( #124922, #73462, #112230, #106261 ) ) ;
#4378 = PLANE ( 'NONE',  #62505 ) ;
#4379 = CIRCLE ( 'NONE', #83820, 0.06509327318403745899 ) ;
#4380 = DIRECTION ( 'NONE',  ( 0.000000000000000000, -0.9999939076577903929, 0.003490651415223739937 ) ) ;
#4381 = VERTEX_POINT ( 'NONE', #85626 ) ;
#4382 = DIRECTION ( 'NONE',  ( -0.000000000000000000, -1.000000000000000000, -0.000000000000000000 ) ) ;
#4383 = DIRECTION ( 'NONE',  ( 0.000000000000000000, 0.000000000000000000, -1.000000000000000000 ) ) ;
#4384 = DIRECTION ( 'NONE',  ( 0.000000000000000000, 1.000000000000000000, 0.000000000000000000 ) ) ;
#4385 = AXIS2_PLACEMENT_3D ( 'NONE', #8252, #48188, #108392 ) ;
#4386 = ADVANCED_FACE ( 'NONE', ( #77106 ), #99900, .T. ) ;
#4387 = CARTESIAN_POINT ( 'NONE',  ( 1.449999999999951328, 12.50000000000000000, -1.818653347947326138 ) ) ;
#4388 = ORIENTED_EDGE ( 'NONE', *, *, #32501, .T. ) ;
#4389 = DIRECTION ( 'NONE',  ( 0.000000000000000000, -0.9999939076577903929, 0.003490651415223739937 ) ) ;
#4390 = CARTESIAN_POINT ( 'NONE',  ( 65.40763333624980191, -3.109051995112019906, 5.794606894455887058 ) ) ;
#4391 = VERTEX_POINT ( 'NONE', #102216 ) ;
#4392 = ORIENTED_EDGE ( 'NONE', *, *, #30655, .T. ) ;
#4393 = CARTESIAN_POINT ( 'NONE',  ( 184.4218750003414016, 0.000000000000000000, 7.564683531250000925 ) ) ;
#4394 = DIRECTION ( 'NONE',  ( 0.000000000000000000, 0.000000000000000000, 1.000000000000000000 ) ) ;
#4395 = DIRECTION ( 'NONE',  ( 0.000000000000000000, 1.000000000000000000, 0.000000000000000000 ) ) ;
#4396 = CARTESIAN_POINT ( 'NONE',  ( 12.09999999999990550, 12.50000000000000000, -4.330127018922201643 ) ) ;
#4397 = CARTESIAN_POINT ( 'NONE',  ( -13.94999999999998685, 12.50000000000000000, 1.818653347947325472 ) ) ;
#4398 = CIRCLE ( 'NONE', #88025, 0.09999999999999982514 ) ;
#4399 = CARTESIAN_POINT ( 'NONE',  ( -10.40000000000000213, 12.50000000000000000, 3.702399969078682407 ) ) ;
#4401 = EDGE_CURVE ( 'NONE', #87296, #124884, #53919, .T. ) ;
#4400 = CARTESIAN_POINT ( 'NONE',  ( 12.29999999999990479, 2.500000000000000000, 4.576537180435972019 ) ) ;
#4402 = CARTESIAN_POINT ( 'NONE',  ( 10.59999999999990905, 2.500000000000000000, -3.983716857408426293 ) ) ;
#4403 = DIRECTION ( 'NONE',  ( 0.000000000000000000, 0.000000000000000000, 1.000000000000000000 ) ) ;
#4404 = DIRECTION ( 'NONE',  ( 0.000000000000000000, 0.000000000000000000, 1.000000000000000000 ) ) ;
#4405 = DIRECTION ( 'NONE',  ( -4.274815082592931898E-19, -0.9999939076577903929, -0.003490651415223739937 ) ) ;
#4406 = VECTOR ( 'NONE', #106028, 1000.000000000000000 ) ;
#4407 = ORIENTED_EDGE ( 'NONE', *, *, #79092, .T. ) ;
#4409 = VERTEX_POINT ( 'NONE', #32842 ) ;
#4408 = CIRCLE ( 'NONE', #31544, 0.06509327318403745899 ) ;
#4410 = ORIENTED_EDGE ( 'NONE', *, *, #94442, .F. ) ;
#4411 = ORIENTED_EDGE ( 'NONE', *, *, #18673, .T. ) ;
#4412 = EDGE_CURVE ( 'NONE', #107061, #31226, #23009, .T. ) ;
#4413 = DIRECTION ( 'NONE',  ( 0.000000000000000000, 0.000000000000000000, 1.000000000000000000 ) ) ;
#4414 = DIRECTION ( 'NONE',  ( 0.000000000000000000, 0.000000000000000000, 1.000000000000000000 ) ) ;
#4415 = LINE ( 'NONE', #5082, #75018 ) ;
#4416 = AXIS2_PLACEMENT_3D ( 'NONE', #70271, #70916, #51295 ) ;
#4417 = CIRCLE ( 'NONE', #115138, 0.06509327318403745899 ) ;
#4418 = ORIENTED_EDGE ( 'NONE', *, *, #4158, .F. ) ;
#4419 = CARTESIAN_POINT ( 'NONE',  ( -17.50000000000000000, -1.500000000000000000, -8.999999999999998224 ) ) ;
#4420 = FACE_OUTER_BOUND ( 'NONE', #61689, .T. ) ;
#4422 = ORIENTED_EDGE ( 'NONE', *, *, #22963, .T. ) ;
#4421 = CARTESIAN_POINT ( 'NONE',  ( -8.950000000000008171, 12.50000000000000000, 1.818653347947321475 ) ) ;
#4423 = CARTESIAN_POINT ( 'NONE',  ( 10.19999999999991225, 2.500000000000000000, 4.083716857408420609 ) ) ;
#4424 = LINE ( 'NONE', #26679, #35381 ) ;
#4425 = EDGE_LOOP ( 'NONE', ( #5466, #113025, #26453, #60792 ) ) ;
#4426 = VECTOR ( 'NONE', #42170, 1000.000000000000000 ) ;
#4427 = ORIENTED_EDGE ( 'NONE', *, *, #108363, .T. ) ;
#4428 = EDGE_LOOP ( 'NONE', ( #103505, #74131, #27819, #29604 ) ) ;
#4429 = ORIENTED_EDGE ( 'NONE', *, *, #23159, .F. ) ;
#4430 = CARTESIAN_POINT ( 'NONE',  ( -1.250000000000035749, 2.500000000000000000, -7.188010851410854052 ) ) ;
#4431 = AXIS2_PLACEMENT_3D ( 'NONE', #21389, #120880, #22058 ) ;
#4432 = DIRECTION ( 'NONE',  ( 0.000000000000000000, -0.9999939076577903929, 0.003490651415223739937 ) ) ;
#4433 = CARTESIAN_POINT ( 'NONE',  ( 5.649999999999936406, 12.50000000000000000, -6.148780366869526226 ) ) ;
#4434 = LINE ( 'NONE', #77079, #45737 ) ;
#4435 = VERTEX_POINT ( 'NONE', #79673 ) ;
#4436 = EDGE_CURVE ( 'NONE', #30658, #112113, #41423, .T. ) ;
#4437 = CIRCLE ( 'NONE', #104796, 0.1000000000000002554 ) ;
#4438 = AXIS2_PLACEMENT_3D ( 'NONE', #114995, #43085, #123532 ) ;
#4439 = DIRECTION ( 'NONE',  ( 0.000000000000000000, 0.000000000000000000, 1.000000000000000000 ) ) ;
#4440 = VERTEX_POINT ( 'NONE', #58754 ) ;
#4441 = DIRECTION ( 'NONE',  ( 0.000000000000000000, 0.000000000000000000, -1.000000000000000000 ) ) ;
#4442 = CARTESIAN_POINT ( 'NONE',  ( 11.74779829703483180, -2.500000000000000888, -7.682567037524495213 ) ) ;
#4443 = DIRECTION ( 'NONE',  ( 0.000000000000000000, -0.9999939076577903929, 0.003490651415223739937 ) ) ;
#4444 = CARTESIAN_POINT ( 'NONE',  ( 16.68526679984168481, -0.4774970013447560335, 5.954360761636621646 ) ) ;
#4445 = ADVANCED_FACE ( 'NONE', ( #128140 ), #51876, .T. ) ;
#4446 = ORIENTED_EDGE ( 'NONE', *, *, #105266, .T. ) ;
#4447 = EDGE_LOOP ( 'NONE', ( #6404, #96028, #101084, #37992 ) ) ;
#4448 = EDGE_LOOP ( 'NONE', ( #128476, #119347, #123915, #116100 ) ) ;
#4449 = CARTESIAN_POINT ( 'NONE',  ( 1.699999999999950218, 2.500000000000000000, 4.430127018922196847 ) ) ;
#4450 = LINE ( 'NONE', #65981, #33088 ) ;
#4451 = ADVANCED_FACE ( 'NONE', ( #48942 ), #58118, .T. ) ;
#4452 = EDGE_CURVE ( 'NONE', #17249, #127376, #79052, .T. ) ;
#4453 = CARTESIAN_POINT ( 'NONE',  ( 9.149999999999920419, 12.50000000000000000, -5.802370205355749988 ) ) ;
#4454 = ADVANCED_FACE ( 'NONE', ( #448 ), #34385, .T. ) ;
#4455 = FACE_BOUND ( 'NONE', #48394, .T. ) ;
#4456 = EDGE_CURVE ( 'NONE', #76524, #66544, #15474, .T. ) ;
#4457 = CARTESIAN_POINT ( 'NONE',  ( 1.249999999999988454, 2.500000000000000000, -2.265063509461101798 ) ) ;
#4458 = CARTESIAN_POINT ( 'NONE',  ( -0.4000000000000339950, 12.50000000000000000, 0.6928203230275518099 ) ) ;
#4459 = DIRECTION ( 'NONE',  ( -4.274815082592931898E-19, -0.9999939076577903929, -0.003490651415223739937 ) ) ;
#4460 = ADVANCED_FACE ( 'NONE', ( #120258 ), #48951, .T. ) ;
#4461 = VECTOR ( 'NONE', #124850, 1000.000000000000000 ) ;
#4462 = AXIS2_PLACEMENT_3D ( 'NONE', #60936, #100848, #30214 ) ;
#4464 = AXIS2_PLACEMENT_3D ( 'NONE', #25170, #73622, #55922 ) ;
#4463 = DIRECTION ( 'NONE',  ( 0.000000000000000000, -1.000000000000000000, 0.000000000000000000 ) ) ;
#4465 = ADVANCED_FACE ( 'NONE', ( #39143 ), #99326, .T. ) ;
#4466 = CARTESIAN_POINT ( 'NONE',  ( 11.44999999999991047, 2.500000000000000000, 6.148780366869520009 ) ) ;
#4467 = EDGE_CURVE ( 'NONE', #69479, #8359, #49593, .T. ) ;
#4468 = DIRECTION ( 'NONE',  ( 0.000000000000000000, 0.000000000000000000, -1.000000000000000000 ) ) ;
#4469 = ORIENTED_EDGE ( 'NONE', *, *, #8475, .F. ) ;
#4470 = EDGE_CURVE ( 'NONE', #5985, #58914, #63611, .T. ) ;
#4472 = ADVANCED_FACE ( 'NONE', ( #48288 ), #38490, .T. ) ;
#4471 = AXIS2_PLACEMENT_3D ( 'NONE', #8479, #121031, #48420 ) ;
#4473 = CARTESIAN_POINT ( 'NONE',  ( -2.500000000000030642, 12.50000000000000000, -5.088040615133791356 ) ) ;
#4474 = CONICAL_SURFACE ( 'NONE', #127831, 0.09999999999999999167, 0.003490658503988666988 ) ;
#4475 = ORIENTED_EDGE ( 'NONE', *, *, #80923, .T. ) ;
#4476 = ORIENTED_EDGE ( 'NONE', *, *, #109244, .F. ) ;
#4477 = ORIENTED_EDGE ( 'NONE', *, *, #17053, .T. ) ;
#4478 = ORIENTED_EDGE ( 'NONE', *, *, #106902, .F. ) ;
#4479 = DIRECTION ( 'NONE',  ( -0.000000000000000000, 1.000000000000000000, -0.000000000000000000 ) ) ;
#4480 = FACE_BOUND ( 'NONE', #93709, .T. ) ;
#4481 = EDGE_CURVE ( 'NONE', #127950, #35702, #20116, .T. ) ;
#4482 = FACE_OUTER_BOUND ( 'NONE', #3109, .T. ) ;
#4483 = EDGE_LOOP ( 'NONE', ( #23092, #86846, #75870, #45001 ) ) ;
#4484 = CARTESIAN_POINT ( 'NONE',  ( 26.61818291006873949, 2.722754637269844569, 4.358315985293821804 ) ) ;
#4485 = CARTESIAN_POINT ( 'NONE',  ( -0.4500000000000397571, 2.500000000000000000, -2.065063509461102065 ) ) ;
#4486 = VERTEX_POINT ( 'NONE', #78410 ) ;
#4487 = CARTESIAN_POINT ( 'NONE',  ( -9.600000000000008527, 12.50000000000000000, -2.385244779468109755E-15 ) ) ;
#4488 = DIRECTION ( 'NONE',  ( -0.000000000000000000, 1.000000000000000000, -0.000000000000000000 ) ) ;
#4489 = ORIENTED_EDGE ( 'NONE', *, *, #16331, .T. ) ;
#4490 = DIRECTION ( 'NONE',  ( 0.000000000000000000, 0.000000000000000000, -1.000000000000000000 ) ) ;
#4491 = CARTESIAN_POINT ( 'NONE',  ( -11.89999999999999680, 12.50000000000000000, -0.3464101615137741841 ) ) ;
#4492 = CONICAL_SURFACE ( 'NONE', #8712, 0.1000000000000002554, 0.003490658503988666988 ) ;
#4493 = VECTOR ( 'NONE', #89266, 1000.000000000000000 ) ;
#4494 = VERTEX_POINT ( 'NONE', #10296 ) ;
#4495 = CARTESIAN_POINT ( 'NONE',  ( 10.64999999999991331, 12.50000000000000000, -2.446380397790840266 ) ) ;
#4496 = LINE ( 'NONE', #14332, #60292 ) ;
#4497 = CARTESIAN_POINT ( 'NONE',  ( -11.44999999999999751, 2.500000000000000000, -6.841600689897074261 ) ) ;
#4498 = ORIENTED_EDGE ( 'NONE', *, *, #2129, .T. ) ;
#4499 = EDGE_LOOP ( 'NONE', ( #90852, #12131, #12803, #72787 ) ) ;
#4500 = CARTESIAN_POINT ( 'NONE',  ( -8.749999999999976907, 2.500000000000000000, -6.595190528383296780 ) ) ;
#4501 = AXIS2_PLACEMENT_3D ( 'NONE', #53592, #103333, #3206 ) ;
#4502 = ORIENTED_EDGE ( 'NONE', *, *, #58072, .T. ) ;
#4503 = LINE ( 'NONE', #16267, #49168 ) ;
#4504 = AXIS2_PLACEMENT_3D ( 'NONE', #107939, #59519, #58220 ) ;
#4505 = DIRECTION ( 'NONE',  ( -0.000000000000000000, -1.000000000000000000, -0.000000000000000000 ) ) ;
#4506 = EDGE_CURVE ( 'NONE', #22468, #124086, #111639, .T. ) ;
#4507 = ORIENTED_EDGE ( 'NONE', *, *, #127729, .T. ) ;
#4508 = AXIS2_PLACEMENT_3D ( 'NONE', #88126, #36505, #126803 ) ;
#4510 = EDGE_CURVE ( 'NONE', #21203, #103425, #94910, .T. ) ;
#4509 = CARTESIAN_POINT ( 'NONE',  ( 8.749999999999918288, 2.500000000000000000, 7.188010851410848723 ) ) ;
#4511 = DIRECTION ( 'NONE',  ( -0.000000000000000000, 1.000000000000000000, -0.000000000000000000 ) ) ;
#4512 = CARTESIAN_POINT ( 'NONE',  ( -8.150000000000009237, 12.50000000000000000, 6.841600689897072485 ) ) ;
#4513 = FACE_OUTER_BOUND ( 'NONE', #3866, .T. ) ;
#4514 = APPLICATION_CONTEXT ( 'automotive_design' ) ;
#4515 = LINE ( 'NONE', #115118, #126781 ) ;
#4516 = CONICAL_SURFACE ( 'NONE', #65165, 0.1000000000000000056, 0.003490658503988666988 ) ;
#4517 = ADVANCED_FACE ( 'NONE', ( #67918 ), #97056, .T. ) ;
#4518 = ORIENTED_EDGE ( 'NONE', *, *, #16702, .F. ) ;
#4519 = PRODUCT_DEFINITION_FORMATION_WITH_SPECIFIED_SOURCE ( 'ANY', '', #111975, .NOT_KNOWN. ) ;
#4520 = VERTEX_POINT ( 'NONE', #7700 ) ;
#4521 = CARTESIAN_POINT ( 'NONE',  ( -3.350000000000029399, 2.500000000000000000, 6.395190528383296602 ) ) ;
#4522 = DIRECTION ( 'NONE',  ( 0.000000000000000000, 0.000000000000000000, 1.000000000000000000 ) ) ;
#4523 = VECTOR ( 'NONE', #413, 1000.000000000000000 ) ;
#4524 = DIRECTION ( 'NONE',  ( -0.000000000000000000, 1.000000000000000000, -0.000000000000000000 ) ) ;
#4526 = ORIENTED_EDGE ( 'NONE', *, *, #24278, .F. ) ;
#4525 = ORIENTED_EDGE ( 'NONE', *, *, #42184, .T. ) ;
#4527 = ORIENTED_EDGE ( 'NONE', *, *, #55775, .F. ) ;
#4528 = FACE_OUTER_BOUND ( 'NONE', #82693, .T. ) ;
#4529 = AXIS2_PLACEMENT_3D ( 'NONE', #76298, #25910, #116205 ) ;
#4530 = DIRECTION ( 'NONE',  ( 0.000000000000000000, 0.000000000000000000, 1.000000000000000000 ) ) ;
#4531 = CARTESIAN_POINT ( 'NONE',  ( -8.950000000000009948, 2.500000000000000000, 2.411473670974873862 ) ) ;
#4532 = DIRECTION ( 'NONE',  ( 0.000000000000000000, 1.000000000000000000, 0.000000000000000000 ) ) ;
#4533 = AXIS2_PLACEMENT_3D ( 'NONE', #69779, #120814, #109716 ) ;
#4534 = CARTESIAN_POINT ( 'NONE',  ( 8.549999999999920774, 2.500000000000000000, -2.611473670974877592 ) ) ;
#4535 = DIRECTION ( 'NONE',  ( 0.000000000000000000, 1.000000000000000000, 0.000000000000000000 ) ) ;
#4536 = CARTESIAN_POINT ( 'NONE',  ( -4.150000000000025224, 2.500000000000000000, 7.088010851410848190 ) ) ;
#4537 = FACE_OUTER_BOUND ( 'NONE', #33821, .T. ) ;
#4538 = DIRECTION ( 'NONE',  ( 0.000000000000000000, 0.000000000000000000, 1.000000000000000000 ) ) ;
#4539 = ORIENTED_EDGE ( 'NONE', *, *, #116485, .T. ) ;
#4540 = DIRECTION ( 'NONE',  ( 0.000000000000000000, 0.000000000000000000, 1.000000000000000000 ) ) ;
#4541 = VERTEX_POINT ( 'NONE', #127499 ) ;
#4542 = ORIENTED_EDGE ( 'NONE', *, *, #105893, .T. ) ;
#4543 = CARTESIAN_POINT ( 'NONE',  ( -2.100000000000033396, 12.50000000000000000, 0.6277270498435120194 ) ) ;
#4544 = CARTESIAN_POINT ( 'NONE',  ( -3.550000000000027356, 12.50000000000000000, 1.753560074763284016 ) ) ;
#4545 = DIRECTION ( 'NONE',  ( -4.274815082592931898E-19, -0.9999939076577903929, -0.003490651415223739937 ) ) ;
#4546 = EDGE_CURVE ( 'NONE', #88432, #17273, #124252, .T. ) ;
#4547 = CARTESIAN_POINT ( 'NONE',  ( -4.550000000000022915, 2.500000000000000000, 2.265063509461097357 ) ) ;
#4548 = FACE_OUTER_BOUND ( 'NONE', #104793, .T. ) ;
#4549 = CARTESIAN_POINT ( 'NONE',  ( 2.899999999999945732, 12.50000000000000000, 0.06509327318403504425 ) ) ;
#4550 = AXIS2_PLACEMENT_3D ( 'NONE', #91590, #12377, #52311 ) ;
#4551 = CARTESIAN_POINT ( 'NONE',  ( 5.199999999999935341, 2.500000000000000000, -0.3464101615137783474 ) ) ;
#4552 = ORIENTED_EDGE ( 'NONE', *, *, #20199, .F. ) ;
#4553 = LINE ( 'NONE', #95555, #20406 ) ;
#4554 = VECTOR ( 'NONE', #9597, 1000.000000000000000 ) ;
#4555 = CIRCLE ( 'NONE', #100721, 0.1000000000000000472 ) ;
#4556 = DIRECTION ( 'NONE',  ( 0.000000000000000000, 0.000000000000000000, 1.000000000000000000 ) ) ;
#4557 = ORIENTED_EDGE ( 'NONE', *, *, #42678, .F. ) ;
#4558 = CIRCLE ( 'NONE', #94463, 3.500000000000000000 ) ;
#4559 = ORIENTED_EDGE ( 'NONE', *, *, #94674, .F. ) ;
#4560 = CIRCLE ( 'NONE', #21312, 0.09999999999999999167 ) ;
#4561 = EDGE_LOOP ( 'NONE', ( #110918, #7485 ) ) ;
#4563 = ADVANCED_FACE ( 'NONE', ( #30598 ), #82411, .T. ) ;
#4562 = VECTOR ( 'NONE', #2272, 1000.000000000000000 ) ;
#4564 = CIRCLE ( 'NONE', #12890, 0.06509327318403745899 ) ;
#4566 = VERTEX_POINT ( 'NONE', #32534 ) ;
#4565 = ADVANCED_FACE ( 'NONE', ( #60697 ), #101174, .T. ) ;
#4567 = CARTESIAN_POINT ( 'NONE',  ( -10.65000000000000213, 2.500000000000000000, 2.511473670974873507 ) ) ;
#4568 = CARTESIAN_POINT ( 'NONE',  ( -6.250000000000021316, 12.50000000000000000, -1.472243186433550122 ) ) ;
#4569 = VECTOR ( 'NONE', #26578, 1000.000000000000000 ) ;
#4570 = CARTESIAN_POINT ( 'NONE',  ( -14.14999999999998792, 2.500000000000000000, 2.957883832488652942 ) ) ;
#4571 = CARTESIAN_POINT ( 'NONE',  ( 3.149999999999946176, 12.50000000000000000, -2.511473670974877948 ) ) ;
#4572 = CARTESIAN_POINT ( 'NONE',  ( -14.34999999999998543, 12.50000000000000000, 2.446380397790839822 ) ) ;
#4573 = ORIENTED_EDGE ( 'NONE', *, *, #29482, .F. ) ;
#4574 = CARTESIAN_POINT ( 'NONE',  ( 76.44859290207541846, -3.583118647509688781, 6.086777568259361004 ) ) ;
#4575 = ADVANCED_FACE ( 'NONE', ( #92062 ), #88648, .T. ) ;
#4576 = PLANE ( 'NONE',  #9702 ) ;
#4577 = DIRECTION ( 'NONE',  ( 0.000000000000000000, 0.000000000000000000, 1.000000000000000000 ) ) ;
#4578 = ORIENTED_EDGE ( 'NONE', *, *, #62783, .T. ) ;
#4579 = ORIENTED_EDGE ( 'NONE', *, *, #81077, .F. ) ;
#4580 = ORIENTED_EDGE ( 'NONE', *, *, #62458, .T. ) ;
#4581 = DIRECTION ( 'NONE',  ( -0.000000000000000000, 1.000000000000000000, -0.000000000000000000 ) ) ;
#4582 = DIRECTION ( 'NONE',  ( -0.000000000000000000, -1.000000000000000000, -0.000000000000000000 ) ) ;
#4583 = AXIS2_PLACEMENT_3D ( 'NONE', #128762, #100554, #61937 ) ;
#4584 = DIRECTION ( 'NONE',  ( 0.000000000000000000, -0.000000000000000000, 1.000000000000000000 ) ) ;
#4585 = VECTOR ( 'NONE', #115990, 1000.000000000000000 ) ;
#4586 = ORIENTED_EDGE ( 'NONE', *, *, #25448, .F. ) ;
#4587 = CARTESIAN_POINT ( 'NONE',  ( -7.950000000000009059, 2.500000000000000000, 6.495190528383297135 ) ) ;
#4588 = CARTESIAN_POINT ( 'NONE',  ( -13.09999999999999254, 12.50000000000000000, -3.918623584224386391 ) ) ;
#4589 = LINE ( 'NONE', #124409, #33746 ) ;
#4590 = DIRECTION ( 'NONE',  ( 0.000000000000000000, -0.000000000000000000, 1.000000000000000000 ) ) ;
#4591 = DIRECTION ( 'NONE',  ( 0.000000000000000000, -0.9999939076577903929, 0.003490651415223739937 ) ) ;
#4592 = AXIS2_PLACEMENT_3D ( 'NONE', #111702, #82250, #72428 ) ;
#4593 = AXIS2_PLACEMENT_3D ( 'NONE', #14046, #33090, #94548 ) ;
#4595 = EDGE_CURVE ( 'NONE', #11368, #63798, #32236, .T. ) ;
#4594 = AXIS2_PLACEMENT_3D ( 'NONE', #95078, #84613, #36809 ) ;
#4596 = ORIENTED_EDGE ( 'NONE', *, *, #117838, .T. ) ;
#4597 = DIRECTION ( 'NONE',  ( -0.000000000000000000, -1.000000000000000000, -0.000000000000000000 ) ) ;
#4598 = CONICAL_SURFACE ( 'NONE', #29685, 0.09999999999999982514, 0.003490658503988666988 ) ;
#4599 = ORIENTED_EDGE ( 'NONE', *, *, #57298, .F. ) ;
#4600 = EDGE_LOOP ( 'NONE', ( #92441, #71078, #11723, #98558, #76871, #216, #64515, #90448, #67535, #43861, #22545, #129524 ) ) ;
#4601 = EDGE_CURVE ( 'NONE', #94495, #109058, #50866, .T. ) ;
#4602 = DIRECTION ( 'NONE',  ( 0.000000000000000000, -1.000000000000000000, 0.000000000000000000 ) ) ;
#4603 = DIRECTION ( 'NONE',  ( 0.000000000000000000, 0.000000000000000000, 1.000000000000000000 ) ) ;
#4604 = EDGE_CURVE ( 'NONE', #117214, #126618, #59430, .T. ) ;
#4605 = DIRECTION ( 'NONE',  ( 0.000000000000000000, 1.000000000000000000, 0.000000000000000000 ) ) ;
#4607 = DIRECTION ( 'NONE',  ( 0.000000000000000000, 0.000000000000000000, 1.000000000000000000 ) ) ;
#4606 = AXIS2_PLACEMENT_3D ( 'NONE', #11399, #90601, #50680 ) ;
#4609 = DIRECTION ( 'NONE',  ( 0.000000000000000000, 0.000000000000000000, 1.000000000000000000 ) ) ;
#4608 = CONICAL_SURFACE ( 'NONE', #117478, 0.09999999999999982514, 0.003490658503988666988 ) ;
#4610 = EDGE_LOOP ( 'NONE', ( #18314, #54305, #72748, #62158 ) ) ;
#4611 = CIRCLE ( 'NONE', #29696, 0.06509327318403745899 ) ;
#4612 = CIRCLE ( 'NONE', #94527, 0.1000000000000002554 ) ;
#4613 = CIRCLE ( 'NONE', #21370, 0.1000000000000000472 ) ;
#4614 = ADVANCED_FACE ( 'NONE', ( #43638 ), #111042, .T. ) ;
#4615 = EDGE_CURVE ( 'NONE', #108499, #29271, #55208, .T. ) ;
#4616 = EDGE_LOOP ( 'NONE', ( #16262, #109759 ) ) ;
#4617 = CARTESIAN_POINT ( 'NONE',  ( -4.999999999999990230, 12.50000000000000000, -4.330127018922201643 ) ) ;
#4618 = CARTESIAN_POINT ( 'NONE',  ( -4.999999999999986677, 2.500000000000000000, -2.276824562219559311E-15 ) ) ;
#4619 = EDGE_CURVE ( 'NONE', #42865, #59695, #81605, .T. ) ;
#4620 = DIRECTION ( 'NONE',  ( -0.000000000000000000, 1.000000000000000000, -0.000000000000000000 ) ) ;
#4621 = AXIS2_PLACEMENT_3D ( 'NONE', #10457, #20931, #8508 ) ;
#4622 = FACE_OUTER_BOUND ( 'NONE', #57006, .T. ) ;
#4623 = VERTEX_POINT ( 'NONE', #111716 ) ;
#4624 = FACE_OUTER_BOUND ( 'NONE', #95766, .T. ) ;
#4625 = EDGE_CURVE ( 'NONE', #128756, #75351, #13419, .T. ) ;
#4626 = CARTESIAN_POINT ( 'NONE',  ( 2.699999999999947331, 2.500000000000000000, -4.776537180435978414 ) ) ;
#4627 = AXIS2_PLACEMENT_3D ( 'NONE', #125573, #63453, #64089 ) ;
#4628 = ORIENTED_EDGE ( 'NONE', *, *, #13066, .F. ) ;
#4629 = DIRECTION ( 'NONE',  ( -0.000000000000000000, -1.000000000000000000, -0.000000000000000000 ) ) ;
#4630 = EDGE_CURVE ( 'NONE', #25435, #109355, #92867, .T. ) ;
#4631 = ORIENTED_EDGE ( 'NONE', *, *, #5367, .F. ) ;
#4632 = EDGE_CURVE ( 'NONE', #61297, #68676, #103323, .T. ) ;
#4633 = LINE ( 'NONE', #15091, #32856 ) ;
#4634 = EDGE_LOOP ( 'NONE', ( #120322, #23997 ) ) ;
#4635 = DIRECTION ( 'NONE',  ( -0.000000000000000000, -1.000000000000000000, -0.000000000000000000 ) ) ;
#4636 = DIRECTION ( 'NONE',  ( -0.000000000000000000, -1.000000000000000000, -0.000000000000000000 ) ) ;
#4637 = ORIENTED_EDGE ( 'NONE', *, *, #82218, .F. ) ;
#4638 = EDGE_LOOP ( 'NONE', ( #73014, #91421 ) ) ;
#4639 = CARTESIAN_POINT ( 'NONE',  ( 186.7552083336747444, 6.551208109652275624, -3.782341765624998686 ) ) ;
#4640 = CARTESIAN_POINT ( 'NONE',  ( 184.9635416670080588, -4.367472073101520635, 7.564683531249999149 ) ) ;
#4641 = DIRECTION ( 'NONE',  ( -0.000000000000000000, 1.000000000000000000, -0.000000000000000000 ) ) ;
#4642 = VECTOR ( 'NONE', #84827, 1000.000000000000000 ) ;
#4643 = DIRECTION ( 'NONE',  ( -4.274815082592931898E-19, -0.9999939076577903929, -0.003490651415223739937 ) ) ;
#4644 = CARTESIAN_POINT ( 'NONE',  ( 9.999999999999914735, 2.500000000000000000, 0.6928203230275494784 ) ) ;
#4645 = AXIS2_PLACEMENT_3D ( 'NONE', #90371, #25496, #2634 ) ;
#4646 = DIRECTION ( 'NONE',  ( 0.000000000000000000, -0.000000000000000000, 1.000000000000000000 ) ) ;
#4647 = DIRECTION ( 'NONE',  ( -0.000000000000000000, -1.000000000000000000, -0.000000000000000000 ) ) ;
#4649 = EDGE_LOOP ( 'NONE', ( #51158, #97507, #43525, #7560 ) ) ;
#4648 = AXIS2_PLACEMENT_3D ( 'NONE', #121639, #22184, #62101 ) ;
#4651 = VERTEX_POINT ( 'NONE', #43007 ) ;
#4650 = VECTOR ( 'NONE', #122417, 1000.000000000000000 ) ;
#4652 = DIRECTION ( 'NONE',  ( -0.000000000000000000, 1.000000000000000000, -0.000000000000000000 ) ) ;
#4653 = DIRECTION ( 'NONE',  ( -4.274815082592931898E-19, -0.9999939076577903929, -0.003490651415223739937 ) ) ;
#4654 = DIRECTION ( 'NONE',  ( 0.000000000000000000, 0.000000000000000000, 1.000000000000000000 ) ) ;
#4655 = CIRCLE ( 'NONE', #50660, 0.06509327318403745899 ) ;
#4656 = DIRECTION ( 'NONE',  ( 0.000000000000000000, 1.000000000000000000, 0.000000000000000000 ) ) ;
#4659 = ORIENTED_EDGE ( 'NONE', *, *, #46653, .T. ) ;
#4658 = ORIENTED_EDGE ( 'NONE', *, *, #50733, .F. ) ;
#4657 = VECTOR ( 'NONE', #67984, 1000.000000000000000 ) ;
#4660 = DIRECTION ( 'NONE',  ( -0.000000000000000000, 1.000000000000000000, -0.000000000000000000 ) ) ;
#4661 = ORIENTED_EDGE ( 'NONE', *, *, #117512, .F. ) ;
#4662 = DIRECTION ( 'NONE',  ( 0.000000000000000000, 0.000000000000000000, -1.000000000000000000 ) ) ;
#4663 = FACE_OUTER_BOUND ( 'NONE', #84560, .T. ) ;
#4664 = AXIS2_PLACEMENT_3D ( 'NONE', #41164, #111821, #111142 ) ;
#4665 = ORIENTED_EDGE ( 'NONE', *, *, #39109, .F. ) ;
#4666 = FACE_OUTER_BOUND ( 'NONE', #91228, .T. ) ;
#4667 = LINE ( 'NONE', #104809, #41091 ) ;
#4668 = EDGE_CURVE ( 'NONE', #78495, #77492, #109587, .T. ) ;
#4669 = DIRECTION ( 'NONE',  ( 0.000000000000000000, 0.000000000000000000, 1.000000000000000000 ) ) ;
#4670 = CARTESIAN_POINT ( 'NONE',  ( -7.900000000000014566, 12.50000000000000000, -3.637306695894650055 ) ) ;
#4672 = EDGE_CURVE ( 'NONE', #63967, #95786, #5009, .T. ) ;
#4671 = DIRECTION ( 'NONE',  ( -0.000000000000000000, -1.000000000000000000, -0.000000000000000000 ) ) ;
#4673 = DIRECTION ( 'NONE',  ( 0.000000000000000000, 0.000000000000000000, -1.000000000000000000 ) ) ;
#4674 = CARTESIAN_POINT ( 'NONE',  ( 185.8177083336747160, 4.367472073101515306, 7.564683531250000925 ) ) ;
#4675 = CARTESIAN_POINT ( 'NONE',  ( 13.34999999999990017, 2.500000000000000000, 2.265063509461097357 ) ) ;
#4676 = CARTESIAN_POINT ( 'NONE',  ( -8.750000000000010658, 12.50000000000000000, -7.188010851410848723 ) ) ;
#4677 = CIRCLE ( 'NONE', #111292, 0.1000000000000002554 ) ;
#4678 = ORIENTED_EDGE ( 'NONE', *, *, #24025, .T. ) ;
#4679 = ORIENTED_EDGE ( 'NONE', *, *, #58409, .F. ) ;
#4680 = VERTEX_POINT ( 'NONE', #63255 ) ;
#4681 = CARTESIAN_POINT ( 'NONE',  ( -11.64999999999999680, 2.500000000000000000, -2.065063509461098068 ) ) ;
#4682 = VERTEX_POINT ( 'NONE', #100592 ) ;
#4683 = LINE ( 'NONE', #51421, #68647 ) ;
#4685 = EDGE_LOOP ( 'NONE', ( #106222, #124078, #127461, #68182 ) ) ;
#4684 = ORIENTED_EDGE ( 'NONE', *, *, #71147, .T. ) ;
#4686 = ORIENTED_EDGE ( 'NONE', *, *, #122295, .F. ) ;
#4687 = DIRECTION ( 'NONE',  ( 0.000000000000000000, 0.000000000000000000, 1.000000000000000000 ) ) ;
#4688 = VECTOR ( 'NONE', #28459, 1000.000000000000000 ) ;
#4689 = CONICAL_SURFACE ( 'NONE', #73748, 0.1000000000000002554, 0.003490658503988666988 ) ;
#4690 = DIRECTION ( 'NONE',  ( -0.000000000000000000, 1.000000000000000000, -0.000000000000000000 ) ) ;
#4691 = SHAPE_REPRESENTATION_RELATIONSHIP ( 'NONE' , 'NONE' ,  #107120, #21197 ) ;
#4692 = CARTESIAN_POINT ( 'NONE',  ( -0.6500000000000389910, 12.50000000000000000, -1.818653347947326138 ) ) ;
#4693 = CARTESIAN_POINT ( 'NONE',  ( 7.299999999999926104, 2.500000000000000000, -3.983716857408426293 ) ) ;
#4694 = CARTESIAN_POINT ( 'NONE',  ( 8.349999999999923261, 2.500000000000000000, -7.288010851410854585 ) ) ;
#4695 = ORIENTED_EDGE ( 'NONE', *, *, #111015, .F. ) ;
#4696 = AXIS2_PLACEMENT_3D ( 'NONE', #48123, #117458, #69685 ) ;
#4697 = AXIS2_PLACEMENT_3D ( 'NONE', #17254, #18581, #76220 ) ;
#4698 = DIRECTION ( 'NONE',  ( 0.000000000000000000, -0.9999939076577903929, 0.003490651415223739937 ) ) ;
#4699 = ORIENTED_EDGE ( 'NONE', *, *, #9854, .F. ) ;
#4700 = CONICAL_SURFACE ( 'NONE', #86176, 0.1000000000000000472, 0.003490658503988666988 ) ;
#4701 = EDGE_LOOP ( 'NONE', ( #71112, #71264 ) ) ;
#4702 = AXIS2_PLACEMENT_3D ( 'NONE', #52586, #2187, #82038 ) ;
#4703 = ORIENTED_EDGE ( 'NONE', *, *, #8700, .F. ) ;
#4704 = FACE_OUTER_BOUND ( 'NONE', #115315, .T. ) ;
#4705 = EDGE_LOOP ( 'NONE', ( #103666, #45245, #41718, #89039 ) ) ;
#4706 = ORIENTED_EDGE ( 'NONE', *, *, #120180, .F. ) ;
#4707 = VERTEX_POINT ( 'NONE', #33176 ) ;
#4708 = CIRCLE ( 'NONE', #56938, 0.1000000000000002554 ) ;
#4709 = FACE_OUTER_BOUND ( 'NONE', #20776, .T. ) ;
#4710 = CIRCLE ( 'NONE', #44448, 0.06509327318403745899 ) ;
#4711 = EDGE_CURVE ( 'NONE', #84112, #70528, #20759, .T. ) ;
#4712 = CARTESIAN_POINT ( 'NONE',  ( 11.89999999999990798, 2.500000000000000000, -3.983716857408426293 ) ) ;
#4713 = FACE_OUTER_BOUND ( 'NONE', #129586, .T. ) ;
#4714 = PLANE ( 'NONE',  #40101 ) ;
#4715 = CARTESIAN_POINT ( 'NONE',  ( 88.00000000000001421, 0.000000000000000000, 0.000000000000000000 ) ) ;
#4716 = VECTOR ( 'NONE', #75249, 1000.000000000000000 ) ;
#4717 = AXIS2_PLACEMENT_3D ( 'NONE', #74578, #104043, #5817 ) ;
#4718 = DIRECTION ( 'NONE',  ( 0.000000000000000000, 1.000000000000000000, 0.000000000000000000 ) ) ;
#4719 = ORIENTED_EDGE ( 'NONE', *, *, #127592, .F. ) ;
#4720 = AXIS2_PLACEMENT_3D ( 'NONE', #84991, #16866, #126216 ) ;
#4721 = DIRECTION ( 'NONE',  ( 0.000000000000000000, 1.000000000000000000, 0.000000000000000000 ) ) ;
#4722 = ADVANCED_FACE ( 'NONE', ( #52154 ), #44839, .T. ) ;
#4723 = ORIENTED_EDGE ( 'NONE', *, *, #110924, .T. ) ;
#4724 = CARTESIAN_POINT ( 'NONE',  ( -8.550000000000013145, 2.500000000000000000, -6.741600689897072840 ) ) ;
#4725 = EDGE_LOOP ( 'NONE', ( #81455, #30356, #1503, #107931 ) ) ;
#4726 = CONICAL_SURFACE ( 'NONE', #94620, 0.1000000000000000472, 0.003490658503988666988 ) ;
#4727 = DIRECTION ( 'NONE',  ( 0.000000000000000000, 0.000000000000000000, 1.000000000000000000 ) ) ;
#4728 = VERTEX_POINT ( 'NONE', #41069 ) ;
#4729 = ADVANCED_FACE ( 'NONE', ( #80972 ), #103833, .T. ) ;
#4730 = ADVANCED_FACE ( 'NONE', ( #126028 ), #84822, .T. ) ;
#4731 = ORIENTED_EDGE ( 'NONE', *, *, #64270, .F. ) ;
#4732 = CARTESIAN_POINT ( 'NONE',  ( 4.349999999999941025, 12.50000000000000000, -1.753560074763288679 ) ) ;
#4733 = FACE_OUTER_BOUND ( 'NONE', #31963, .T. ) ;
#4734 = EDGE_CURVE ( 'NONE', #6533, #120460, #86093, .T. ) ;
#4735 = FACE_OUTER_BOUND ( 'NONE', #104955, .T. ) ;
#4736 = VERTEX_POINT ( 'NONE', #95299 ) ;
#4737 = CARTESIAN_POINT ( 'NONE',  ( 10.84999999999991260, 12.50000000000000000, 5.802370205355744659 ) ) ;
#4738 = ORIENTED_EDGE ( 'NONE', *, *, #120504, .T. ) ;
#4739 = CARTESIAN_POINT ( 'NONE',  ( 3.749999999999944045, 12.50000000000000000, -2.857883832488653741 ) ) ;
#4740 = CARTESIAN_POINT ( 'NONE',  ( 0.5999999999999547917, 2.500000000000000000, 4.083716857408420609 ) ) ;
#4741 = VECTOR ( 'NONE', #45831, 1000.000000000000000 ) ;
#4742 = EDGE_CURVE ( 'NONE', #63146, #33567, #120048, .T. ) ;
#4743 = DIRECTION ( 'NONE',  ( 0.000000000000000000, -0.000000000000000000, 1.000000000000000000 ) ) ;
#4744 = CARTESIAN_POINT ( 'NONE',  ( 17.50000000000000000, -2.500000000000000000, 2.922290670089274567 ) ) ;
#4745 = CARTESIAN_POINT ( 'NONE',  ( -9.400000000000007461, 12.50000000000000000, 3.983716857408420076 ) ) ;
#4746 = ORIENTED_EDGE ( 'NONE', *, *, #87661, .F. ) ;
#4747 = CIRCLE ( 'NONE', #77918, 0.06509327318403745899 ) ;
#4748 = EDGE_LOOP ( 'NONE', ( #55917, #32994 ) ) ;
#4749 = CIRCLE ( 'NONE', #92503, 0.1000000000000002554 ) ;
#4750 = CONICAL_SURFACE ( 'NONE', #23548, 0.1000000000000002554, 0.003490658503988666988 ) ;
#4751 = ORIENTED_EDGE ( 'NONE', *, *, #39669, .T. ) ;
#4752 = DIRECTION ( 'NONE',  ( -0.000000000000000000, -1.000000000000000000, -0.000000000000000000 ) ) ;
#4753 = CARTESIAN_POINT ( 'NONE',  ( 11.24999999999991118, 12.50000000000000000, -2.792790559304616504 ) ) ;
#4754 = AXIS2_PLACEMENT_3D ( 'NONE', #77823, #118400, #59518 ) ;
#4755 = CIRCLE ( 'NONE', #77927, 0.1000000000000002554 ) ;
#4756 = CIRCLE ( 'NONE', #71679, 0.1000000000000002554 ) ;
#4757 = AXIS2_PLACEMENT_3D ( 'NONE', #5819, #123210, #86973 ) ;
#4758 = CIRCLE ( 'NONE', #103078, 0.1000000000000000472 ) ;
#4759 = CARTESIAN_POINT ( 'NONE',  ( 185.9218750003414016, 0.000000000000000000, 7.564683531250000925 ) ) ;
#4760 = LINE ( 'NONE', #125205, #28133 ) ;
#4761 = LINE ( 'NONE', #104276, #113377 ) ;
#4762 = DIRECTION ( 'NONE',  ( 0.000000000000000000, 0.000000000000000000, 1.000000000000000000 ) ) ;
#4763 = CARTESIAN_POINT ( 'NONE',  ( 8.099999999999923261, 12.50000000000000000, 4.048810130592458201 ) ) ;
#4764 = ORIENTED_EDGE ( 'NONE', *, *, #45432, .T. ) ;
#4765 = DIRECTION ( 'NONE',  ( 0.000000000000000000, 1.000000000000000000, 0.000000000000000000 ) ) ;
#4766 = EDGE_CURVE ( 'NONE', #16720, #68464, #28104, .T. ) ;
#4767 = DIRECTION ( 'NONE',  ( 0.000000000000000000, 0.000000000000000000, -1.000000000000000000 ) ) ;
#4768 = CARTESIAN_POINT ( 'NONE',  ( 14.34999999999989662, 2.500000000000000000, 2.511473670974873507 ) ) ;
#4769 = ORIENTED_EDGE ( 'NONE', *, *, #64059, .T. ) ;
#4770 = EDGE_CURVE ( 'NONE', #33245, #78150, #44746, .T. ) ;
#4771 = EDGE_CURVE ( 'NONE', #86814, #39666, #78196, .T. ) ;
#4772 = CARTESIAN_POINT ( 'NONE',  ( 15.59999999999988951, 2.500000000000000000, -0.3464101615137783474 ) ) ;
#4773 = AXIS2_PLACEMENT_3D ( 'NONE', #110879, #61808, #49413 ) ;
#4774 = EDGE_LOOP ( 'NONE', ( #65861, #105035, #118796, #52460 ) ) ;
#4775 = FACE_OUTER_BOUND ( 'NONE', #110979, .T. ) ;
#4776 = EDGE_CURVE ( 'NONE', #41506, #61373, #118070, .T. ) ;
#4777 = EDGE_CURVE ( 'NONE', #55365, #93720, #14766, .T. ) ;
#4778 = VERTEX_POINT ( 'NONE', #94005 ) ;
#4779 = DIRECTION ( 'NONE',  ( 0.000000000000000000, 0.000000000000000000, 1.000000000000000000 ) ) ;
#4780 = LINE ( 'NONE', #3519, #27875 ) ;
#4781 = EDGE_CURVE ( 'NONE', #117938, #45123, #26049, .T. ) ;
#4782 = DIRECTION ( 'NONE',  ( 0.000000000000000000, 0.000000000000000000, -1.000000000000000000 ) ) ;
#4783 = ADVANCED_FACE ( 'NONE', ( #35107 ), #111722, .T. ) ;
#4784 = CIRCLE ( 'NONE', #8996, 0.1000000000000002554 ) ;
#4785 = ORIENTED_EDGE ( 'NONE', *, *, #97404, .F. ) ;
#4786 = CIRCLE ( 'NONE', #59101, 0.09999999999999982514 ) ;
#4787 = AXIS2_PLACEMENT_3D ( 'NONE', #70053, #117839, #107393 ) ;
#4788 = CARTESIAN_POINT ( 'NONE',  ( 185.6562500006828031, 8.891194145520236347, 5.444286225454521982E-16 ) ) ;
#4789 = EDGE_CURVE ( 'NONE', #117945, #125498, #24629, .T. ) ;
#4790 = CARTESIAN_POINT ( 'NONE',  ( -11.89999999999999680, 12.50000000000000000, 0.3464101615137776813 ) ) ;
#4791 = AXIS2_PLACEMENT_3D ( 'NONE', #98180, #18968, #70025 ) ;
#4792 = VERTEX_POINT ( 'NONE', #85472 ) ;
#4793 = AXIS2_PLACEMENT_3D ( 'NONE', #49680, #18896, #69948 ) ;
#4794 = EDGE_CURVE ( 'NONE', #85654, #29791, #92958, .T. ) ;
#4795 = DIRECTION ( 'NONE',  ( -0.000000000000000000, -1.000000000000000000, -0.000000000000000000 ) ) ;
#4796 = AXIS2_PLACEMENT_3D ( 'NONE', #57675, #27539, #36101 ) ;
#4797 = EDGE_CURVE ( 'NONE', #52060, #112457, #55294, .T. ) ;
#4798 = VERTEX_POINT ( 'NONE', #114919 ) ;
#4799 = ORIENTED_EDGE ( 'NONE', *, *, #120226, .T. ) ;
#4800 = CARTESIAN_POINT ( 'NONE',  ( -8.150000000000012790, 2.500000000000000000, 2.511473670974873507 ) ) ;
#4801 = DIRECTION ( 'NONE',  ( 0.000000000000000000, -0.000000000000000000, 1.000000000000000000 ) ) ;
#4802 = VERTEX_POINT ( 'NONE', #25244 ) ;
#4803 = DIRECTION ( 'NONE',  ( 0.000000000000000000, 0.000000000000000000, 1.000000000000000000 ) ) ;
#4804 = DIRECTION ( 'NONE',  ( 0.000000000000000000, 0.000000000000000000, 1.000000000000000000 ) ) ;
#4805 = CIRCLE ( 'NONE', #17316, 0.06509327318403745899 ) ;
#4806 = VERTEX_POINT ( 'NONE', #115555 ) ;
#4807 = CARTESIAN_POINT ( 'NONE',  ( -13.14999999999999147, 12.50000000000000000, -2.446380397790838046 ) ) ;
#4808 = CARTESIAN_POINT ( 'NONE',  ( 6.649999999999930189, 12.50000000000000000, -1.407149913249512663 ) ) ;
#4809 = AXIS2_PLACEMENT_3D ( 'NONE', #78905, #68409, #118804 ) ;
#4810 = AXIS2_PLACEMENT_3D ( 'NONE', #81539, #102467, #109208 ) ;
#4811 = CIRCLE ( 'NONE', #96852, 0.06509327318403745899 ) ;
#4812 = DIRECTION ( 'NONE',  ( 0.000000000000000000, 1.000000000000000000, 0.000000000000000000 ) ) ;
#4813 = FACE_OUTER_BOUND ( 'NONE', #26377, .T. ) ;
#4814 = DIRECTION ( 'NONE',  ( 0.000000000000000000, 0.000000000000000000, 1.000000000000000000 ) ) ;
#4815 = FACE_OUTER_BOUND ( 'NONE', #57206, .T. ) ;
#4816 = AXIS2_PLACEMENT_3D ( 'NONE', #84844, #57326, #126051 ) ;
#4817 = DIRECTION ( 'NONE',  ( 0.000000000000000000, 0.000000000000000000, 1.000000000000000000 ) ) ;
#4818 = ORIENTED_EDGE ( 'NONE', *, *, #84146, .F. ) ;
#4819 = CIRCLE ( 'NONE', #71749, 0.06509327318403745899 ) ;
#4820 = ORIENTED_EDGE ( 'NONE', *, *, #326, .T. ) ;
#4821 = ORIENTED_EDGE ( 'NONE', *, *, #40578, .T. ) ;
#4822 = ORIENTED_EDGE ( 'NONE', *, *, #52211, .F. ) ;
#4823 = CARTESIAN_POINT ( 'NONE',  ( 129.5000000000000000, 0.000000000000000000, -6.000000000000000000 ) ) ;
#4824 = DIRECTION ( 'NONE',  ( -0.000000000000000000, -1.000000000000000000, -0.000000000000000000 ) ) ;
#4825 = DIRECTION ( 'NONE',  ( 0.000000000000000000, -0.000000000000000000, 1.000000000000000000 ) ) ;
#4826 = VERTEX_POINT ( 'NONE', #65163 ) ;
#4827 = FACE_BOUND ( 'NONE', #40551, .T. ) ;
#4828 = DIRECTION ( 'NONE',  ( 0.000000000000000000, 0.000000000000000000, 1.000000000000000000 ) ) ;
#4829 = DIRECTION ( 'NONE',  ( 0.000000000000000000, 0.000000000000000000, 1.000000000000000000 ) ) ;
#4830 = DIRECTION ( 'NONE',  ( 0.000000000000000000, 1.000000000000000000, 0.000000000000000000 ) ) ;
#4831 = ADVANCED_FACE ( 'NONE', ( #64540 ), #5102, .T. ) ;
#4832 = FACE_OUTER_BOUND ( 'NONE', #58745, .T. ) ;
#4833 = CARTESIAN_POINT ( 'NONE',  ( 3.349999999999945466, 2.500000000000000000, -6.495190528383302464 ) ) ;
#4834 = CARTESIAN_POINT ( 'NONE',  ( 13.54999999999990123, 12.50000000000000000, 1.818653347947321475 ) ) ;
#4835 = CARTESIAN_POINT ( 'NONE',  ( 3.549999999999940314, 2.500000000000000000, 6.941600689897073018 ) ) ;
#4836 = DIRECTION ( 'NONE',  ( 0.000000000000000000, 1.000000000000000000, 0.000000000000000000 ) ) ;
#4837 = AXIS2_PLACEMENT_3D ( 'NONE', #119672, #28735, #68643 ) ;
#4838 = VECTOR ( 'NONE', #37079, 1000.000000000000000 ) ;
#4839 = CARTESIAN_POINT ( 'NONE',  ( 5.799999999999933209, 12.50000000000000000, -0.06509327318403980434 ) ) ;
#4840 = CARTESIAN_POINT ( 'NONE',  ( -13.14999999999999147, 2.500000000000000000, -1.818653347947323917 ) ) ;
#4841 = EDGE_CURVE ( 'NONE', #62185, #4982, #56001, .T. ) ;
#4842 = AXIS2_PLACEMENT_3D ( 'NONE', #77547, #98466, #127314 ) ;
#4843 = EDGE_LOOP ( 'NONE', ( #38595, #62513, #109993, #82465 ) ) ;
#4844 = ORIENTED_EDGE ( 'NONE', *, *, #73202, .T. ) ;
#4845 = ORIENTED_EDGE ( 'NONE', *, *, #56074, .T. ) ;
#4846 = AXIS2_PLACEMENT_3D ( 'NONE', #39943, #10463, #50390 ) ;
#4847 = ORIENTED_EDGE ( 'NONE', *, *, #69909, .T. ) ;
#4849 = CIRCLE ( 'NONE', #19425, 0.1000000000000000472 ) ;
#4848 = CARTESIAN_POINT ( 'NONE',  ( 1.249999999999986899, 2.500000000000000000, 6.495190528383297135 ) ) ;
#4850 = EDGE_LOOP ( 'NONE', ( #77696, #30667, #110011, #113770 ) ) ;
#4851 = CIRCLE ( 'NONE', #90541, 0.06509327318403745899 ) ;
#4852 = LINE ( 'NONE', #83445, #31886 ) ;
#4853 = ORIENTED_EDGE ( 'NONE', *, *, #18506, .T. ) ;
#4854 = ORIENTED_EDGE ( 'NONE', *, *, #85888, .T. ) ;
#4855 = AXIS2_PLACEMENT_3D ( 'NONE', #109214, #66713, #7142 ) ;
#4856 = AXIS2_PLACEMENT_3D ( 'NONE', #34580, #115035, #106515 ) ;
#4857 = AXIS2_PLACEMENT_3D ( 'NONE', #48732, #29101, #89923 ) ;
#4858 = CARTESIAN_POINT ( 'NONE',  ( 3.677269697637739476, -2.500000000000000444, 8.999999999915248239 ) ) ;
#4859 = LINE ( 'NONE', #64433, #58347 ) ;
#4860 = CARTESIAN_POINT ( 'NONE',  ( -3.350000000000029399, 2.500000000000000000, 6.495190528383297135 ) ) ;
#4861 = DIRECTION ( 'NONE',  ( 0.000000000000000000, 0.000000000000000000, 1.000000000000000000 ) ) ;
#4862 = AXIS2_PLACEMENT_3D ( 'NONE', #105529, #33575, #44036 ) ;
#4863 = EDGE_LOOP ( 'NONE', ( #114614, #58454, #20937, #19980 ) ) ;
#4864 = CIRCLE ( 'NONE', #88495, 0.06509327318403745899 ) ;
#4865 = EDGE_LOOP ( 'NONE', ( #65689, #11282 ) ) ;
#4866 = ORIENTED_EDGE ( 'NONE', *, *, #123504, .F. ) ;
#4868 = VERTEX_POINT ( 'NONE', #6244 ) ;
#4867 = CARTESIAN_POINT ( 'NONE',  ( 5.849999999999933031, 2.500000000000000000, -1.572243186433550211 ) ) ;
#4869 = DIRECTION ( 'NONE',  ( 0.000000000000000000, 1.000000000000000000, 0.000000000000000000 ) ) ;
#4870 = EDGE_LOOP ( 'NONE', ( #56891, #63140 ) ) ;
#4871 = EDGE_LOOP ( 'NONE', ( #105938, #82775 ) ) ;
#4872 = DIRECTION ( 'NONE',  ( 0.000000000000000000, 0.000000000000000000, -1.000000000000000000 ) ) ;
#4873 = DIRECTION ( 'NONE',  ( 0.000000000000000000, 0.000000000000000000, 1.000000000000000000 ) ) ;
#4874 = CARTESIAN_POINT ( 'NONE',  ( -11.24999999999996270, 12.50000000000000000, 6.560283801567334372 ) ) ;
#4875 = DIRECTION ( 'NONE',  ( -0.000000000000000000, -1.000000000000000000, -0.000000000000000000 ) ) ;
#4876 = DIRECTION ( 'NONE',  ( 0.000000000000000000, 0.000000000000000000, 1.000000000000000000 ) ) ;
#4878 = VERTEX_POINT ( 'NONE', #33795 ) ;
#4877 = AXIS2_PLACEMENT_3D ( 'NONE', #2511, #121656, #51654 ) ;
#4879 = DIRECTION ( 'NONE',  ( 0.000000000000000000, 1.000000000000000000, 0.000000000000000000 ) ) ;
#4880 = CIRCLE ( 'NONE', #32020, 0.06509327318403745899 ) ;
#4881 = ADVANCED_FACE ( 'NONE', ( #113648 ), #11466, .T. ) ;
#4882 = VECTOR ( 'NONE', #38306, 1000.000000000000000 ) ;
#4883 = EDGE_LOOP ( 'NONE', ( #106955, #41863 ) ) ;
#4884 = DIRECTION ( 'NONE',  ( -0.000000000000000000, 1.000000000000000000, -0.000000000000000000 ) ) ;
#4885 = ORIENTED_EDGE ( 'NONE', *, *, #105281, .T. ) ;
#4886 = DIRECTION ( 'NONE',  ( -0.000000000000000000, 1.000000000000000000, -0.000000000000000000 ) ) ;
#4887 = CARTESIAN_POINT ( 'NONE',  ( 186.5000000000000000, 6.123233995736766282E-16, 5.000000000000000000 ) ) ;
#4889 = EDGE_CURVE ( 'NONE', #106872, #121536, #118797, .T. ) ;
#4888 = CARTESIAN_POINT ( 'NONE',  ( 2.499999999999981792, 2.500000000000000000, 4.230127018922196669 ) ) ;
#4891 = AXIS2_PLACEMENT_3D ( 'NONE', #71967, #92220, #82437 ) ;
#4890 = CARTESIAN_POINT ( 'NONE',  ( 149.5981739382431783, 2.500000000000000000, 1.703575533167231537 ) ) ;
#4892 = EDGE_CURVE ( 'NONE', #26341, #110101, #21861, .T. ) ;
#4893 = ORIENTED_EDGE ( 'NONE', *, *, #19383, .F. ) ;
#4894 = DIRECTION ( 'NONE',  ( 0.000000000000000000, 0.000000000000000000, -1.000000000000000000 ) ) ;
#4895 = AXIS2_PLACEMENT_3D ( 'NONE', #21696, #4582, #72091 ) ;
#4896 = EDGE_CURVE ( 'NONE', #87803, #2505, #80434, .T. ) ;
#4897 = CARTESIAN_POINT ( 'NONE',  ( -6.450000000000019718, 12.50000000000000000, -6.148780366869526226 ) ) ;
#4898 = ORIENTED_EDGE ( 'NONE', *, *, #74468, .T. ) ;
#4899 = ORIENTED_EDGE ( 'NONE', *, *, #29341, .F. ) ;
#4900 = ORIENTED_EDGE ( 'NONE', *, *, #63743, .T. ) ;
#4901 = LINE ( 'NONE', #46132, #16523 ) ;
#4902 = DIRECTION ( 'NONE',  ( 0.000000000000000000, 0.000000000000000000, 1.000000000000000000 ) ) ;
#4903 = ADVANCED_FACE ( 'NONE', ( #48135 ), #17353, .T. ) ;
#4904 = CARTESIAN_POINT ( 'NONE',  ( 186.1510416670080588, 4.367472073101518859, -7.564683531249999149 ) ) ;
#4905 = VECTOR ( 'NONE', #76346, 1000.000000000000000 ) ;
#4906 = LINE ( 'NONE', #46793, #51308 ) ;
#4907 = DIRECTION ( 'NONE',  ( 0.000000000000000000, -0.9999939076577903929, 0.003490651415223739937 ) ) ;
#4908 = AXIS2_PLACEMENT_3D ( 'NONE', #31072, #70972, #21893 ) ;
#4909 = CIRCLE ( 'NONE', #119851, 0.06509327318403741736 ) ;
#4910 = AXIS2_PLACEMENT_3D ( 'NONE', #87452, #78312, #107751 ) ;
#4911 = CARTESIAN_POINT ( 'NONE',  ( 0.000000000000000000, 2.500000000000000000, 0.1000000000000000056 ) ) ;
#4912 = VECTOR ( 'NONE', #101764, 1000.000000000000000 ) ;
#4913 = VERTEX_POINT ( 'NONE', #47491 ) ;
#4914 = AXIS2_PLACEMENT_3D ( 'NONE', #122663, #80820, #102390 ) ;
#4915 = DIRECTION ( 'NONE',  ( -0.000000000000000000, 1.000000000000000000, -0.000000000000000000 ) ) ;
#4916 = ORIENTED_EDGE ( 'NONE', *, *, #51941, .T. ) ;
#4917 = PLANE ( 'NONE',  #28498 ) ;
#4918 = CARTESIAN_POINT ( 'NONE',  ( 4.149999999999938183, 12.50000000000000000, 7.188010851410848723 ) ) ;
#4919 = FACE_OUTER_BOUND ( 'NONE', #69320, .T. ) ;
#4920 = ORIENTED_EDGE ( 'NONE', *, *, #38781, .F. ) ;
#4921 = DIRECTION ( 'NONE',  ( 0.000000000000000000, 0.000000000000000000, -1.000000000000000000 ) ) ;
#4922 = CARTESIAN_POINT ( 'NONE',  ( 184.5000000000000000, 9.429780353434619030E-16, 7.699999999999999289 ) ) ;
#4923 = CONICAL_SURFACE ( 'NONE', #84465, 0.1000000000000002554, 0.003490658503988666988 ) ;
#4924 = ORIENTED_EDGE ( 'NONE', *, *, #8203, .F. ) ;
#4925 = DIRECTION ( 'NONE',  ( 0.000000000000000000, -0.9999939076577903929, 0.003490651415223739937 ) ) ;
#4926 = AXIS2_PLACEMENT_3D ( 'NONE', #66444, #67062, #107000 ) ;
#4927 = ORIENTED_EDGE ( 'NONE', *, *, #66993, .T. ) ;
#4928 = VECTOR ( 'NONE', #90141, 1000.000000000000000 ) ;
#4929 = EDGE_LOOP ( 'NONE', ( #11971, #67160, #14044, #4195 ) ) ;
#4930 = FACE_OUTER_BOUND ( 'NONE', #121558, .T. ) ;
#4931 = CIRCLE ( 'NONE', #44678, 0.1000000000000000472 ) ;
#4933 = EDGE_CURVE ( 'NONE', #21022, #42779, #48782, .T. ) ;
#4932 = AXIS2_PLACEMENT_3D ( 'NONE', #65610, #113427, #56429 ) ;
#4934 = ADVANCED_FACE ( 'NONE', ( #116853, #38319 ), #87392, .F. ) ;
#4935 = ORIENTED_EDGE ( 'NONE', *, *, #60109, .T. ) ;
#4936 = LINE ( 'NONE', #84800, #7019 ) ;
#4938 = EDGE_CURVE ( 'NONE', #58767, #28931, #23992, .T. ) ;
#4937 = DIRECTION ( 'NONE',  ( 0.000000000000000000, 0.000000000000000000, 1.000000000000000000 ) ) ;
#4939 = FACE_OUTER_BOUND ( 'NONE', #128868, .T. ) ;
#4941 = VERTEX_POINT ( 'NONE', #57308 ) ;
#4940 = CONICAL_SURFACE ( 'NONE', #80183, 0.1000000000000002554, 0.003490658503988666988 ) ;
#4942 = AXIS2_PLACEMENT_3D ( 'NONE', #33131, #121478, #61292 ) ;
#4943 = CONICAL_SURFACE ( 'NONE', #90640, 0.09999999999999999167, 0.003490658503988666988 ) ;
#4944 = FACE_BOUND ( 'NONE', #111556, .T. ) ;
#4945 = EDGE_CURVE ( 'NONE', #34926, #65177, #63707, .T. ) ;
#4946 = CARTESIAN_POINT ( 'NONE',  ( 11.24999999999991118, 2.500000000000000000, 5.802370205355744659 ) ) ;
#4948 = EDGE_LOOP ( 'NONE', ( #46157, #78105, #64882, #57992 ) ) ;
#4947 = CARTESIAN_POINT ( 'NONE',  ( -5.000000000000024869, 12.50000000000000000, -4.957854068765716882 ) ) ;
#4949 = CONICAL_SURFACE ( 'NONE', #46838, 0.09999999999999982514, 0.003490658503988666988 ) ;
#4950 = DIRECTION ( 'NONE',  ( -1.000000000000000000, -0.000000000000000000, -0.000000000000000000 ) ) ;
#4951 = DIRECTION ( 'NONE',  ( 0.000000000000000000, 0.000000000000000000, 1.000000000000000000 ) ) ;
#4952 = ORIENTED_EDGE ( 'NONE', *, *, #82872, .T. ) ;
#4953 = EDGE_CURVE ( 'NONE', #9679, #29270, #101363, .T. ) ;
#4954 = EDGE_CURVE ( 'NONE', #28355, #2437, #126393, .T. ) ;
#4955 = VERTEX_POINT ( 'NONE', #7543 ) ;
#4956 = VERTEX_POINT ( 'NONE', #88020 ) ;
#4957 = DIRECTION ( 'NONE',  ( 0.000000000000000000, 0.000000000000000000, -1.000000000000000000 ) ) ;
#4958 = DIRECTION ( 'NONE',  ( 0.000000000000000000, 0.000000000000000000, -1.000000000000000000 ) ) ;
#4959 = FACE_OUTER_BOUND ( 'NONE', #90951, .T. ) ;
#4960 = FACE_BOUND ( 'NONE', #56700, .T. ) ;
#4961 = EDGE_LOOP ( 'NONE', ( #83025, #126071 ) ) ;
#4962 = CARTESIAN_POINT ( 'NONE',  ( 185.6093750003413732, 9.264065473108010111E-16, -7.564683531250000925 ) ) ;
#4963 = ADVANCED_FACE ( 'NONE', ( #98496 ), #13508, .T. ) ;
#4964 = DIRECTION ( 'NONE',  ( -0.000000000000000000, 1.000000000000000000, -0.000000000000000000 ) ) ;
#4965 = DIRECTION ( 'NONE',  ( -1.000000000000000000, -0.000000000000000000, -0.000000000000000000 ) ) ;
#4966 = CONICAL_SURFACE ( 'NONE', #38449, 0.1000000000000002554, 0.003490658503988666988 ) ;
#4967 = FACE_OUTER_BOUND ( 'NONE', #61566, .T. ) ;
#4968 = DIRECTION ( 'NONE',  ( 0.000000000000000000, 0.000000000000000000, 1.000000000000000000 ) ) ;
#4969 = FACE_OUTER_BOUND ( 'NONE', #36693, .T. ) ;
#4970 = FACE_OUTER_BOUND ( 'NONE', #33727, .T. ) ;
#4971 = AXIS2_PLACEMENT_3D ( 'NONE', #16198, #96064, #76434 ) ;
#4972 = AXIS2_PLACEMENT_3D ( 'NONE', #41402, #2084, #102243 ) ;
#4973 = AXIS2_PLACEMENT_3D ( 'NONE', #36707, #27487, #37975 ) ;
#4974 = DIRECTION ( 'NONE',  ( 0.000000000000000000, -0.9999939076577903929, 0.003490651415223739937 ) ) ;
#4975 = ORIENTED_EDGE ( 'NONE', *, *, #26952, .F. ) ;
#4976 = ORIENTED_EDGE ( 'NONE', *, *, #21229, .T. ) ;
#4977 = ORIENTED_EDGE ( 'NONE', *, *, #54533, .T. ) ;
#4978 = ORIENTED_EDGE ( 'NONE', *, *, #121702, .T. ) ;
#4979 = ORIENTED_EDGE ( 'NONE', *, *, #113099, .T. ) ;
#4980 = CARTESIAN_POINT ( 'NONE',  ( -11.69999999999999929, 12.50000000000000000, -4.330127018922198978 ) ) ;
#4981 = CARTESIAN_POINT ( 'NONE',  ( 6.249999999999968914, 2.500000000000000000, -6.395190528383301931 ) ) ;
#4982 = VERTEX_POINT ( 'NONE', #8826 ) ;
#4983 = FACE_BOUND ( 'NONE', #60629, .T. ) ;
#4984 = CIRCLE ( 'NONE', #128357, 0.9999999999999995559 ) ;
#4985 = DIRECTION ( 'NONE',  ( -4.274815082592931898E-19, -0.9999939076577903929, -0.003490651415223739937 ) ) ;
#4986 = CIRCLE ( 'NONE', #63504, 0.1000000000000002554 ) ;
#4987 = AXIS2_PLACEMENT_3D ( 'NONE', #93336, #82883, #122793 ) ;
#4988 = FACE_OUTER_BOUND ( 'NONE', #27342, .T. ) ;
#4989 = ORIENTED_EDGE ( 'NONE', *, *, #39742, .T. ) ;
#4990 = CARTESIAN_POINT ( 'NONE',  ( 1.049999999999953637, 2.500000000000000000, 2.511473670974873507 ) ) ;
#4991 = DIRECTION ( 'NONE',  ( 0.000000000000000000, 1.000000000000000000, 0.000000000000000000 ) ) ;
#4992 = DIRECTION ( 'NONE',  ( 0.000000000000000000, 0.000000000000000000, -1.000000000000000000 ) ) ;
#4993 = AXIS2_PLACEMENT_3D ( 'NONE', #128017, #8232, #70389 ) ;
#4994 = ORIENTED_EDGE ( 'NONE', *, *, #26972, .T. ) ;
#4995 = DIRECTION ( 'NONE',  ( 0.000000000000000000, -0.9999939076577903929, 0.003490651415223739937 ) ) ;
#4996 = EDGE_LOOP ( 'NONE', ( #23252, #114972 ) ) ;
#4997 = EDGE_CURVE ( 'NONE', #108909, #47117, #97866, .T. ) ;
#4998 = AXIS2_PLACEMENT_3D ( 'NONE', #119920, #87222, #127179 ) ;
#4999 = CONICAL_SURFACE ( 'NONE', #109478, 0.09999999999999982514, 0.003490658503988666988 ) ;
#5000 = AXIS2_PLACEMENT_3D ( 'NONE', #128475, #87863, #7377 ) ;
#5001 = ORIENTED_EDGE ( 'NONE', *, *, #70586, .F. ) ;
#5002 = EDGE_LOOP ( 'NONE', ( #33042, #3095 ) ) ;
#5003 = CARTESIAN_POINT ( 'NONE',  ( 4.149999999999941735, 2.500000000000000000, -5.802370205355749988 ) ) ;
#5004 = CARTESIAN_POINT ( 'NONE',  ( 6.249999999999932498, 2.500000000000000000, -5.902370205355750521 ) ) ;
#5006 = CIRCLE ( 'NONE', #65651, 0.1000000000000002554 ) ;
#5005 = DIRECTION ( 'NONE',  ( -4.274815082592931898E-19, -0.9999939076577903929, -0.003490651415223739937 ) ) ;
#5007 = ORIENTED_EDGE ( 'NONE', *, *, #103438, .F. ) ;
#5008 = CARTESIAN_POINT ( 'NONE',  ( 8.497934422630084583, 2.499999999999237499, -9.526046681105988512 ) ) ;
#5009 = CIRCLE ( 'NONE', #128386, 0.09999999999999982514 ) ;
#5010 = CARTESIAN_POINT ( 'NONE',  ( -8.350000000000013856, 2.500000000000000000, -6.495190528383297135 ) ) ;
#5011 = CARTESIAN_POINT ( 'NONE',  ( -0.8500000000000386136, 2.500000000000000000, 5.802370205355744659 ) ) ;
#5012 = CARTESIAN_POINT ( 'NONE',  ( 186.9427083336747160, -6.551208109652278289, 3.782341765624995134 ) ) ;
#5013 = DIRECTION ( 'NONE',  ( 0.000000000000000000, 0.000000000000000000, -1.000000000000000000 ) ) ;
#5014 = CARTESIAN_POINT ( 'NONE',  ( 6.649999999999931077, 2.500000000000000000, -6.495190528383302464 ) ) ;
#5015 = ORIENTED_EDGE ( 'NONE', *, *, #117211, .T. ) ;
#5016 = CARTESIAN_POINT ( 'NONE',  ( -11.64999999999999680, 2.500000000000000000, -6.495190528383298911 ) ) ;
#5017 = EDGE_LOOP ( 'NONE', ( #24373, #85596, #89158, #101784, #111936 ) ) ;
#5018 = ORIENTED_EDGE ( 'NONE', *, *, #11367, .T. ) ;
#5019 = DIRECTION ( 'NONE',  ( -0.000000000000000000, 1.000000000000000000, -0.000000000000000000 ) ) ;
#5020 = FACE_OUTER_BOUND ( 'NONE', #35499, .T. ) ;
#5021 = CIRCLE ( 'NONE', #120061, 0.06509327318403745899 ) ;
#5022 = VECTOR ( 'NONE', #46939, 1000.000000000000000 ) ;
#5023 = DIRECTION ( 'NONE',  ( -0.000000000000000000, 1.000000000000000000, -0.000000000000000000 ) ) ;
#5024 = VECTOR ( 'NONE', #108530, 1000.000000000000000 ) ;
#5025 = PLANE ( 'NONE',  #71779 ) ;
#5026 = CARTESIAN_POINT ( 'NONE',  ( -3.750000000000027534, 2.500000000000000000, -1.572243186433550211 ) ) ;
#5027 = VERTEX_POINT ( 'NONE', #128654 ) ;
#5028 = VERTEX_POINT ( 'NONE', #126697 ) ;
#5029 = CARTESIAN_POINT ( 'NONE',  ( 10.39999999999991154, 12.50000000000000000, -5.022947341949754119 ) ) ;
#5030 = CONICAL_SURFACE ( 'NONE', #61500, 0.09999999999999982514, 0.003490658503988666988 ) ;
#5031 = AXIS2_PLACEMENT_3D ( 'NONE', #117433, #19250, #38274 ) ;
#5032 = CARTESIAN_POINT ( 'NONE',  ( 59.86262955839788447, 3.775832727647709497, -4.995375241584474324 ) ) ;
#5033 = CIRCLE ( 'NONE', #107454, 0.1000000000000002554 ) ;
#5034 = DIRECTION ( 'NONE',  ( 0.000000000000000000, 1.000000000000000000, 0.000000000000000000 ) ) ;
#5035 = ORIENTED_EDGE ( 'NONE', *, *, #30435, .T. ) ;
#5036 = VERTEX_POINT ( 'NONE', #67764 ) ;
#5037 = LINE ( 'NONE', #94715, #114697 ) ;
#5038 = ADVANCED_FACE ( 'NONE', ( #38989 ), #69968, .T. ) ;
#5039 = EDGE_LOOP ( 'NONE', ( #7533, #54215, #19907, #25528 ) ) ;
#5040 = CARTESIAN_POINT ( 'NONE',  ( -3.350000000000032507, 2.500000000000000000, -6.595190528383302109 ) ) ;
#5042 = EDGE_CURVE ( 'NONE', #68393, #45115, #86679, .T. ) ;
#5041 = VECTOR ( 'NONE', #98844, 1000.000000000000000 ) ;
#5043 = DIRECTION ( 'NONE',  ( 0.000000000000000000, 0.000000000000000000, 1.000000000000000000 ) ) ;
#5044 = ORIENTED_EDGE ( 'NONE', *, *, #46268, .T. ) ;
#5045 = LINE ( 'NONE', #54169, #119264 ) ;
#5046 = CARTESIAN_POINT ( 'NONE',  ( 0.5999999999999612310, 12.50000000000000000, -0.3464101615137760715 ) ) ;
#5047 = CARTESIAN_POINT ( 'NONE',  ( 11.44999999999990870, 12.50000000000000000, 6.841600689897072485 ) ) ;
#5048 = CONICAL_SURFACE ( 'NONE', #74016, 0.1000000000000002554, 0.003490658503988666988 ) ;
#5049 = EDGE_CURVE ( 'NONE', #23957, #55213, #103415, .T. ) ;
#5050 = DIRECTION ( 'NONE',  ( -0.000000000000000000, -1.000000000000000000, -0.000000000000000000 ) ) ;
#5051 = EDGE_CURVE ( 'NONE', #58166, #52632, #113880, .T. ) ;
#5052 = ORIENTED_EDGE ( 'NONE', *, *, #108774, .T. ) ;
#5053 = CARTESIAN_POINT ( 'NONE',  ( -12.29999999999999361, 2.500000000000000000, 3.883716857408420431 ) ) ;
#5054 = LINE ( 'NONE', #124847, #24714 ) ;
#5055 = EDGE_CURVE ( 'NONE', #92856, #126533, #1005, .T. ) ;
#5056 = ORIENTED_EDGE ( 'NONE', *, *, #91059, .F. ) ;
#5057 = EDGE_CURVE ( 'NONE', #63382, #73184, #36528, .T. ) ;
#5058 = SHAPE_REPRESENTATION ( 'Waterproof Outer Handle Shell', ( #108296 ), #20574 ) ;
#5059 = ORIENTED_EDGE ( 'NONE', *, *, #24741, .T. ) ;
#5060 = EDGE_CURVE ( 'NONE', #15503, #19409, #74169, .T. ) ;
#5061 = CARTESIAN_POINT ( 'NONE',  ( 185.7552083336747444, 6.551208109652275624, -3.782341765624998686 ) ) ;
#5063 = EDGE_CURVE ( 'NONE', #93363, #81045, #10746, .T. ) ;
#5062 = DIRECTION ( 'NONE',  ( 0.000000000000000000, -0.000000000000000000, 1.000000000000000000 ) ) ;
#5064 = EDGE_CURVE ( 'NONE', #41827, #90531, #76230, .T. ) ;
#5065 = DIRECTION ( 'NONE',  ( 0.000000000000000000, 0.000000000000000000, 1.000000000000000000 ) ) ;
#5066 = CIRCLE ( 'NONE', #78251, 0.06509327318403745899 ) ;
#5067 = LINE ( 'NONE', #125490, #122120 ) ;
#5068 = CARTESIAN_POINT ( 'NONE',  ( -3.550000000000027356, 12.50000000000000000, -2.511473670974877948 ) ) ;
#5069 = CARTESIAN_POINT ( 'NONE',  ( 15.83209681635554666, 2.500000000000000000, -5.404881881984140435 ) ) ;
#5070 = DIRECTION ( 'NONE',  ( 0.000000000000000000, 0.000000000000000000, -1.000000000000000000 ) ) ;
#5071 = DIRECTION ( 'NONE',  ( 1.000000000000000000, 0.000000000000000000, -1.084202172485504434E-16 ) ) ;
#5072 = DIRECTION ( 'NONE',  ( -0.000000000000000000, 1.000000000000000000, -0.000000000000000000 ) ) ;
#5073 = EDGE_CURVE ( 'NONE', #72972, #97694, #109677, .T. ) ;
#5074 = DIRECTION ( 'NONE',  ( -0.000000000000000000, -1.000000000000000000, -0.000000000000000000 ) ) ;
#5075 = VERTEX_POINT ( 'NONE', #22553 ) ;
#5076 = CIRCLE ( 'NONE', #109554, 0.1000000000000002554 ) ;
#5077 = EDGE_LOOP ( 'NONE', ( #70411, #17156, #19043, #78322 ) ) ;
#5078 = VERTEX_POINT ( 'NONE', #23166 ) ;
#5079 = ORIENTED_EDGE ( 'NONE', *, *, #117055, .F. ) ;
#5080 = DIRECTION ( 'NONE',  ( 0.000000000000000000, 0.000000000000000000, -1.000000000000000000 ) ) ;
#5081 = DIRECTION ( 'NONE',  ( 0.000000000000000000, 0.000000000000000000, 1.000000000000000000 ) ) ;
#5082 = CARTESIAN_POINT ( 'NONE',  ( 4.349999999999937472, 2.500000000000000000, 6.741600689897071952 ) ) ;
#5083 = ORIENTED_EDGE ( 'NONE', *, *, #121374, .F. ) ;
#5084 = DIRECTION ( 'NONE',  ( 0.000000000000000000, 1.000000000000000000, 0.000000000000000000 ) ) ;
#5085 = CIRCLE ( 'NONE', #117952, 0.1000000000000000472 ) ;
#5086 = CARTESIAN_POINT ( 'NONE',  ( -7.050000000000016698, 2.500000000000000000, -6.495190528383302464 ) ) ;
#5088 = ORIENTED_EDGE ( 'NONE', *, *, #7587, .T. ) ;
#5087 = FACE_OUTER_BOUND ( 'NONE', #58025, .T. ) ;
#5089 = CARTESIAN_POINT ( 'NONE',  ( 1.049999999999954081, 2.500000000000000000, -6.148780366869526226 ) ) ;
#5090 = VERTEX_POINT ( 'NONE', #21905 ) ;
#5091 = AXIS2_PLACEMENT_3D ( 'NONE', #62301, #102220, #32847 ) ;
#5092 = VECTOR ( 'NONE', #126057, 1000.000000000000000 ) ;
#5093 = ORIENTED_EDGE ( 'NONE', *, *, #5228, .T. ) ;
#5094 = VERTEX_POINT ( 'NONE', #52004 ) ;
#5095 = ORIENTED_EDGE ( 'NONE', *, *, #86730, .T. ) ;
#5096 = CARTESIAN_POINT ( 'NONE',  ( -0.8500000000000390576, 12.50000000000000000, -2.099970236277064473 ) ) ;
#5097 = CIRCLE ( 'NONE', #90788, 0.1000000000000000472 ) ;
#5098 = EDGE_CURVE ( 'NONE', #37944, #84568, #95005, .T. ) ;
#5099 = FACE_OUTER_BOUND ( 'NONE', #17057, .T. ) ;
#5101 = EDGE_CURVE ( 'NONE', #3892, #26528, #49052, .T. ) ;
#5100 = DIRECTION ( 'NONE',  ( 0.000000000000000000, 1.000000000000000000, 0.000000000000000000 ) ) ;
#5102 = CONICAL_SURFACE ( 'NONE', #53246, 0.1000000000000000472, 0.003490658503988666988 ) ;
#5103 = FACE_OUTER_BOUND ( 'NONE', #88549, .T. ) ;
#5104 = ORIENTED_EDGE ( 'NONE', *, *, #67744, .F. ) ;
#5105 = EDGE_CURVE ( 'NONE', #111372, #122281, #21957, .T. ) ;
#5106 = DIRECTION ( 'NONE',  ( -0.000000000000000000, -1.000000000000000000, -0.000000000000000000 ) ) ;
#5107 = ORIENTED_EDGE ( 'NONE', *, *, #111762, .T. ) ;
#5108 = LINE ( 'NONE', #26055, #78958 ) ;
#5109 = LINE ( 'NONE', #44402, #37228 ) ;
#5110 = DIRECTION ( 'NONE',  ( 0.000000000000000000, 0.000000000000000000, 1.000000000000000000 ) ) ;
#5111 = CARTESIAN_POINT ( 'NONE',  ( 16.09541403888747624, -2.463474929527651458, 3.723514363708886776 ) ) ;
#5112 = EDGE_CURVE ( 'NONE', #120069, #17444, #15651, .T. ) ;
#5113 = EDGE_CURVE ( 'NONE', #114788, #10245, #78383, .T. ) ;
#5114 = ORIENTED_EDGE ( 'NONE', *, *, #22390, .T. ) ;
#5115 = ADVANCED_FACE ( 'NONE', ( #50700 ), #110898, .T. ) ;
#5116 = EDGE_CURVE ( 'NONE', #49994, #107746, #95099, .T. ) ;
#5117 = VECTOR ( 'NONE', #81844, 1000.000000000000000 ) ;
#5118 = VERTEX_POINT ( 'NONE', #111554 ) ;
#5119 = ORIENTED_EDGE ( 'NONE', *, *, #24766, .F. ) ;
#5120 = CARTESIAN_POINT ( 'NONE',  ( -4.600000000000024514, 12.50000000000000000, 0.6928203230275494784 ) ) ;
#5121 = FACE_OUTER_BOUND ( 'NONE', #119665, .T. ) ;
#5122 = DIRECTION ( 'NONE',  ( 0.000000000000000000, 0.000000000000000000, 1.000000000000000000 ) ) ;
#5123 = FACE_BOUND ( 'NONE', #122538, .T. ) ;
#5124 = CARTESIAN_POINT ( 'NONE',  ( -6.650000000000019007, 12.50000000000000000, -1.472243186433550122 ) ) ;
#5125 = DIRECTION ( 'NONE',  ( 0.000000000000000000, 0.000000000000000000, 1.000000000000000000 ) ) ;
#5126 = EDGE_CURVE ( 'NONE', #91178, #77609, #32432, .T. ) ;
#5127 = CARTESIAN_POINT ( 'NONE',  ( -4.600000000000024514, 2.500000000000000000, 0.5928203230275495006 ) ) ;
#5128 = CIRCLE ( 'NONE', #19813, 0.06509327318403745899 ) ;
#5129 = VECTOR ( 'NONE', #55090, 1000.000000000000000 ) ;
#5130 = VECTOR ( 'NONE', #23788, 1000.000000000000000 ) ;
#5131 = CARTESIAN_POINT ( 'NONE',  ( -2.900000000000029221, 12.50000000000000000, -0.6277270498435166823 ) ) ;
#5132 = VECTOR ( 'NONE', #119709, 1000.000000000000000 ) ;
#5133 = CARTESIAN_POINT ( 'NONE',  ( 5.399999999999931966, 12.50000000000000000, 4.265033745738159077 ) ) ;
#5134 = FACE_OUTER_BOUND ( 'NONE', #43130, .T. ) ;
#5135 = ORIENTED_EDGE ( 'NONE', *, *, #12320, .F. ) ;
#5136 = VECTOR ( 'NONE', #127583, 1000.000000000000000 ) ;
#5137 = CIRCLE ( 'NONE', #120082, 0.1000000000000000472 ) ;
#5138 = CARTESIAN_POINT ( 'NONE',  ( 3.149999999999946176, 2.500000000000000000, -6.741600689897077281 ) ) ;
#5139 = ORIENTED_EDGE ( 'NONE', *, *, #105703, .F. ) ;
#5140 = EDGE_LOOP ( 'NONE', ( #95781, #109775, #28832, #97676 ) ) ;
#5141 = VERTEX_POINT ( 'NONE', #40915 ) ;
#5142 = EDGE_LOOP ( 'NONE', ( #74538, #112223, #95546, #125646 ) ) ;
#5143 = AXIS2_PLACEMENT_3D ( 'NONE', #93465, #13598, #14866 ) ;
#5144 = CARTESIAN_POINT ( 'NONE',  ( -2.050000000000033129, 2.500000000000000000, 2.265063509461097357 ) ) ;
#5145 = EDGE_CURVE ( 'NONE', #53201, #5697, #61170, .T. ) ;
#5146 = FACE_BOUND ( 'NONE', #2391, .T. ) ;
#5147 = DIRECTION ( 'NONE',  ( 0.000000000000000000, 1.000000000000000000, -0.000000000000000000 ) ) ;
#5148 = ORIENTED_EDGE ( 'NONE', *, *, #112779, .F. ) ;
#5149 = CARTESIAN_POINT ( 'NONE',  ( 24.00496409367085704, 0.9037364216963271746, 4.313973893093799639 ) ) ;
#5150 = FACE_OUTER_BOUND ( 'NONE', #95012, .T. ) ;
#5152 = VERTEX_POINT ( 'NONE', #92559 ) ;
#5151 = VECTOR ( 'NONE', #69136, 1000.000000000000000 ) ;
#5153 = DIRECTION ( 'NONE',  ( 0.000000000000000000, -0.000000000000000000, 1.000000000000000000 ) ) ;
#5154 = DIRECTION ( 'NONE',  ( 0.000000000000000000, 0.000000000000000000, -1.000000000000000000 ) ) ;
#5155 = ADVANCED_FACE ( 'NONE', ( #112207 ), #62477, .T. ) ;
#5156 = ORIENTED_EDGE ( 'NONE', *, *, #94770, .F. ) ;
#5157 = DIRECTION ( 'NONE',  ( 0.000000000000000000, 0.000000000000000000, 1.000000000000000000 ) ) ;
#5158 = DIRECTION ( 'NONE',  ( 1.000000000000000000, 0.000000000000000000, 0.000000000000000000 ) ) ;
#5159 = AXIS2_PLACEMENT_3D ( 'NONE', #24010, #72471, #62655 ) ;
#5160 = AXIS2_PLACEMENT_3D ( 'NONE', #26721, #55542, #105926 ) ;
#5161 = ORIENTED_EDGE ( 'NONE', *, *, #48364, .T. ) ;
#5162 = DIRECTION ( 'NONE',  ( -0.000000000000000000, -1.000000000000000000, -0.000000000000000000 ) ) ;
#5163 = CARTESIAN_POINT ( 'NONE',  ( 12.29999999999990479, 12.50000000000000000, 4.676537180435972552 ) ) ;
#5164 = ORIENTED_EDGE ( 'NONE', *, *, #4452, .F. ) ;
#5165 = ORIENTED_EDGE ( 'NONE', *, *, #4306, .T. ) ;
#5166 = ADVANCED_FACE ( 'NONE', ( #52630 ), #33020, .T. ) ;
#5167 = DIRECTION ( 'NONE',  ( 0.000000000000000000, 0.000000000000000000, 1.000000000000000000 ) ) ;
#5168 = VERTEX_POINT ( 'NONE', #54551 ) ;
#5169 = CARTESIAN_POINT ( 'NONE',  ( 17.50000000000000000, -2.500000000000000000, -2.922290670087884124 ) ) ;
#5170 = DIRECTION ( 'NONE',  ( 0.000000000000000000, 0.000000000000000000, 1.000000000000000000 ) ) ;
#5171 = CIRCLE ( 'NONE', #78365, 0.1000000000000002554 ) ;
#5172 = ORIENTED_EDGE ( 'NONE', *, *, #81372, .T. ) ;
#5173 = CARTESIAN_POINT ( 'NONE',  ( -6.250000000000021316, 12.50000000000000000, -5.802370205355749988 ) ) ;
#5174 = DIRECTION ( 'NONE',  ( -0.000000000000000000, 1.000000000000000000, -0.000000000000000000 ) ) ;
#5175 = LINE ( 'NONE', #45127, #46627 ) ;
#5176 = FACE_OUTER_BOUND ( 'NONE', #48615, .T. ) ;
#5177 = DIRECTION ( 'NONE',  ( 0.000000000000000000, 0.000000000000000000, -1.000000000000000000 ) ) ;
#5178 = EDGE_LOOP ( 'NONE', ( #95951, #113524 ) ) ;
#5179 = ORIENTED_EDGE ( 'NONE', *, *, #23707, .F. ) ;
#5180 = FACE_OUTER_BOUND ( 'NONE', #117236, .T. ) ;
#5181 = AXIS2_PLACEMENT_3D ( 'NONE', #62153, #625, #80504 ) ;
#5182 = CONICAL_SURFACE ( 'NONE', #128571, 0.1000000000000002554, 0.003490658503988666988 ) ;
#5183 = DIRECTION ( 'NONE',  ( -0.000000000000000000, -1.000000000000000000, -0.000000000000000000 ) ) ;
#5184 = CARTESIAN_POINT ( 'NONE',  ( 11.44999999999990514, 2.500000000000000000, -6.048780366869526581 ) ) ;
#5186 = ORIENTED_EDGE ( 'NONE', *, *, #51232, .F. ) ;
#5185 = ORIENTED_EDGE ( 'NONE', *, *, #14288, .F. ) ;
#5187 = EDGE_LOOP ( 'NONE', ( #48315, #57710 ) ) ;
#5188 = CIRCLE ( 'NONE', #90885, 0.09999999999999982514 ) ;
#5189 = CARTESIAN_POINT ( 'NONE',  ( 2.899999999999946620, 2.500000000000000000, 0.6928203230275494784 ) ) ;
#5190 = AXIS2_PLACEMENT_3D ( 'NONE', #112853, #60552, #12061 ) ;
#5191 = DIRECTION ( 'NONE',  ( 0.000000000000000000, 0.000000000000000000, 1.000000000000000000 ) ) ;
#5192 = CARTESIAN_POINT ( 'NONE',  ( -8.300000000000011369, 2.500000000000000000, -4.430127018922202176 ) ) ;
#5193 = EDGE_CURVE ( 'NONE', #4124, #949, #119951, .T. ) ;
#5194 = DIRECTION ( 'NONE',  ( 1.000000000000000000, 0.000000000000000000, 0.000000000000000000 ) ) ;
#5195 = CARTESIAN_POINT ( 'NONE',  ( -3.950000000000024603, 2.500000000000000000, 1.918653347947321564 ) ) ;
#5196 = CARTESIAN_POINT ( 'NONE',  ( 165.4999999999999716, 0.000000000000000000, -2.000000000000000000 ) ) ;
#5197 = DIRECTION ( 'NONE',  ( 0.000000000000000000, 0.000000000000000000, -1.000000000000000000 ) ) ;
#5198 = FACE_OUTER_BOUND ( 'NONE', #122937, .T. ) ;
#5199 = PLANE ( 'NONE',  #63437 ) ;
#5200 = CARTESIAN_POINT ( 'NONE',  ( -0.2000000000000412836, 2.500000000000000000, 4.676537180435972552 ) ) ;
#5201 = EDGE_LOOP ( 'NONE', ( #55497, #48337 ) ) ;
#5202 = AXIS2_PLACEMENT_3D ( 'NONE', #78510, #25497, #5859 ) ;
#5203 = VECTOR ( 'NONE', #100538, 1000.000000000000000 ) ;
#5204 = CARTESIAN_POINT ( 'NONE',  ( -2.950000000000029932, 2.500000000000000000, -2.165063509461101710 ) ) ;
#5205 = EDGE_CURVE ( 'NONE', #42741, #60040, #122013, .T. ) ;
#5206 = AXIS2_PLACEMENT_3D ( 'NONE', #34509, #84870, #63298 ) ;
#5207 = ORIENTED_EDGE ( 'NONE', *, *, #12039, .T. ) ;
#5208 = EDGE_CURVE ( 'NONE', #82898, #110307, #74214, .T. ) ;
#5209 = ORIENTED_EDGE ( 'NONE', *, *, #55722, .T. ) ;
#5210 = EDGE_CURVE ( 'NONE', #59339, #123245, #34290, .T. ) ;
#5211 = DIRECTION ( 'NONE',  ( 0.000000000000000000, 1.000000000000000000, 0.000000000000000000 ) ) ;
#5213 = ADVANCED_FACE ( 'NONE', ( #34950 ), #84352, .T. ) ;
#5212 = CARTESIAN_POINT ( 'NONE',  ( -12.49999999999995737, 2.500000000000000000, 4.230127018922196669 ) ) ;
#5214 = DIRECTION ( 'NONE',  ( 0.000000000000000000, -0.9999939076577903929, 0.003490651415223739937 ) ) ;
#5215 = CIRCLE ( 'NONE', #105584, 0.06509327318403745899 ) ;
#5216 = CARTESIAN_POINT ( 'NONE',  ( 12.49999999999990408, 2.500000000000000000, 4.922947341949748257 ) ) ;
#5217 = AXIS2_PLACEMENT_3D ( 'NONE', #54285, #66668, #85673 ) ;
#5219 = DIRECTION ( 'NONE',  ( 0.000000000000000000, 0.000000000000000000, -1.000000000000000000 ) ) ;
#5218 = AXIS2_PLACEMENT_3D ( 'NONE', #80091, #31015, #32309 ) ;
#5220 = ADVANCED_FACE ( 'NONE', ( #66314 ), #65569, .T. ) ;
#5221 = FACE_OUTER_BOUND ( 'NONE', #89162, .T. ) ;
#5222 = DIRECTION ( 'NONE',  ( -4.274815082592931898E-19, -0.9999939076577903929, -0.003490651415223739937 ) ) ;
#5223 = VERTEX_POINT ( 'NONE', #114768 ) ;
#5224 = DIRECTION ( 'NONE',  ( 0.000000000000000000, 1.000000000000000000, 0.000000000000000000 ) ) ;
#5225 = AXIS2_PLACEMENT_3D ( 'NONE', #47612, #77065, #87509 ) ;
#5226 = ADVANCED_FACE ( 'NONE', ( #33646 ), #80251, .T. ) ;
#5228 = EDGE_CURVE ( 'NONE', #26496, #18441, #125246, .T. ) ;
#5227 = DIRECTION ( 'NONE',  ( -0.000000000000000000, 1.000000000000000000, -0.000000000000000000 ) ) ;
#5230 = EDGE_LOOP ( 'NONE', ( #47623, #1173 ) ) ;
#5229 = CIRCLE ( 'NONE', #57477, 0.06509327318403745899 ) ;
#5231 = AXIS2_PLACEMENT_3D ( 'NONE', #3562, #4830, #43506 ) ;
#5232 = EDGE_CURVE ( 'NONE', #18500, #90643, #55115, .T. ) ;
#5233 = VERTEX_POINT ( 'NONE', #44099 ) ;
#5234 = EDGE_LOOP ( 'NONE', ( #57950, #100376 ) ) ;
#5235 = CONICAL_SURFACE ( 'NONE', #103545, 0.09999999999999982514, 0.003490658503988666988 ) ;
#5236 = PRODUCT_DEFINITION ( 'UNKNOWN', '', #4519, #49332 ) ;
#5237 = ORIENTED_EDGE ( 'NONE', *, *, #17928, .F. ) ;
#5238 = EDGE_CURVE ( 'NONE', #21571, #58472, #23813, .T. ) ;
#5239 = DIRECTION ( 'NONE',  ( 0.000000000000000000, 0.000000000000000000, 1.000000000000000000 ) ) ;
#5240 = DIRECTION ( 'NONE',  ( -0.000000000000000000, -1.000000000000000000, -0.000000000000000000 ) ) ;
#5241 = CARTESIAN_POINT ( 'NONE',  ( 16.55763164795904174, -0.1615198509451942488, -6.093150836621332722 ) ) ;
#5242 = CARTESIAN_POINT ( 'NONE',  ( -11.05000000000000071, 2.500000000000000000, -6.741600689897074616 ) ) ;
#5243 = LINE ( 'NONE', #74634, #61788 ) ;
#5244 = ORIENTED_EDGE ( 'NONE', *, *, #9392, .F. ) ;
#5245 = CARTESIAN_POINT ( 'NONE',  ( 3.549999999999940314, 2.500000000000000000, 6.741600689897071952 ) ) ;
#5246 = CARTESIAN_POINT ( 'NONE',  ( 7.949999999999922018, 12.50000000000000000, 6.495190528383297135 ) ) ;
#5247 = AXIS2_PLACEMENT_3D ( 'NONE', #70212, #110764, #110132 ) ;
#5248 = CARTESIAN_POINT ( 'NONE',  ( 1.849999999999949685, 2.500000000000000000, -2.411473670974877859 ) ) ;
#5249 = ORIENTED_EDGE ( 'NONE', *, *, #93634, .F. ) ;
#5250 = VERTEX_POINT ( 'NONE', #14619 ) ;
#5251 = ORIENTED_EDGE ( 'NONE', *, *, #54967, .T. ) ;
#5252 = CARTESIAN_POINT ( 'NONE',  ( -3.950000000000029932, 12.50000000000000000, -6.083687093685488989 ) ) ;
#5253 = CIRCLE ( 'NONE', #53308, 0.1000000000000002554 ) ;
#5254 = FACE_OUTER_BOUND ( 'NONE', #120150, .T. ) ;
#5255 = FACE_OUTER_BOUND ( 'NONE', #26043, .T. ) ;
#5256 = ORIENTED_EDGE ( 'NONE', *, *, #23355, .F. ) ;
#5257 = CARTESIAN_POINT ( 'NONE',  ( 6.049999999999935874, 2.500000000000000000, -6.741600689897077281 ) ) ;
#5258 = CARTESIAN_POINT ( 'NONE',  ( -8.150000000000012790, 12.50000000000000000, -1.818653347947326138 ) ) ;
#5259 = CARTESIAN_POINT ( 'NONE',  ( -7.300000000000016698, 12.50000000000000000, -0.2813168883297409439 ) ) ;
#5260 = DIRECTION ( 'NONE',  ( 0.000000000000000000, 0.000000000000000000, 1.000000000000000000 ) ) ;
#5261 = LINE ( 'NONE', #13790, #72862 ) ;
#5262 = CONICAL_SURFACE ( 'NONE', #78461, 0.1000000000000000472, 0.003490658503988666988 ) ;
#5263 = EDGE_CURVE ( 'NONE', #112855, #38253, #105283, .T. ) ;
#5264 = VERTEX_POINT ( 'NONE', #105612 ) ;
#5265 = LINE ( 'NONE', #85119, #87555 ) ;
#5267 = ADVANCED_FACE ( 'NONE', ( #46050 ), #116060, .T. ) ;
#5266 = AXIS2_PLACEMENT_3D ( 'NONE', #24809, #94834, #5154 ) ;
#5268 = EDGE_LOOP ( 'NONE', ( #98109, #36872 ) ) ;
#5269 = EDGE_LOOP ( 'NONE', ( #112041, #86507, #20833, #10520 ) ) ;
#5270 = VERTEX_POINT ( 'NONE', #43477 ) ;
#5271 = CARTESIAN_POINT ( 'NONE',  ( 1.049999999999953637, 12.50000000000000000, 2.511473670974873507 ) ) ;
#5272 = FACE_BOUND ( 'NONE', #17793, .T. ) ;
#5273 = CARTESIAN_POINT ( 'NONE',  ( -1.250000000000035749, 2.500000000000000000, -2.857883832488653741 ) ) ;
#5274 = EDGE_CURVE ( 'NONE', #104358, #12341, #51015, .T. ) ;
#5275 = DIRECTION ( 'NONE',  ( -0.000000000000000000, 1.000000000000000000, -0.000000000000000000 ) ) ;
#5276 = AXIS2_PLACEMENT_3D ( 'NONE', #64390, #51375, #91278 ) ;
#5277 = CIRCLE ( 'NONE', #67977, 0.1000000000000002554 ) ;
#5278 = ORIENTED_EDGE ( 'NONE', *, *, #23064, .F. ) ;
#5279 = CARTESIAN_POINT ( 'NONE',  ( -14.99999999999994671, 2.500000000000000000, -0.1000000000000000056 ) ) ;
#5280 = DIRECTION ( 'NONE',  ( 0.000000000000000000, 0.000000000000000000, 1.000000000000000000 ) ) ;
#5281 = CARTESIAN_POINT ( 'NONE',  ( 11.04999999999990834, 12.50000000000000000, -6.906693963081115051 ) ) ;
#5282 = DIRECTION ( 'NONE',  ( 0.000000000000000000, 0.000000000000000000, 1.000000000000000000 ) ) ;
#5283 = EDGE_LOOP ( 'NONE', ( #93950, #81481 ) ) ;
#5284 = CARTESIAN_POINT ( 'NONE',  ( -8.550000000000007816, 12.50000000000000000, 6.148780366869520009 ) ) ;
#5285 = CARTESIAN_POINT ( 'NONE',  ( 139.9358549477330200, 2.500000000000000000, -3.576063159858998475 ) ) ;
#5286 = CIRCLE ( 'NONE', #59710, 0.1000000000000000056 ) ;
#5287 = EDGE_LOOP ( 'NONE', ( #14898, #42890 ) ) ;
#5288 = DIRECTION ( 'NONE',  ( -0.000000000000000000, 1.000000000000000000, -0.000000000000000000 ) ) ;
#5289 = AXIS2_PLACEMENT_3D ( 'NONE', #128226, #18891, #68642 ) ;
#5290 = EDGE_LOOP ( 'NONE', ( #124242, #93623, #55790, #42089 ) ) ;
#5291 = FACE_BOUND ( 'NONE', #14517, .T. ) ;
#5292 = DIRECTION ( 'NONE',  ( 0.000000000000000000, 0.000000000000000000, 1.000000000000000000 ) ) ;
#5293 = CIRCLE ( 'NONE', #118177, 0.06509327318403745899 ) ;
#5294 = ORIENTED_EDGE ( 'NONE', *, *, #41057, .T. ) ;
#5295 = CARTESIAN_POINT ( 'NONE',  ( -6.850000000000017408, 12.50000000000000000, -6.083687093685488989 ) ) ;
#5296 = DIRECTION ( 'NONE',  ( -0.000000000000000000, -1.000000000000000000, -0.000000000000000000 ) ) ;
#5297 = AXIS2_PLACEMENT_3D ( 'NONE', #16014, #44193, #125344 ) ;
#5298 = VECTOR ( 'NONE', #66199, 1000.000000000000000 ) ;
#5299 = ORIENTED_EDGE ( 'NONE', *, *, #73497, .T. ) ;
#5300 = ORIENTED_EDGE ( 'NONE', *, *, #58998, .F. ) ;
#5301 = CARTESIAN_POINT ( 'NONE',  ( 186.0885416670080872, -6.551208109652273848, -3.782341765625003571 ) ) ;
#5302 = ORIENTED_EDGE ( 'NONE', *, *, #70127, .T. ) ;
#5303 = CARTESIAN_POINT ( 'NONE',  ( -14.79999999999998472, 12.50000000000000000, 0.4115034346978132529 ) ) ;
#5304 = DIRECTION ( 'NONE',  ( 0.000000000000000000, 1.000000000000000000, 0.000000000000000000 ) ) ;
#5305 = AXIS2_PLACEMENT_3D ( 'NONE', #99376, #9696, #37863 ) ;
#5306 = CIRCLE ( 'NONE', #120261, 0.09999999999999999167 ) ;
#5307 = CARTESIAN_POINT ( 'NONE',  ( 12.09999999999990550, 2.500000000000000000, -4.230127018922201998 ) ) ;
#5308 = CARTESIAN_POINT ( 'NONE',  ( -4.120979160187744630E-14, 12.50000000000000000, 3.572213422710607489 ) ) ;
#5309 = AXIS2_PLACEMENT_3D ( 'NONE', #99289, #121479, #39094 ) ;
#5310 = DIRECTION ( 'NONE',  ( -0.000000000000000000, -1.000000000000000000, -0.000000000000000000 ) ) ;
#5311 = CARTESIAN_POINT ( 'NONE',  ( -4.600000000000025402, 2.500000000000000000, 0.09999999999999761857 ) ) ;
#5312 = CIRCLE ( 'NONE', #122329, 0.06509327318403745899 ) ;
#5313 = VECTOR ( 'NONE', #22428, 1000.000000000000000 ) ;
#5314 = VERTEX_POINT ( 'NONE', #104938 ) ;
#5316 = VERTEX_POINT ( 'NONE', #55223 ) ;
#5315 = AXIS2_PLACEMENT_3D ( 'NONE', #11323, #100356, #99715 ) ;
#5317 = CARTESIAN_POINT ( 'NONE',  ( 7.899999999999924860, 2.500000000000000000, -4.922947341949753586 ) ) ;
#5318 = LINE ( 'NONE', #45265, #127083 ) ;
#5319 = CARTESIAN_POINT ( 'NONE',  ( -2.500000000000032419, 12.50000000000000000, 0.6928203230275494784 ) ) ;
#5320 = CONICAL_SURFACE ( 'NONE', #59739, 0.1000000000000000472, 0.003490658503988666988 ) ;
#5321 = EDGE_CURVE ( 'NONE', #95827, #3051, #96958, .T. ) ;
#5322 = CARTESIAN_POINT ( 'NONE',  ( -4.999999999999986677, 12.50000000000000000, -0.06509327318403970719 ) ) ;
#5324 = ORIENTED_EDGE ( 'NONE', *, *, #86536, .F. ) ;
#5323 = ORIENTED_EDGE ( 'NONE', *, *, #19091, .T. ) ;
#5325 = CARTESIAN_POINT ( 'NONE',  ( -10.45000000000000462, 12.50000000000000000, -2.230156782645135394 ) ) ;
#5326 = ORIENTED_EDGE ( 'NONE', *, *, #124740, .T. ) ;
#5327 = ADVANCED_FACE ( 'NONE', ( #95783 ), #25865, .T. ) ;
#5328 = FACE_OUTER_BOUND ( 'NONE', #22977, .T. ) ;
#5329 = CARTESIAN_POINT ( 'NONE',  ( 108.0000000000000142, 8.500000000000000000, 0.000000000000000000 ) ) ;
#5330 = ORIENTED_EDGE ( 'NONE', *, *, #51787, .T. ) ;
#5331 = CARTESIAN_POINT ( 'NONE',  ( -14.39999999999998614, 12.50000000000000000, -0.4115034346978134749 ) ) ;
#5332 = CARTESIAN_POINT ( 'NONE',  ( -3.550000000000027356, 12.50000000000000000, 1.818653347947321475 ) ) ;
#5333 = PLANE ( 'NONE',  #45106 ) ;
#5334 = PLANE ( 'NONE',  #109273 ) ;
#5335 = CARTESIAN_POINT ( 'NONE',  ( -8.750000000000010658, 2.500000000000000000, 2.957883832488649389 ) ) ;
#5336 = CARTESIAN_POINT ( 'NONE',  ( 1.249999999999952038, 2.500000000000000000, 2.757883832488649656 ) ) ;
#5337 = EDGE_CURVE ( 'NONE', #50344, #10471, #82309, .T. ) ;
#5338 = CARTESIAN_POINT ( 'NONE',  ( 186.6510416670080872, 4.367472073101518859, -7.564683531249999149 ) ) ;
#5339 = DIRECTION ( 'NONE',  ( -0.000000000000000000, -1.000000000000000000, -0.000000000000000000 ) ) ;
#5340 = AXIS2_PLACEMENT_3D ( 'NONE', #125727, #67438, #47198 ) ;
#5341 = CARTESIAN_POINT ( 'NONE',  ( 13.34999999999990017, 2.500000000000000000, 1.472243186433545459 ) ) ;
#5342 = ORIENTED_EDGE ( 'NONE', *, *, #125933, .F. ) ;
#5343 = VERTEX_POINT ( 'NONE', #83400 ) ;
#5344 = DIRECTION ( 'NONE',  ( 0.000000000000000000, -0.000000000000000000, 1.000000000000000000 ) ) ;
#5345 = ORIENTED_EDGE ( 'NONE', *, *, #110778, .T. ) ;
#5346 = DIRECTION ( 'NONE',  ( 0.000000000000000000, 0.000000000000000000, 1.000000000000000000 ) ) ;
#5348 = ORIENTED_EDGE ( 'NONE', *, *, #37774, .T. ) ;
#5347 = ORIENTED_EDGE ( 'NONE', *, *, #99969, .T. ) ;
#5349 = AXIS2_PLACEMENT_3D ( 'NONE', #25606, #85184, #83268 ) ;
#5350 = ORIENTED_EDGE ( 'NONE', *, *, #118188, .T. ) ;
#5351 = DIRECTION ( 'NONE',  ( 0.000000000000000000, 0.000000000000000000, 1.000000000000000000 ) ) ;
#5352 = CONICAL_SURFACE ( 'NONE', #1153, 0.1000000000000002554, 0.003490658503988666988 ) ;
#5353 = AXIS2_PLACEMENT_3D ( 'NONE', #77578, #79537, #117485 ) ;
#5354 = CARTESIAN_POINT ( 'NONE',  ( -14.34999999999998543, 2.500000000000000000, -1.818653347947323695 ) ) ;
#5355 = EDGE_CURVE ( 'NONE', #109519, #64213, #8663, .T. ) ;
#5356 = DIRECTION ( 'NONE',  ( 0.000000000000000000, 0.000000000000000000, 1.000000000000000000 ) ) ;
#5357 = CARTESIAN_POINT ( 'NONE',  ( -10.65000000000000213, 2.500000000000000000, 2.411473670974873862 ) ) ;
#5358 = LINE ( 'NONE', #115290, #64269 ) ;
#5359 = ORIENTED_EDGE ( 'NONE', *, *, #13084, .T. ) ;
#5360 = CARTESIAN_POINT ( 'NONE',  ( 11.44999999999990514, 12.50000000000000000, -6.213873640053564351 ) ) ;
#5361 = ORIENTED_EDGE ( 'NONE', *, *, #43244, .T. ) ;
#5362 = CONICAL_SURFACE ( 'NONE', #95265, 0.09999999999999982514, 0.003490658503988666988 ) ;
#5363 = EDGE_CURVE ( 'NONE', #80231, #80146, #99005, .T. ) ;
#5364 = ORIENTED_EDGE ( 'NONE', *, *, #19444, .F. ) ;
#5365 = ORIENTED_EDGE ( 'NONE', *, *, #71201, .F. ) ;
#5366 = CARTESIAN_POINT ( 'NONE',  ( 11.04999999999991189, 12.50000000000000000, -2.511473670974877948 ) ) ;
#5367 = EDGE_CURVE ( 'NONE', #88198, #123035, #44652, .T. ) ;
#5368 = ORIENTED_EDGE ( 'NONE', *, *, #19046, .T. ) ;
#5369 = EDGE_CURVE ( 'NONE', #43040, #87465, #9334, .T. ) ;
#5370 = VERTEX_POINT ( 'NONE', #7385 ) ;
#5371 = EDGE_CURVE ( 'NONE', #128977, #114770, #40557, .T. ) ;
#5372 = ORIENTED_EDGE ( 'NONE', *, *, #1955, .F. ) ;
#5373 = EDGE_CURVE ( 'NONE', #16094, #48072, #88530, .T. ) ;
#5374 = CARTESIAN_POINT ( 'NONE',  ( 11.24999999999990585, 2.500000000000000000, 2.857883832488649301 ) ) ;
#5376 = CIRCLE ( 'NONE', #13684, 0.09999999999999982514 ) ;
#5375 = DIRECTION ( 'NONE',  ( 0.000000000000000000, 0.000000000000000000, -1.000000000000000000 ) ) ;
#5377 = CARTESIAN_POINT ( 'NONE',  ( -12.69999999999999218, 2.500000000000000000, -4.776537180435974861 ) ) ;
#5378 = AXIS2_PLACEMENT_3D ( 'NONE', #93095, #3409, #80040 ) ;
#5379 = CARTESIAN_POINT ( 'NONE',  ( -12.29999999999999538, 2.500000000000000000, 4.576537180435972019 ) ) ;
#5380 = CARTESIAN_POINT ( 'NONE',  ( -6.700000000000019718, 2.500000000000000000, -4.330127018922201643 ) ) ;
#5381 = EDGE_CURVE ( 'NONE', #108643, #69133, #27668, .T. ) ;
#5382 = CARTESIAN_POINT ( 'NONE',  ( 6.049999999999934097, 2.500000000000000000, -6.048780366869526581 ) ) ;
#5383 = ORIENTED_EDGE ( 'NONE', *, *, #102734, .F. ) ;
#5384 = EDGE_CURVE ( 'NONE', #74183, #78070, #42608, .T. ) ;
#5385 = CARTESIAN_POINT ( 'NONE',  ( -2.050000000000032685, 12.50000000000000000, -2.165063509461101710 ) ) ;
#5386 = EDGE_CURVE ( 'NONE', #109254, #126002, #36351, .T. ) ;
#5387 = ORIENTED_EDGE ( 'NONE', *, *, #73660, .T. ) ;
#5388 = FACE_OUTER_BOUND ( 'NONE', #75262, .T. ) ;
#5389 = EDGE_CURVE ( 'NONE', #60649, #91248, #57258, .T. ) ;
#5390 = ORIENTED_EDGE ( 'NONE', *, *, #26232, .F. ) ;
#5391 = CARTESIAN_POINT ( 'NONE',  ( -5.850000000000021849, 12.50000000000000000, -2.857883832488653741 ) ) ;
#5392 = ORIENTED_EDGE ( 'NONE', *, *, #73708, .T. ) ;
#5393 = ORIENTED_EDGE ( 'NONE', *, *, #15700, .F. ) ;
#5394 = EDGE_CURVE ( 'NONE', #31364, #12823, #61375, .T. ) ;
#5395 = DIRECTION ( 'NONE',  ( 0.000000000000000000, 1.000000000000000000, 0.000000000000000000 ) ) ;
#5396 = CARTESIAN_POINT ( 'NONE',  ( 17.50000000000000000, -2.500000000000000000, 0.000000000000000000 ) ) ;
#5397 = AXIS2_PLACEMENT_3D ( 'NONE', #92593, #54579, #4187 ) ;
#5399 = CARTESIAN_POINT ( 'NONE',  ( -11.64999999999999858, 2.500000000000000000, -1.472243186433546125 ) ) ;
#5398 = CIRCLE ( 'NONE', #59719, 0.06509327318403745899 ) ;
#5400 = CARTESIAN_POINT ( 'NONE',  ( -7.500000000000016875, 2.500000000000000000, 0.6928203230275494784 ) ) ;
#5401 = ORIENTED_EDGE ( 'NONE', *, *, #47169, .T. ) ;
#5402 = CARTESIAN_POINT ( 'NONE',  ( 7.499999999999961808, 2.500000000000000000, -4.430127018922202176 ) ) ;
#5403 = CARTESIAN_POINT ( 'NONE',  ( -10.40000000000000213, 12.50000000000000000, 3.637306695894644726 ) ) ;
#5404 = CARTESIAN_POINT ( 'NONE',  ( -5.650000000000023448, 2.500000000000000000, -6.148780366869526226 ) ) ;
#5405 = CARTESIAN_POINT ( 'NONE',  ( 105.0000000000000142, 8.500000000000000000, -0.2499999999999996392 ) ) ;
#5406 = DIRECTION ( 'NONE',  ( 0.000000000000000000, 0.000000000000000000, 1.000000000000000000 ) ) ;
#5407 = ORIENTED_EDGE ( 'NONE', *, *, #100584, .F. ) ;
#5408 = ORIENTED_EDGE ( 'NONE', *, *, #23703, .F. ) ;
#5409 = AXIS2_PLACEMENT_3D ( 'NONE', #91243, #89943, #40214 ) ;
#5410 = ORIENTED_EDGE ( 'NONE', *, *, #22969, .F. ) ;
#5411 = VECTOR ( 'NONE', #46133, 1000.000000000000000 ) ;
#5412 = CARTESIAN_POINT ( 'NONE',  ( 0.7999999999999548583, 12.50000000000000000, 4.330127018922196314 ) ) ;
#5414 = AXIS2_PLACEMENT_3D ( 'NONE', #127686, #60266, #88390 ) ;
#5413 = DIRECTION ( 'NONE',  ( 0.000000000000000000, 1.000000000000000000, 0.000000000000000000 ) ) ;
#5415 = AXIS2_PLACEMENT_3D ( 'NONE', #54207, #124236, #43758 ) ;
#5416 = CARTESIAN_POINT ( 'NONE',  ( 184.2968750003414300, 8.734944146203032389, 5.348610694689227483E-16 ) ) ;
#5417 = CARTESIAN_POINT ( 'NONE',  ( 7.499999999999925393, 12.50000000000000000, -0.6277270498435166823 ) ) ;
#5418 = DIRECTION ( 'NONE',  ( 0.000000000000000000, 1.000000000000000000, 0.000000000000000000 ) ) ;
#5419 = CARTESIAN_POINT ( 'NONE',  ( 13.29999999999990301, 12.50000000000000000, -4.395220292106239768 ) ) ;
#5420 = CARTESIAN_POINT ( 'NONE',  ( 9.399999999999915090, 12.50000000000000000, -4.048810130592463530 ) ) ;
#5421 = ORIENTED_EDGE ( 'NONE', *, *, #48546, .F. ) ;
#5422 = ADVANCED_FACE ( 'NONE', ( #78080 ), #30088, .T. ) ;
#5423 = DIRECTION ( 'NONE',  ( -0.000000000000000000, 1.000000000000000000, -0.000000000000000000 ) ) ;
#5424 = DIRECTION ( 'NONE',  ( 0.000000000000000000, 0.000000000000000000, 1.000000000000000000 ) ) ;
#5425 = EDGE_CURVE ( 'NONE', #106738, #8949, #13324, .T. ) ;
#5426 = ORIENTED_EDGE ( 'NONE', *, *, #104379, .F. ) ;
#5427 = CARTESIAN_POINT ( 'NONE',  ( 3.949999999999938893, 2.500000000000000000, 6.248780366869520542 ) ) ;
#5428 = CIRCLE ( 'NONE', #107846, 0.06509327318403745899 ) ;
#5429 = DIRECTION ( 'NONE',  ( -0.000000000000000000, 1.000000000000000000, -0.000000000000000000 ) ) ;
#5430 = DIRECTION ( 'NONE',  ( 0.000000000000000000, 1.000000000000000000, 0.000000000000000000 ) ) ;
#5431 = ORIENTED_EDGE ( 'NONE', *, *, #128653, .F. ) ;
#5432 = DIRECTION ( 'NONE',  ( -0.000000000000000000, -1.000000000000000000, -0.000000000000000000 ) ) ;
#5433 = AXIS2_PLACEMENT_3D ( 'NONE', #62822, #113189, #13043 ) ;
#5434 = ORIENTED_EDGE ( 'NONE', *, *, #114585, .F. ) ;
#5435 = DIRECTION ( 'NONE',  ( 0.000000000000000000, 1.000000000000000000, 0.000000000000000000 ) ) ;
#5436 = CARTESIAN_POINT ( 'NONE',  ( 2.299999999999948752, 12.50000000000000000, -4.048810130592463530 ) ) ;
#5437 = FACE_OUTER_BOUND ( 'NONE', #80381, .T. ) ;
#5438 = CONICAL_SURFACE ( 'NONE', #89085, 0.1000000000000000056, 0.003490658503988666988 ) ;
#5439 = AXIS2_PLACEMENT_3D ( 'NONE', #46696, #66324, #95792 ) ;
#5440 = EDGE_LOOP ( 'NONE', ( #82980, #17495, #65727, #30628 ) ) ;
#5441 = VECTOR ( 'NONE', #109964, 1000.000000000000000 ) ;
#5442 = DIRECTION ( 'NONE',  ( 0.000000000000000000, 0.000000000000000000, -1.000000000000000000 ) ) ;
#5443 = EDGE_LOOP ( 'NONE', ( #25934, #36081, #118557, #2574 ) ) ;
#5445 = AXIS2_PLACEMENT_3D ( 'NONE', #446, #77722, #87550 ) ;
#5444 = CARTESIAN_POINT ( 'NONE',  ( -12.49999999999999289, 2.500000000000000000, -4.922947341949750921 ) ) ;
#5446 = EDGE_LOOP ( 'NONE', ( #33661, #95263 ) ) ;
#5448 = AXIS2_PLACEMENT_3D ( 'NONE', #6276, #103213, #13531 ) ;
#5447 = AXIS2_PLACEMENT_3D ( 'NONE', #83761, #114500, #82490 ) ;
#5449 = ORIENTED_EDGE ( 'NONE', *, *, #83683, .F. ) ;
#5450 = CARTESIAN_POINT ( 'NONE',  ( -11.44999999999999751, 12.50000000000000000, -6.841600689897074261 ) ) ;
#5451 = LINE ( 'NONE', #44756, #81385 ) ;
#5452 = VERTEX_POINT ( 'NONE', #47986 ) ;
#5453 = DIRECTION ( 'NONE',  ( -0.000000000000000000, -1.000000000000000000, -0.000000000000000000 ) ) ;
#5454 = CARTESIAN_POINT ( 'NONE',  ( -7.100000000000017408, 12.50000000000000000, 0.6928203230275494784 ) ) ;
#5455 = EDGE_LOOP ( 'NONE', ( #4785, #9220 ) ) ;
#5457 = EDGE_CURVE ( 'NONE', #11223, #14873, #813, .T. ) ;
#5456 = DIRECTION ( 'NONE',  ( 0.000000000000000000, 0.000000000000000000, 1.000000000000000000 ) ) ;
#5458 = DIRECTION ( 'NONE',  ( -0.000000000000000000, 1.000000000000000000, -0.000000000000000000 ) ) ;
#5459 = FACE_OUTER_BOUND ( 'NONE', #232, .T. ) ;
#5460 = DIRECTION ( 'NONE',  ( 0.000000000000000000, 0.000000000000000000, -1.000000000000000000 ) ) ;
#5461 = DIRECTION ( 'NONE',  ( 0.000000000000000000, -0.9999939076577903929, 0.003490651415223739937 ) ) ;
#5462 = DIRECTION ( 'NONE',  ( -0.000000000000000000, -1.000000000000000000, -0.000000000000000000 ) ) ;
#5463 = ORIENTED_EDGE ( 'NONE', *, *, #4933, .F. ) ;
#5464 = VERTEX_POINT ( 'NONE', #126541 ) ;
#5465 = ORIENTED_EDGE ( 'NONE', *, *, #43572, .T. ) ;
#5466 = ORIENTED_EDGE ( 'NONE', *, *, #19965, .F. ) ;
#5467 = CARTESIAN_POINT ( 'NONE',  ( 43.29488422903774847, 3.510951914389877526, 3.940494739282152992 ) ) ;
#5468 = DIRECTION ( 'NONE',  ( 0.000000000000000000, 0.000000000000000000, 1.000000000000000000 ) ) ;
#5469 = EDGE_CURVE ( 'NONE', #51819, #118832, #84447, .T. ) ;
#5470 = DIRECTION ( 'NONE',  ( -0.000000000000000000, -1.000000000000000000, -0.000000000000000000 ) ) ;
#5471 = ORIENTED_EDGE ( 'NONE', *, *, #73353, .F. ) ;
#5472 = FACE_BOUND ( 'NONE', #62179, .T. ) ;
#5473 = ADVANCED_FACE ( 'NONE', ( #117991 ), #108335, .T. ) ;
#5474 = DIRECTION ( 'NONE',  ( -0.000000000000000000, -1.000000000000000000, -0.000000000000000000 ) ) ;
#5475 = CARTESIAN_POINT ( 'NONE',  ( 4.999999999999936939, 12.50000000000000000, -3.637306695894650055 ) ) ;
#5476 = CARTESIAN_POINT ( 'NONE',  ( -1.650000000000034772, 2.500000000000000000, 2.065063509461097624 ) ) ;
#5477 = CIRCLE ( 'NONE', #91179, 0.1000000000000002554 ) ;
#5478 = CARTESIAN_POINT ( 'NONE',  ( -8.350000000000012079, 2.500000000000000000, -2.857883832488653741 ) ) ;
#5479 = CARTESIAN_POINT ( 'NONE',  ( -3.642919299551294898E-14, 2.500000000000000000, 0.6928203230275518099 ) ) ;
#5480 = DIRECTION ( 'NONE',  ( -0.000000000000000000, -1.000000000000000000, -0.000000000000000000 ) ) ;
#5481 = CARTESIAN_POINT ( 'NONE',  ( 0.000000000000000000, 12.50000000000000000, 0.06509327318403743123 ) ) ;
#5482 = DIRECTION ( 'NONE',  ( 0.000000000000000000, 0.000000000000000000, 1.000000000000000000 ) ) ;
#5483 = EDGE_CURVE ( 'NONE', #11815, #117684, #47339, .T. ) ;
#5484 = CARTESIAN_POINT ( 'NONE',  ( -0.6000000000000383915, 2.500000000000000000, -3.883716857408426648 ) ) ;
#5485 = DIRECTION ( 'NONE',  ( 0.000000000000000000, -0.9999939076577903929, 0.003490651415223739937 ) ) ;
#5487 = CIRCLE ( 'NONE', #72413, 0.09999999999999982514 ) ;
#5486 = VECTOR ( 'NONE', #124407, 1000.000000000000000 ) ;
#5488 = ORIENTED_EDGE ( 'NONE', *, *, #115000, .F. ) ;
#5489 = VERTEX_POINT ( 'NONE', #28341 ) ;
#5490 = VERTEX_POINT ( 'NONE', #8033 ) ;
#5491 = ORIENTED_EDGE ( 'NONE', *, *, #24041, .F. ) ;
#5492 = CARTESIAN_POINT ( 'NONE',  ( 7.899999999999924860, 2.500000000000000000, 5.022947341949748790 ) ) ;
#5493 = ORIENTED_EDGE ( 'NONE', *, *, #83409, .F. ) ;
#5494 = DIRECTION ( 'NONE',  ( -0.000000000000000000, 1.000000000000000000, -0.000000000000000000 ) ) ;
#5495 = ORIENTED_EDGE ( 'NONE', *, *, #9273, .F. ) ;
#5496 = VERTEX_POINT ( 'NONE', #58452 ) ;
#5497 = CARTESIAN_POINT ( 'NONE',  ( 9.549999999999915445, 2.500000000000000000, 6.595190528383296780 ) ) ;
#5499 = AXIS2_PLACEMENT_3D ( 'NONE', #64216, #56321, #123766 ) ;
#5498 = CIRCLE ( 'NONE', #55683, 0.1000000000000000472 ) ;
#5500 = CARTESIAN_POINT ( 'NONE',  ( 8.920123399940051101, -2.500000000000000444, 8.410822907403851190 ) ) ;
#5501 = CARTESIAN_POINT ( 'NONE',  ( 6.249999999999932498, 12.50000000000000000, -2.922977105672691422 ) ) ;
#5502 = DIRECTION ( 'NONE',  ( 0.000000000000000000, 1.000000000000000000, 0.000000000000000000 ) ) ;
#5503 = CARTESIAN_POINT ( 'NONE',  ( -4.400000000000025224, 12.50000000000000000, 0.2813168883297361700 ) ) ;
#5504 = VERTEX_POINT ( 'NONE', #89186 ) ;
#5505 = ORIENTED_EDGE ( 'NONE', *, *, #127912, .T. ) ;
#5506 = ADVANCED_FACE ( 'NONE', ( #39470 ), #79377, .T. ) ;
#5507 = ORIENTED_EDGE ( 'NONE', *, *, #118386, .F. ) ;
#5509 = ORIENTED_EDGE ( 'NONE', *, *, #6716, .F. ) ;
#5508 = CARTESIAN_POINT ( 'NONE',  ( 14.14999999999989377, 2.500000000000000000, -1.572243186433550211 ) ) ;
#5510 = CARTESIAN_POINT ( 'NONE',  ( -10.00000000000000711, 12.50000000000000000, -3.637306695894645614 ) ) ;
#5511 = ORIENTED_EDGE ( 'NONE', *, *, #12211, .T. ) ;
#5512 = ADVANCED_FACE ( 'NONE', ( #70193 ), #71465, .T. ) ;
#5513 = VECTOR ( 'NONE', #87593, 1000.000000000000000 ) ;
#5514 = ORIENTED_EDGE ( 'NONE', *, *, #64965, .F. ) ;
#5515 = EDGE_CURVE ( 'NONE', #74476, #93079, #41558, .T. ) ;
#5516 = PLANE ( 'NONE',  #67287 ) ;
#5517 = DIRECTION ( 'NONE',  ( 0.000000000000000000, 0.000000000000000000, 1.000000000000000000 ) ) ;
#5518 = LINE ( 'NONE', #26475, #95968 ) ;
#5519 = CIRCLE ( 'NONE', #64029, 0.06509327318403745899 ) ;
#5520 = FACE_OUTER_BOUND ( 'NONE', #107670, .T. ) ;
#5521 = EDGE_CURVE ( 'NONE', #74712, #2890, #70780, .T. ) ;
#5522 = ADVANCED_FACE ( 'NONE', ( #121220 ), #120951, .T. ) ;
#5523 = DIRECTION ( 'NONE',  ( 0.000000000000000000, -0.9999939076577903929, 0.003490651415223739937 ) ) ;
#5524 = AXIS2_PLACEMENT_3D ( 'NONE', #65380, #105321, #63467 ) ;
#5525 = DIRECTION ( 'NONE',  ( 0.000000000000000000, 1.000000000000000000, 0.000000000000000000 ) ) ;
#5526 = EDGE_CURVE ( 'NONE', #93332, #51670, #51211, .T. ) ;
#5527 = CONICAL_SURFACE ( 'NONE', #49482, 0.1000000000000002554, 0.003490658503988666988 ) ;
#5528 = EDGE_CURVE ( 'NONE', #53090, #88981, #16370, .T. ) ;
#5529 = ORIENTED_EDGE ( 'NONE', *, *, #88308, .F. ) ;
#5531 = AXIS2_PLACEMENT_3D ( 'NONE', #87883, #67606, #9346 ) ;
#5530 = DIRECTION ( 'NONE',  ( -0.000000000000000000, -1.000000000000000000, -0.000000000000000000 ) ) ;
#5532 = EDGE_LOOP ( 'NONE', ( #127885, #101640, #123823, #118707 ) ) ;
#5533 = CONICAL_SURFACE ( 'NONE', #80781, 0.1000000000000000472, 0.003490658503988666988 ) ;
#5534 = CARTESIAN_POINT ( 'NONE',  ( -0.4000000000000404898, 12.50000000000000000, 5.022947341949748790 ) ) ;
#5535 = EDGE_CURVE ( 'NONE', #123894, #69676, #2725, .T. ) ;
#5536 = VERTEX_POINT ( 'NONE', #121863 ) ;
#5537 = DIRECTION ( 'NONE',  ( 0.000000000000000000, 1.000000000000000000, 0.000000000000000000 ) ) ;
#5538 = DIRECTION ( 'NONE',  ( 0.000000000000000000, 0.000000000000000000, 1.000000000000000000 ) ) ;
#5539 = EDGE_LOOP ( 'NONE', ( #103673, #78625 ) ) ;
#5540 = DIRECTION ( 'NONE',  ( 0.000000000000000000, 0.000000000000000000, 1.000000000000000000 ) ) ;
#5541 = CARTESIAN_POINT ( 'NONE',  ( -7.499999999999980460, 2.500000000000000000, -4.330127018922201643 ) ) ;
#5542 = ORIENTED_EDGE ( 'NONE', *, *, #119028, .F. ) ;
#5543 = EDGE_CURVE ( 'NONE', #56755, #102028, #83321, .T. ) ;
#5544 = AXIS2_PLACEMENT_3D ( 'NONE', #28657, #68557, #108483 ) ;
#5545 = CARTESIAN_POINT ( 'NONE',  ( -5.850000000000022737, 2.500000000000000000, -6.495190528383302464 ) ) ;
#5547 = VECTOR ( 'NONE', #26280, 1000.000000000000000 ) ;
#5546 = AXIS2_PLACEMENT_3D ( 'NONE', #100033, #41129, #49012 ) ;
#5548 = CARTESIAN_POINT ( 'NONE',  ( -13.14999999999999147, 2.500000000000000000, -2.511473670974875727 ) ) ;
#5549 = EDGE_LOOP ( 'NONE', ( #109464, #5364 ) ) ;
#5550 = VERTEX_POINT ( 'NONE', #60393 ) ;
#5551 = ORIENTED_EDGE ( 'NONE', *, *, #18503, .F. ) ;
#5552 = DIRECTION ( 'NONE',  ( 0.000000000000000000, -0.000000000000000000, 1.000000000000000000 ) ) ;
#5553 = CARTESIAN_POINT ( 'NONE',  ( 0.4499999999999569344, 2.500000000000000000, -2.165063509461101710 ) ) ;
#5554 = CARTESIAN_POINT ( 'NONE',  ( 184.6093750003413732, 9.264065473108010111E-16, -7.564683531250000925 ) ) ;
#5555 = CARTESIAN_POINT ( 'NONE',  ( -3.100000000000028955, 2.500000000000000000, 3.883716857408421319 ) ) ;
#5556 = FACE_OUTER_BOUND ( 'NONE', #114193, .T. ) ;
#5557 = CARTESIAN_POINT ( 'NONE',  ( 12.09999999999990550, 12.50000000000000000, -3.637306695894650055 ) ) ;
#5558 = ORIENTED_EDGE ( 'NONE', *, *, #35698, .F. ) ;
#5559 = CARTESIAN_POINT ( 'NONE',  ( 14.99999999999989342, 12.50000000000000000, -0.6928203230275541413 ) ) ;
#5560 = EDGE_LOOP ( 'NONE', ( #90102, #83229 ) ) ;
#5561 = DIRECTION ( 'NONE',  ( 0.000000000000000000, 0.000000000000000000, -1.000000000000000000 ) ) ;
#5562 = LINE ( 'NONE', #46147, #4688 ) ;
#5563 = DIRECTION ( 'NONE',  ( 0.000000000000000000, 1.000000000000000000, 0.000000000000000000 ) ) ;
#5564 = ORIENTED_EDGE ( 'NONE', *, *, #90344, .F. ) ;
#5565 = EDGE_CURVE ( 'NONE', #126422, #97481, #24812, .T. ) ;
#5566 = VECTOR ( 'NONE', #66745, 1000.000000000000000 ) ;
#5567 = DIRECTION ( 'NONE',  ( 0.000000000000000000, 0.000000000000000000, 1.000000000000000000 ) ) ;
#5568 = CARTESIAN_POINT ( 'NONE',  ( -12.69999999999999218, 2.500000000000000000, -0.3464101615137741286 ) ) ;
#5569 = ORIENTED_EDGE ( 'NONE', *, *, #56895, .T. ) ;
#5570 = AXIS2_PLACEMENT_3D ( 'NONE', #66478, #85484, #109477 ) ;
#5571 = DIRECTION ( 'NONE',  ( -0.000000000000000000, -1.000000000000000000, -0.000000000000000000 ) ) ;
#5572 = ADVANCED_FACE ( 'NONE', ( #90455 ), #58271, .T. ) ;
#5573 = ORIENTED_EDGE ( 'NONE', *, *, #25416, .F. ) ;
#5574 = ORIENTED_EDGE ( 'NONE', *, *, #47275, .T. ) ;
#5575 = DIRECTION ( 'NONE',  ( 0.000000000000000000, 0.000000000000000000, -1.000000000000000000 ) ) ;
#5576 = VECTOR ( 'NONE', #104191, 1000.000000000000000 ) ;
#5577 = EDGE_LOOP ( 'NONE', ( #53434, #67594, #88455, #29839 ) ) ;
#5578 = DIRECTION ( 'NONE',  ( 0.000000000000000000, 0.000000000000000000, -1.000000000000000000 ) ) ;
#5579 = CARTESIAN_POINT ( 'NONE',  ( -7.499999999999976907, 2.500000000000000000, 4.230127018922196669 ) ) ;
#5581 = AXIS2_PLACEMENT_3D ( 'NONE', #17009, #127024, #119125 ) ;
#5580 = CIRCLE ( 'NONE', #72519, 0.1000000000000000472 ) ;
#5582 = CARTESIAN_POINT ( 'NONE',  ( -12.49999999999995737, 2.500000000000000000, 4.330127018922196314 ) ) ;
#5583 = EDGE_LOOP ( 'NONE', ( #28892, #44647, #32509, #111013 ) ) ;
#5584 = CONICAL_SURFACE ( 'NONE', #85016, 0.1000000000000002554, 0.003490658503988666988 ) ;
#5585 = FACE_BOUND ( 'NONE', #41124, .T. ) ;
#5587 = ORIENTED_EDGE ( 'NONE', *, *, #27303, .F. ) ;
#5586 = DIRECTION ( 'NONE',  ( 0.000000000000000000, -0.9999939076577903929, 0.003490651415223739937 ) ) ;
#5588 = DIRECTION ( 'NONE',  ( 0.000000000000000000, 0.000000000000000000, 1.000000000000000000 ) ) ;
#5589 = CARTESIAN_POINT ( 'NONE',  ( -12.29999999999999538, 2.500000000000000000, -4.676537180435976104 ) ) ;
#5590 = EDGE_LOOP ( 'NONE', ( #74348, #85355 ) ) ;
#5591 = ORIENTED_EDGE ( 'NONE', *, *, #38964, .T. ) ;
#5592 = EDGE_LOOP ( 'NONE', ( #31315, #68551, #67878, #8634 ) ) ;
#5593 = DIRECTION ( 'NONE',  ( 0.000000000000000000, -0.000000000000000000, 1.000000000000000000 ) ) ;
#5594 = DIRECTION ( 'NONE',  ( 0.000000000000000000, 0.000000000000000000, -1.000000000000000000 ) ) ;
#5595 = DIRECTION ( 'NONE',  ( -0.000000000000000000, -1.000000000000000000, -0.000000000000000000 ) ) ;
#5596 = FACE_BOUND ( 'NONE', #58620, .T. ) ;
#5597 = EDGE_LOOP ( 'NONE', ( #10928, #123348 ) ) ;
#5598 = AXIS2_PLACEMENT_3D ( 'NONE', #25964, #75058, #63951 ) ;
#5599 = CARTESIAN_POINT ( 'NONE',  ( 186.6093750003414016, 9.264065473108010111E-16, -7.564683531250000925 ) ) ;
#5600 = AXIS2_PLACEMENT_3D ( 'NONE', #66825, #65552, #36758 ) ;
#5601 = CARTESIAN_POINT ( 'NONE',  ( -7.050000000000016698, 2.500000000000000000, -2.065063509461102065 ) ) ;
#5602 = CARTESIAN_POINT ( 'NONE',  ( 2.099999999999948574, 2.500000000000000000, 4.430127018922196847 ) ) ;
#5603 = AXIS2_PLACEMENT_3D ( 'NONE', #100966, #11296, #51252 ) ;
#5604 = ADVANCED_FACE ( 'NONE', ( #51849 ), #49928, .T. ) ;
#5605 = DIRECTION ( 'NONE',  ( -0.000000000000000000, -1.000000000000000000, -0.000000000000000000 ) ) ;
#5606 = AXIS2_PLACEMENT_3D ( 'NONE', #104923, #15247, #5442 ) ;
#5607 = LINE ( 'NONE', #46856, #61114 ) ;
#5608 = PLANE ( 'NONE',  #75805 ) ;
#5609 = CARTESIAN_POINT ( 'NONE',  ( 0.8499999999999553468, 12.50000000000000000, -2.922977105672691422 ) ) ;
#5610 = VECTOR ( 'NONE', #117501, 1000.000000000000000 ) ;
#5611 = CARTESIAN_POINT ( 'NONE',  ( 16.55874544816223448, 0.4845305829267578801, 6.091953208799004926 ) ) ;
#5612 = CONICAL_SURFACE ( 'NONE', #110096, 0.1000000000000002554, 0.003490658503988666988 ) ;
#5613 = EDGE_CURVE ( 'NONE', #49210, #10571, #87490, .T. ) ;
#5614 = FACE_OUTER_BOUND ( 'NONE', #128737, .T. ) ;
#5615 = AXIS2_PLACEMENT_3D ( 'NONE', #21704, #1400, #109432 ) ;
#5616 = ORIENTED_EDGE ( 'NONE', *, *, #14550, .T. ) ;
#5617 = ORIENTED_EDGE ( 'NONE', *, *, #118129, .T. ) ;
#5618 = VERTEX_POINT ( 'NONE', #9980 ) ;
#5619 = EDGE_LOOP ( 'NONE', ( #118635, #70062, #16081, #106205 ) ) ;
#5620 = EDGE_LOOP ( 'NONE', ( #50477, #23687 ) ) ;
#5621 = DIRECTION ( 'NONE',  ( 0.000000000000000000, 0.000000000000000000, 1.000000000000000000 ) ) ;
#5622 = EDGE_CURVE ( 'NONE', #94894, #40952, #2078, .T. ) ;
#5623 = PLANE ( 'NONE',  #4816 ) ;
#5624 = AXIS2_PLACEMENT_3D ( 'NONE', #127701, #8554, #77955 ) ;
#5625 = ORIENTED_EDGE ( 'NONE', *, *, #89977, .T. ) ;
#5626 = FACE_BOUND ( 'NONE', #115042, .T. ) ;
#5627 = ADVANCED_FACE ( 'NONE', ( #42022 ), #100035, .T. ) ;
#5629 = LINE ( 'NONE', #122845, #8057 ) ;
#5628 = CIRCLE ( 'NONE', #55822, 0.06509327318403745899 ) ;
#5631 = AXIS2_PLACEMENT_3D ( 'NONE', #113858, #96770, #86964 ) ;
#5630 = AXIS2_PLACEMENT_3D ( 'NONE', #65238, #105173, #85538 ) ;
#5632 = EDGE_CURVE ( 'NONE', #41715, #21708, #40756, .T. ) ;
#5633 = CARTESIAN_POINT ( 'NONE',  ( -7.700000000000016165, 12.50000000000000000, -3.983716857408426293 ) ) ;
#5634 = EDGE_LOOP ( 'NONE', ( #12952, #108098, #38152, #117411 ) ) ;
#5635 = PLANE ( 'NONE',  #128998 ) ;
#5636 = CARTESIAN_POINT ( 'NONE',  ( 11.64999999999990443, 12.50000000000000000, 2.857883832488649301 ) ) ;
#5637 = ADVANCED_FACE ( 'NONE', ( #22398 ), #110953, .T. ) ;
#5638 = LINE ( 'NONE', #64566, #32947 ) ;
#5639 = EDGE_LOOP ( 'NONE', ( #69738, #28016 ) ) ;
#5640 = CARTESIAN_POINT ( 'NONE',  ( 0.6499999999999561684, 2.500000000000000000, 2.611473670974873151 ) ) ;
#5641 = ORIENTED_EDGE ( 'NONE', *, *, #122178, .T. ) ;
#5642 = ORIENTED_EDGE ( 'NONE', *, *, #19648, .T. ) ;
#5643 = ORIENTED_EDGE ( 'NONE', *, *, #102488, .F. ) ;
#5644 = FACE_OUTER_BOUND ( 'NONE', #22816, .T. ) ;
#5645 = DIRECTION ( 'NONE',  ( 0.000000000000000000, -0.9999939076577903929, 0.003490651415223739937 ) ) ;
#5646 = CARTESIAN_POINT ( 'NONE',  ( -7.500000000000016875, 2.500000000000000000, -3.637306695894650055 ) ) ;
#5647 = ORIENTED_EDGE ( 'NONE', *, *, #47338, .F. ) ;
#5648 = CIRCLE ( 'NONE', #110126, 0.06509327318403745899 ) ;
#5649 = CARTESIAN_POINT ( 'NONE',  ( 14.93814515115542640, 2.500000000000000444, -6.173787963789177269 ) ) ;
#5650 = FACE_OUTER_BOUND ( 'NONE', #97587, .T. ) ;
#5651 = CARTESIAN_POINT ( 'NONE',  ( -1.050000000000037792, 2.500000000000000000, 1.718653347947321386 ) ) ;
#5652 = CARTESIAN_POINT ( 'NONE',  ( 186.8593750003414016, 0.000000000000000000, 7.564683531250000925 ) ) ;
#5653 = CARTESIAN_POINT ( 'NONE',  ( -15.59999999999998010, 12.50000000000000000, -0.2813168883297385570 ) ) ;
#5654 = DIRECTION ( 'NONE',  ( -4.274815082592931898E-19, -0.9999939076577903929, -0.003490651415223739937 ) ) ;
#5655 = ORIENTED_EDGE ( 'NONE', *, *, #26530, .F. ) ;
#5656 = DIRECTION ( 'NONE',  ( -0.000000000000000000, 1.000000000000000000, -0.000000000000000000 ) ) ;
#5657 = CONICAL_SURFACE ( 'NONE', #87144, 0.09999999999999982514, 0.003490658503988666988 ) ;
#5658 = ORIENTED_EDGE ( 'NONE', *, *, #84490, .T. ) ;
#5659 = VECTOR ( 'NONE', #97824, 1000.000000000000000 ) ;
#5660 = ORIENTED_EDGE ( 'NONE', *, *, #38584, .F. ) ;
#5661 = FACE_OUTER_BOUND ( 'NONE', #127077, .T. ) ;
#5662 = CARTESIAN_POINT ( 'NONE',  ( -10.80000000000000071, 12.50000000000000000, -0.06509327318403970719 ) ) ;
#5663 = DIRECTION ( 'NONE',  ( -0.000000000000000000, 1.000000000000000000, -0.000000000000000000 ) ) ;
#5664 = DIRECTION ( 'NONE',  ( -0.000000000000000000, -1.000000000000000000, -0.000000000000000000 ) ) ;
#5665 = EDGE_LOOP ( 'NONE', ( #1876, #2474, #35663, #9585 ) ) ;
#5669 = EDGE_CURVE ( 'NONE', #83259, #61624, #43609, .T. ) ;
#5668 = ORIENTED_EDGE ( 'NONE', *, *, #87969, .F. ) ;
#5667 = AXIS2_PLACEMENT_3D ( 'NONE', #39891, #58867, #98137 ) ;
#5666 = AXIS2_PLACEMENT_3D ( 'NONE', #76590, #66117, #96211 ) ;
#5670 = FACE_OUTER_BOUND ( 'NONE', #95957, .T. ) ;
#5671 = LINE ( 'NONE', #45633, #64136 ) ;
#5673 = EDGE_CURVE ( 'NONE', #124518, #87255, #18459, .T. ) ;
#5672 = CARTESIAN_POINT ( 'NONE',  ( -5.400000000000023448, 12.50000000000000000, -4.265033745738164406 ) ) ;
#5674 = EDGE_LOOP ( 'NONE', ( #34941, #64826, #29441, #115671 ) ) ;
#5675 = EDGE_LOOP ( 'NONE', ( #114849, #35240, #55808, #8326 ) ) ;
#5676 = EDGE_CURVE ( 'NONE', #119267, #40041, #12177, .T. ) ;
#5677 = DIRECTION ( 'NONE',  ( 0.000000000000000000, 0.000000000000000000, 1.000000000000000000 ) ) ;
#5678 = ADVANCED_FACE ( 'NONE', ( #70044 ), #74904, .T. ) ;
#5681 = EDGE_CURVE ( 'NONE', #40822, #9001, #85359, .T. ) ;
#5680 = VECTOR ( 'NONE', #63427, 1000.000000000000000 ) ;
#5679 = AXIS2_PLACEMENT_3D ( 'NONE', #41665, #81564, #72401 ) ;
#5682 = VERTEX_POINT ( 'NONE', #60243 ) ;
#5683 = CARTESIAN_POINT ( 'NONE',  ( -1.450000000000035483, 2.500000000000000000, 6.048780366869521252 ) ) ;
#5684 = AXIS2_PLACEMENT_3D ( 'NONE', #31576, #72791, #115248 ) ;
#5685 = DIRECTION ( 'NONE',  ( -0.000000000000000000, -1.000000000000000000, -0.000000000000000000 ) ) ;
#5686 = ORIENTED_EDGE ( 'NONE', *, *, #82605, .F. ) ;
#5687 = DIRECTION ( 'NONE',  ( 0.000000000000000000, -0.9999939076577903929, 0.003490651415223739937 ) ) ;
#5688 = EDGE_CURVE ( 'NONE', #18148, #59490, #22243, .T. ) ;
#5689 = DIRECTION ( 'NONE',  ( 0.000000000000000000, 1.000000000000000000, 0.000000000000000000 ) ) ;
#5690 = CARTESIAN_POINT ( 'NONE',  ( 9.999999999999912959, 12.50000000000000000, -5.022947341949754119 ) ) ;
#5691 = DIRECTION ( 'NONE',  ( 0.000000000000000000, 1.000000000000000000, 0.000000000000000000 ) ) ;
#5692 = ORIENTED_EDGE ( 'NONE', *, *, #7555, .T. ) ;
#5693 = EDGE_CURVE ( 'NONE', #73131, #69690, #79116, .T. ) ;
#5694 = CARTESIAN_POINT ( 'NONE',  ( -1.050000000000038680, 2.500000000000000000, 6.941600689897073018 ) ) ;
#5695 = ADVANCED_FACE ( 'NONE', ( #640 ), #45665, .T. ) ;
#5696 = CARTESIAN_POINT ( 'NONE',  ( -13.54999999999998828, 12.50000000000000000, 1.753560074763288013 ) ) ;
#5697 = VERTEX_POINT ( 'NONE', #80518 ) ;
#5698 = ORIENTED_EDGE ( 'NONE', *, *, #34163, .T. ) ;
#5699 = CARTESIAN_POINT ( 'NONE',  ( 184.6718750003414016, 9.264065473108010111E-16, -7.564683531250000925 ) ) ;
#5700 = CARTESIAN_POINT ( 'NONE',  ( -1.322875655532295136, -1.500000000000000222, 6.000000000000005329 ) ) ;
#5701 = DIRECTION ( 'NONE',  ( 0.000000000000000000, 0.000000000000000000, 1.000000000000000000 ) ) ;
#5702 = DIRECTION ( 'NONE',  ( -0.000000000000000000, 1.000000000000000000, -0.000000000000000000 ) ) ;
#5703 = AXIS2_PLACEMENT_3D ( 'NONE', #123040, #13706, #92940 ) ;
#5705 = AXIS2_PLACEMENT_3D ( 'NONE', #78392, #48930, #99952 ) ;
#5704 = DIRECTION ( 'NONE',  ( -4.274815082592931898E-19, -0.9999939076577903929, -0.003490651415223739937 ) ) ;
#5706 = CARTESIAN_POINT ( 'NONE',  ( -5.850000000000019185, 2.500000000000000000, 6.395190528383296602 ) ) ;
#5707 = CARTESIAN_POINT ( 'NONE',  ( 154.1524742528378056, 0.5000000000000000000, 1.703575533167231537 ) ) ;
#5708 = DIRECTION ( 'NONE',  ( -0.000000000000000000, 1.000000000000000000, -0.000000000000000000 ) ) ;
#5709 = DIRECTION ( 'NONE',  ( 0.000000000000000000, 1.000000000000000000, 0.000000000000000000 ) ) ;
#5710 = CARTESIAN_POINT ( 'NONE',  ( -5.200000000000022382, 2.500000000000000000, 0.3464101615137735735 ) ) ;
#5711 = VECTOR ( 'NONE', #51551, 1000.000000000000000 ) ;
#5712 = CARTESIAN_POINT ( 'NONE',  ( 7.949999999999925571, 2.500000000000000000, 2.165063509461097713 ) ) ;
#5713 = VERTEX_POINT ( 'NONE', #64083 ) ;
#5714 = CIRCLE ( 'NONE', #3383, 0.09999999999999982514 ) ;
#5715 = EDGE_LOOP ( 'NONE', ( #89701, #33061 ) ) ;
#5716 = EDGE_LOOP ( 'NONE', ( #89197, #62835 ) ) ;
#5717 = CIRCLE ( 'NONE', #60046, 0.1000000000000002554 ) ;
#5718 = DIRECTION ( 'NONE',  ( 0.000000000000000000, 0.000000000000000000, 1.000000000000000000 ) ) ;
#5719 = DIRECTION ( 'NONE',  ( 0.000000000000000000, 1.000000000000000000, 0.000000000000000000 ) ) ;
#5720 = VERTEX_POINT ( 'NONE', #54266 ) ;
#5721 = DIRECTION ( 'NONE',  ( 0.000000000000000000, -0.9999939076577903929, 0.003490651415223739937 ) ) ;
#5723 = VECTOR ( 'NONE', #124148, 1000.000000000000000 ) ;
#5722 = AXIS2_PLACEMENT_3D ( 'NONE', #86668, #104383, #84084 ) ;
#5724 = DIRECTION ( 'NONE',  ( 0.000000000000000000, 0.000000000000000000, 1.000000000000000000 ) ) ;
#5726 = ORIENTED_EDGE ( 'NONE', *, *, #65688, .T. ) ;
#5725 = DIRECTION ( 'NONE',  ( 0.000000000000000000, 1.000000000000000000, 0.000000000000000000 ) ) ;
#5727 = DIRECTION ( 'NONE',  ( 0.000000000000000000, -0.000000000000000000, 1.000000000000000000 ) ) ;
#5728 = EDGE_LOOP ( 'NONE', ( #91786, #44566, #127705, #72618 ) ) ;
#5729 = ADVANCED_FACE ( 'NONE', ( #103370 ), #28939, .T. ) ;
#5730 = EDGE_LOOP ( 'NONE', ( #99024, #116232, #75971, #65661 ) ) ;
#5731 = ORIENTED_EDGE ( 'NONE', *, *, #34651, .T. ) ;
#5732 = ORIENTED_EDGE ( 'NONE', *, *, #114540, .T. ) ;
#5733 = CARTESIAN_POINT ( 'NONE',  ( -0.4000000000000392131, 2.500000000000000000, -4.330127018922201643 ) ) ;
#5734 = CARTESIAN_POINT ( 'NONE',  ( 9.349999999999919709, 2.500000000000000000, 2.511473670974873507 ) ) ;
#5735 = DIRECTION ( 'NONE',  ( 0.000000000000000000, 0.000000000000000000, 1.000000000000000000 ) ) ;
#5736 = CARTESIAN_POINT ( 'NONE',  ( 10.84999999999990905, 2.500000000000000000, 2.857883832488649301 ) ) ;
#5737 = EDGE_LOOP ( 'NONE', ( #17065, #14170 ) ) ;
#5738 = PLANE ( 'NONE',  #73227 ) ;
#5739 = ORIENTED_EDGE ( 'NONE', *, *, #70059, .F. ) ;
#5740 = CARTESIAN_POINT ( 'NONE',  ( 32.28071041562795074, -1.401423001994599904, -4.680142630336261433 ) ) ;
#5741 = LINE ( 'NONE', #45702, #72727 ) ;
#5742 = FACE_OUTER_BOUND ( 'NONE', #14037, .T. ) ;
#5743 = CARTESIAN_POINT ( 'NONE',  ( 19.21290572970625732, -2.587129408759245575, 2.394140119532681688 ) ) ;
#5744 = ORIENTED_EDGE ( 'NONE', *, *, #61570, .F. ) ;
#5745 = AXIS2_PLACEMENT_3D ( 'NONE', #82970, #122891, #33237 ) ;
#5746 = CONICAL_SURFACE ( 'NONE', #22523, 0.1000000000000002554, 0.003490658503988666988 ) ;
#5747 = ORIENTED_EDGE ( 'NONE', *, *, #120955, .F. ) ;
#5748 = EDGE_LOOP ( 'NONE', ( #32933, #12528, #42354, #100528 ) ) ;
#5749 = CARTESIAN_POINT ( 'NONE',  ( -4.600000000000028066, 2.500000000000000000, -3.637306695894650055 ) ) ;
#5750 = DIRECTION ( 'NONE',  ( -0.000000000000000000, -1.000000000000000000, -0.000000000000000000 ) ) ;
#5751 = CARTESIAN_POINT ( 'NONE',  ( 3.349999999999941913, 2.500000000000000000, 6.395190528383296602 ) ) ;
#5752 = FACE_BOUND ( 'NONE', #118185, .T. ) ;
#5753 = DIRECTION ( 'NONE',  ( 0.000000000000000000, 1.000000000000000000, 0.000000000000000000 ) ) ;
#5754 = DIRECTION ( 'NONE',  ( 0.000000000000000000, 0.000000000000000000, 1.000000000000000000 ) ) ;
#5755 = AXIS2_PLACEMENT_3D ( 'NONE', #13640, #72584, #24770 ) ;
#5756 = CARTESIAN_POINT ( 'NONE',  ( -0.6000000000000388356, 2.500000000000000000, 3.983716857408420964 ) ) ;
#5757 = DIRECTION ( 'NONE',  ( 0.000000000000000000, 1.000000000000000000, 0.000000000000000000 ) ) ;
#5758 = CIRCLE ( 'NONE', #118641, 0.06509327318403745899 ) ;
#5759 = CIRCLE ( 'NONE', #78962, 0.1000000000000002554 ) ;
#5760 = CARTESIAN_POINT ( 'NONE',  ( 187.2552083336747444, 6.551208109652275624, -3.782341765624998686 ) ) ;
#5761 = DIRECTION ( 'NONE',  ( 0.000000000000000000, 0.000000000000000000, 1.000000000000000000 ) ) ;
#5762 = DIRECTION ( 'NONE',  ( 0.000000000000000000, 1.000000000000000000, 0.000000000000000000 ) ) ;
#5764 = EDGE_CURVE ( 'NONE', #69733, #97064, #89562, .T. ) ;
#5763 = AXIS2_PLACEMENT_3D ( 'NONE', #100162, #69395, #71324 ) ;
#5765 = DIRECTION ( 'NONE',  ( 0.000000000000000000, 0.000000000000000000, 1.000000000000000000 ) ) ;
#5766 = EDGE_LOOP ( 'NONE', ( #41133, #58657 ) ) ;
#5767 = ORIENTED_EDGE ( 'NONE', *, *, #78247, .T. ) ;
#5768 = EDGE_LOOP ( 'NONE', ( #44009, #63234, #75388, #42269 ) ) ;
#5769 = VERTEX_POINT ( 'NONE', #92243 ) ;
#5770 = CIRCLE ( 'NONE', #18411, 0.06509327318403745899 ) ;
#5771 = EDGE_CURVE ( 'NONE', #109919, #15887, #54057, .T. ) ;
#5772 = CARTESIAN_POINT ( 'NONE',  ( 108.0000000000000142, 5.000000000000000000, 0.000000000000000000 ) ) ;
#5773 = FACE_BOUND ( 'NONE', #29795, .T. ) ;
#5774 = EDGE_CURVE ( 'NONE', #41136, #3741, #13022, .T. ) ;
#5775 = DIRECTION ( 'NONE',  ( 0.000000000000000000, 0.000000000000000000, 1.000000000000000000 ) ) ;
#5776 = CIRCLE ( 'NONE', #78980, 0.09999999999999999167 ) ;
#5777 = AXIS2_PLACEMENT_3D ( 'NONE', #57674, #7254, #47210 ) ;
#5778 = EDGE_CURVE ( 'NONE', #94129, #52069, #47804, .T. ) ;
#5779 = ADVANCED_FACE ( 'NONE', ( #43176 ), #104011, .T. ) ;
#5780 = EDGE_LOOP ( 'NONE', ( #117184, #39969 ) ) ;
#5781 = CARTESIAN_POINT ( 'NONE',  ( 2.899999999999946620, 2.500000000000000000, -0.5928203230275542746 ) ) ;
#5782 = EDGE_CURVE ( 'NONE', #49583, #13385, #118805, .T. ) ;
#5783 = DIRECTION ( 'NONE',  ( 0.000000000000000000, 0.000000000000000000, 1.000000000000000000 ) ) ;
#5784 = EDGE_CURVE ( 'NONE', #120910, #102673, #5908, .T. ) ;
#5785 = AXIS2_PLACEMENT_3D ( 'NONE', #58177, #52207, #124000 ) ;
#5786 = VERTEX_POINT ( 'NONE', #3238 ) ;
#5787 = CARTESIAN_POINT ( 'NONE',  ( 12.89999999999990088, 12.50000000000000000, -4.330127018922201643 ) ) ;
#5788 = CIRCLE ( 'NONE', #49746, 0.1000000000000000472 ) ;
#5789 = LINE ( 'NONE', #126229, #38765 ) ;
#5790 = AXIS2_PLACEMENT_3D ( 'NONE', #4768, #54522, #125211 ) ;
#5791 = EDGE_LOOP ( 'NONE', ( #54468, #103310, #17198, #105823 ) ) ;
#5792 = DIRECTION ( 'NONE',  ( 0.000000000000000000, 1.000000000000000000, 0.000000000000000000 ) ) ;
#5794 = EDGE_CURVE ( 'NONE', #100348, #66863, #94183, .T. ) ;
#5793 = CARTESIAN_POINT ( 'NONE',  ( 8.349999999999923261, 2.500000000000000000, 2.757883832488649656 ) ) ;
#5795 = CONICAL_SURFACE ( 'NONE', #74784, 0.1000000000000002554, 0.003490658503988666988 ) ;
#5796 = AXIS2_PLACEMENT_3D ( 'NONE', #21268, #2263, #73583 ) ;
#5797 = EDGE_LOOP ( 'NONE', ( #22080, #113484 ) ) ;
#5798 = AXIS2_PLACEMENT_3D ( 'NONE', #12037, #51985, #112184 ) ;
#5799 = DIRECTION ( 'NONE',  ( 0.000000000000000000, 1.000000000000000000, 0.000000000000000000 ) ) ;
#5800 = DIRECTION ( 'NONE',  ( 0.000000000000000000, 1.000000000000000000, 0.000000000000000000 ) ) ;
#5801 = ORIENTED_EDGE ( 'NONE', *, *, #27504, .F. ) ;
#5802 = DIRECTION ( 'NONE',  ( 0.000000000000000000, 0.000000000000000000, -1.000000000000000000 ) ) ;
#5803 = ORIENTED_EDGE ( 'NONE', *, *, #91534, .T. ) ;
#5804 = ORIENTED_EDGE ( 'NONE', *, *, #24263, .F. ) ;
#5805 = VECTOR ( 'NONE', #8255, 1000.000000000000000 ) ;
#5806 = CARTESIAN_POINT ( 'NONE',  ( 12.09999999999990550, 12.50000000000000000, 3.637306695894644726 ) ) ;
#5807 = ORIENTED_EDGE ( 'NONE', *, *, #27594, .F. ) ;
#5808 = DIRECTION ( 'NONE',  ( -0.000000000000000000, -1.000000000000000000, -0.000000000000000000 ) ) ;
#5809 = FACE_OUTER_BOUND ( 'NONE', #9872, .T. ) ;
#5811 = CONICAL_SURFACE ( 'NONE', #60149, 0.09999999999999982514, 0.003490658503988666988 ) ;
#5810 = CIRCLE ( 'NONE', #110294, 0.06509327318403745899 ) ;
#5812 = VERTEX_POINT ( 'NONE', #83730 ) ;
#5813 = CARTESIAN_POINT ( 'NONE',  ( 10.39999999999991154, 12.50000000000000000, -4.957854068765716882 ) ) ;
#5814 = FACE_OUTER_BOUND ( 'NONE', #20646, .T. ) ;
#5815 = DIRECTION ( 'NONE',  ( -0.000000000000000000, -1.000000000000000000, -0.000000000000000000 ) ) ;
#5816 =( BOUNDED_CURVE ( )  B_SPLINE_CURVE ( 2, ( #29457, #100130, #79209, #128311, #69359, #11079, #128967 ),
 .UNSPECIFIED., .F., .F. ) 
 B_SPLINE_CURVE_WITH_KNOTS ( ( 3, 2, 2, 3 ),
 ( 0.2142857142857144681, 0.2380952380952383041, 0.2619047619047621955, 0.2857142857142859760 ),
 .UNSPECIFIED. ) 
 CURVE ( )  GEOMETRIC_REPRESENTATION_ITEM ( )  RATIONAL_B_SPLINE_CURVE ( ( 0.9999999999999988898, 0.8660254037844397068, 1.000000000000000000, 0.8660254037844387076, 1.000000000000000000, 0.8660254037844371533, 1.000000000000001554 ) ) 
 REPRESENTATION_ITEM ( '' )  );
#5817 = DIRECTION ( 'NONE',  ( 0.000000000000000000, 0.000000000000000000, 1.000000000000000000 ) ) ;
#5818 = EDGE_CURVE ( 'NONE', #7920, #25044, #123009, .T. ) ;
#5819 = CARTESIAN_POINT ( 'NONE',  ( 5.449999999999936229, 2.500000000000000000, 6.495190528383297135 ) ) ;
#5820 = DIRECTION ( 'NONE',  ( 0.000000000000000000, 1.000000000000000000, 0.000000000000000000 ) ) ;
#5821 = ORIENTED_EDGE ( 'NONE', *, *, #113188, .F. ) ;
#5822 = ORIENTED_EDGE ( 'NONE', *, *, #115525, .T. ) ;
#5823 = CARTESIAN_POINT ( 'NONE',  ( -9.150000000000009237, 2.500000000000000000, -1.472243186433550122 ) ) ;
#5824 = DIRECTION ( 'NONE',  ( 0.000000000000000000, 0.000000000000000000, -1.000000000000000000 ) ) ;
#5825 = DIRECTION ( 'NONE',  ( 0.000000000000000000, -0.9999939076577903929, 0.003490651415223739937 ) ) ;
#5827 = EDGE_LOOP ( 'NONE', ( #9886, #30996 ) ) ;
#5826 = ORIENTED_EDGE ( 'NONE', *, *, #104827, .F. ) ;
#5828 = ORIENTED_EDGE ( 'NONE', *, *, #26699, .T. ) ;
#5829 = EDGE_CURVE ( 'NONE', #37944, #92178, #85002, .T. ) ;
#5830 = DIRECTION ( 'NONE',  ( -0.000000000000000000, 1.000000000000000000, -0.000000000000000000 ) ) ;
#5831 = EDGE_CURVE ( 'NONE', #72089, #54959, #121044, .T. ) ;
#5832 = CARTESIAN_POINT ( 'NONE',  ( -6.650000000000014566, 2.500000000000000000, 6.495190528383297135 ) ) ;
#5833 = DIRECTION ( 'NONE',  ( -0.000000000000000000, 1.000000000000000000, -0.000000000000000000 ) ) ;
#5834 = EDGE_CURVE ( 'NONE', #114185, #2568, #62803, .T. ) ;
#5835 = DIRECTION ( 'NONE',  ( 0.000000000000000000, 0.000000000000000000, 1.000000000000000000 ) ) ;
#5836 = DIRECTION ( 'NONE',  ( -0.000000000000000000, 1.000000000000000000, -0.000000000000000000 ) ) ;
#5837 = DIRECTION ( 'NONE',  ( -4.274815082592931898E-19, -0.9999939076577903929, -0.003490651415223739937 ) ) ;
#5838 = DIRECTION ( 'NONE',  ( -0.000000000000000000, -1.000000000000000000, -0.000000000000000000 ) ) ;
#5839 = DIRECTION ( 'NONE',  ( -0.000000000000000000, -1.000000000000000000, -0.000000000000000000 ) ) ;
#5840 = DIRECTION ( 'NONE',  ( 0.000000000000000000, 0.000000000000000000, 1.000000000000000000 ) ) ;
#5841 = EDGE_CURVE ( 'NONE', #51535, #126108, #35290, .T. ) ;
#5842 = DIRECTION ( 'NONE',  ( 0.000000000000000000, 1.000000000000000000, 0.000000000000000000 ) ) ;
#5843 = EDGE_CURVE ( 'NONE', #40852, #3310, #123630, .T. ) ;
#5845 = EDGE_LOOP ( 'NONE', ( #90256, #16620 ) ) ;
#5844 = EDGE_CURVE ( 'NONE', #71057, #115877, #6017, .T. ) ;
#5846 = CONICAL_SURFACE ( 'NONE', #28861, 0.1000000000000002554, 0.003490658503988666988 ) ;
#5847 = ADVANCED_FACE ( 'NONE', ( #24806 ), #64719, .T. ) ;
#5848 = FACE_OUTER_BOUND ( 'NONE', #60487, .T. ) ;
#5849 = ORIENTED_EDGE ( 'NONE', *, *, #2862, .T. ) ;
#5850 = EDGE_LOOP ( 'NONE', ( #24162, #77212 ) ) ;
#5851 = CARTESIAN_POINT ( 'NONE',  ( 0.3999999999999628852, 12.50000000000000000, -0.6928203230275520319 ) ) ;
#5852 = FACE_OUTER_BOUND ( 'NONE', #14068, .T. ) ;
#5853 = CARTESIAN_POINT ( 'NONE',  ( -10.40000000000000213, 2.500000000000000000, -5.022947341949749678 ) ) ;
#5854 = ADVANCED_FACE ( 'NONE', ( #5150 ), #45101, .T. ) ;
#5855 = CIRCLE ( 'NONE', #72689, 0.06509327318403745899 ) ;
#5856 = CARTESIAN_POINT ( 'NONE',  ( -0.6000000000000383915, 12.50000000000000000, -3.983716857408426293 ) ) ;
#5857 = CIRCLE ( 'NONE', #41505, 0.1000000000000000472 ) ;
#5858 = DIRECTION ( 'NONE',  ( -4.274815082592931898E-19, -0.9999939076577903929, -0.003490651415223739937 ) ) ;
#5859 = DIRECTION ( 'NONE',  ( 0.000000000000000000, 0.000000000000000000, -1.000000000000000000 ) ) ;
#5860 = LINE ( 'NONE', #37287, #90646 ) ;
#5861 = ORIENTED_EDGE ( 'NONE', *, *, #86570, .F. ) ;
#5862 = DIRECTION ( 'NONE',  ( -4.274815082592931898E-19, -0.9999939076577903929, -0.003490651415223739937 ) ) ;
#5863 = LINE ( 'NONE', #53695, #83327 ) ;
#5864 = EDGE_LOOP ( 'NONE', ( #42066, #121420 ) ) ;
#5865 = CONICAL_SURFACE ( 'NONE', #1754, 0.1000000000000000056, 0.003490658503988666988 ) ;
#5866 = ORIENTED_EDGE ( 'NONE', *, *, #110867, .T. ) ;
#5867 = VERTEX_POINT ( 'NONE', #85653 ) ;
#5868 = CIRCLE ( 'NONE', #8021, 0.1000000000000002554 ) ;
#5869 = EDGE_LOOP ( 'NONE', ( #125294, #13998, #10454, #106543 ) ) ;
#5870 = CARTESIAN_POINT ( 'NONE',  ( -3.550000000000030909, 12.50000000000000000, -6.841600689897078702 ) ) ;
#5871 = DIRECTION ( 'NONE',  ( -0.000000000000000000, 1.000000000000000000, -0.000000000000000000 ) ) ;
#5872 = CONICAL_SURFACE ( 'NONE', #102138, 0.09999999999999982514, 0.003490658503988666988 ) ;
#5873 = CARTESIAN_POINT ( 'NONE',  ( 9.599999999999914380, 2.500000000000000000, -3.637306695894650055 ) ) ;
#5874 = LINE ( 'NONE', #5242, #2686 ) ;
#5875 = CARTESIAN_POINT ( 'NONE',  ( 9.999999999999911182, 12.50000000000000000, 5.088040615133786027 ) ) ;
#5876 = EDGE_LOOP ( 'NONE', ( #10322, #116225 ) ) ;
#5877 = DIRECTION ( 'NONE',  ( -4.274815082592931898E-19, -0.9999939076577903929, -0.003490651415223739937 ) ) ;
#5878 = CIRCLE ( 'NONE', #22647, 0.1000000000000002554 ) ;
#5879 = CONICAL_SURFACE ( 'NONE', #79079, 0.09999999999999982514, 0.003490658503988666988 ) ;
#5880 = LINE ( 'NONE', #85741, #22786 ) ;
#5881 = ORIENTED_EDGE ( 'NONE', *, *, #88282, .T. ) ;
#5882 = AXIS2_PLACEMENT_3D ( 'NONE', #92358, #2680, #19773 ) ;
#5883 = EDGE_CURVE ( 'NONE', #66538, #119116, #3967, .T. ) ;
#5884 = VERTEX_POINT ( 'NONE', #117021 ) ;
#5885 = ORIENTED_EDGE ( 'NONE', *, *, #91262, .T. ) ;
#5886 = DIRECTION ( 'NONE',  ( -0.000000000000000000, -1.000000000000000000, -0.000000000000000000 ) ) ;
#5887 = DIRECTION ( 'NONE',  ( 0.000000000000000000, 0.000000000000000000, 1.000000000000000000 ) ) ;
#5888 = DIRECTION ( 'NONE',  ( 0.000000000000000000, 1.000000000000000000, 0.000000000000000000 ) ) ;
#5889 = EDGE_LOOP ( 'NONE', ( #37233, #106184, #50325, #128711 ) ) ;
#5890 = CARTESIAN_POINT ( 'NONE',  ( 4.999999999999936939, 2.500000000000000000, -3.637306695894650055 ) ) ;
#5891 = DIRECTION ( 'NONE',  ( 0.000000000000000000, 0.000000000000000000, -1.000000000000000000 ) ) ;
#5892 = EDGE_CURVE ( 'NONE', #87369, #41701, #31189, .T. ) ;
#5893 = DIRECTION ( 'NONE',  ( 0.000000000000000000, -0.9999939076577903929, 0.003490651415223739937 ) ) ;
#5894 = DIRECTION ( 'NONE',  ( -0.000000000000000000, 1.000000000000000000, -0.000000000000000000 ) ) ;
#5895 = DIRECTION ( 'NONE',  ( 0.000000000000000000, 0.000000000000000000, 1.000000000000000000 ) ) ;
#5896 = EDGE_LOOP ( 'NONE', ( #122123, #125014 ) ) ;
#5898 = CONICAL_SURFACE ( 'NONE', #43508, 0.1000000000000002554, 0.003490658503988666988 ) ;
#5897 = CIRCLE ( 'NONE', #118788, 0.1000000000000002554 ) ;
#5899 = DIRECTION ( 'NONE',  ( 0.000000000000000000, 0.000000000000000000, 1.000000000000000000 ) ) ;
#5900 = ORIENTED_EDGE ( 'NONE', *, *, #22942, .T. ) ;
#5901 = ORIENTED_EDGE ( 'NONE', *, *, #56326, .T. ) ;
#5902 = ORIENTED_EDGE ( 'NONE', *, *, #72453, .T. ) ;
#5903 = DIRECTION ( 'NONE',  ( 0.000000000000000000, 1.000000000000000000, 0.000000000000000000 ) ) ;
#5904 = FACE_BOUND ( 'NONE', #67365, .T. ) ;
#5905 = CARTESIAN_POINT ( 'NONE',  ( 186.1145833340161175, 6.668395609140177704, -3.849999999999998312 ) ) ;
#5906 = DIRECTION ( 'NONE',  ( -0.000000000000000000, -1.000000000000000000, -0.000000000000000000 ) ) ;
#5907 = DIRECTION ( 'NONE',  ( -0.000000000000000000, -1.000000000000000000, -0.000000000000000000 ) ) ;
#5908 = CIRCLE ( 'NONE', #49875, 0.1000000000000000056 ) ;
#5909 = ORIENTED_EDGE ( 'NONE', *, *, #69506, .F. ) ;
#5910 = DIRECTION ( 'NONE',  ( 0.000000000000000000, 0.000000000000000000, 1.000000000000000000 ) ) ;
#5911 = LINE ( 'NONE', #115887, #26015 ) ;
#5912 = FACE_OUTER_BOUND ( 'NONE', #73383, .T. ) ;
#5913 = DIRECTION ( 'NONE',  ( 0.000000000000000000, 1.000000000000000000, 0.000000000000000000 ) ) ;
#5914 = ORIENTED_EDGE ( 'NONE', *, *, #51214, .F. ) ;
#5915 = DIRECTION ( 'NONE',  ( 0.000000000000000000, 0.000000000000000000, -1.000000000000000000 ) ) ;
#5916 = AXIS2_PLACEMENT_3D ( 'NONE', #117936, #58400, #18455 ) ;
#5917 = ADVANCED_FACE ( 'NONE', ( #67260 ), #66651, .T. ) ;
#5918 = AXIS2_PLACEMENT_3D ( 'NONE', #60628, #30529, #21318 ) ;
#5919 = DIRECTION ( 'NONE',  ( 0.000000000000000000, 0.000000000000000000, 1.000000000000000000 ) ) ;
#5920 = CIRCLE ( 'NONE', #37548, 0.06509327318403745899 ) ;
#5921 = ORIENTED_EDGE ( 'NONE', *, *, #120359, .T. ) ;
#5922 = CARTESIAN_POINT ( 'NONE',  ( 5.199999999999933564, 12.50000000000000000, 0.3464101615137735735 ) ) ;
#5923 = FACE_BOUND ( 'NONE', #119940, .T. ) ;
#5924 = EDGE_CURVE ( 'NONE', #50242, #59628, #116391, .T. ) ;
#5925 = DIRECTION ( 'NONE',  ( 0.000000000000000000, 0.000000000000000000, 1.000000000000000000 ) ) ;
#5926 = AXIS2_PLACEMENT_3D ( 'NONE', #58007, #98537, #128705 ) ;
#5927 = CONICAL_SURFACE ( 'NONE', #47733, 0.1000000000000002554, 0.003490658503988666988 ) ;
#5928 = VECTOR ( 'NONE', #83825, 1000.000000000000000 ) ;
#5929 = ORIENTED_EDGE ( 'NONE', *, *, #87428, .F. ) ;
#5930 = DIRECTION ( 'NONE',  ( -0.000000000000000000, -1.000000000000000000, -0.000000000000000000 ) ) ;
#5931 = FACE_OUTER_BOUND ( 'NONE', #19012, .T. ) ;
#5932 = EDGE_CURVE ( 'NONE', #27373, #69211, #74985, .T. ) ;
#5933 = ORIENTED_EDGE ( 'NONE', *, *, #44218, .F. ) ;
#5934 = EDGE_CURVE ( 'NONE', #121533, #10045, #37443, .T. ) ;
#5935 = ORIENTED_EDGE ( 'NONE', *, *, #106790, .T. ) ;
#5936 = ADVANCED_FACE ( 'NONE', ( #128168 ), #64609, .T. ) ;
#5937 = EDGE_CURVE ( 'NONE', #74378, #124598, #47905, .T. ) ;
#5938 = CARTESIAN_POINT ( 'NONE',  ( 186.1718750003414016, 9.264065473108010111E-16, -7.564683531250000925 ) ) ;
#5939 = ADVANCED_FACE ( 'NONE', ( #126878 ), #110580, .T. ) ;
#5940 = VECTOR ( 'NONE', #83697, 1000.000000000000000 ) ;
#5941 = ORIENTED_EDGE ( 'NONE', *, *, #55971, .F. ) ;
#5942 = CARTESIAN_POINT ( 'NONE',  ( 186.0885416670080872, -6.551208109652273848, -3.782341765625003571 ) ) ;
#5943 = FACE_OUTER_BOUND ( 'NONE', #39851, .T. ) ;
#5944 = DIRECTION ( 'NONE',  ( 0.000000000000000000, 0.000000000000000000, 1.000000000000000000 ) ) ;
#5945 = CARTESIAN_POINT ( 'NONE',  ( 2.299999999999948752, 2.500000000000000000, 0.3464101615137735735 ) ) ;
#5946 = CARTESIAN_POINT ( 'NONE',  ( -0.4000000000000401013, 12.50000000000000000, -3.572213422710612374 ) ) ;
#5947 = EDGE_CURVE ( 'NONE', #3753, #72399, #39513, .T. ) ;
#5948 = EDGE_CURVE ( 'NONE', #44658, #72823, #37839, .T. ) ;
#5949 = AXIS2_PLACEMENT_3D ( 'NONE', #79088, #29346, #109826 ) ;
#5950 = EDGE_CURVE ( 'NONE', #120001, #39091, #20709, .T. ) ;
#5951 = EDGE_LOOP ( 'NONE', ( #116376, #78578 ) ) ;
#5952 = EDGE_LOOP ( 'NONE', ( #78835, #1359 ) ) ;
#5953 = CARTESIAN_POINT ( 'NONE',  ( -4.200000000000025935, 12.50000000000000000, 0.06509327318403504425 ) ) ;
#5954 = FACE_OUTER_BOUND ( 'NONE', #120034, .T. ) ;
#5955 = CIRCLE ( 'NONE', #16406, 0.1000000000000002554 ) ;
#5956 = DIRECTION ( 'NONE',  ( -0.000000000000000000, 1.000000000000000000, -0.000000000000000000 ) ) ;
#5957 = CONICAL_SURFACE ( 'NONE', #110434, 0.1000000000000002554, 0.003490658503988666988 ) ;
#5958 = DIRECTION ( 'NONE',  ( -0.000000000000000000, -1.000000000000000000, -0.000000000000000000 ) ) ;
#5960 = ORIENTED_EDGE ( 'NONE', *, *, #95414, .T. ) ;
#5959 = EDGE_LOOP ( 'NONE', ( #80506, #11905 ) ) ;
#5961 = DIRECTION ( 'NONE',  ( 0.000000000000000000, -0.000000000000000000, -1.000000000000000000 ) ) ;
#5962 = ORIENTED_EDGE ( 'NONE', *, *, #39520, .T. ) ;
#5963 = DIRECTION ( 'NONE',  ( -0.000000000000000000, -1.000000000000000000, -0.000000000000000000 ) ) ;
#5964 = DIRECTION ( 'NONE',  ( -0.000000000000000000, -1.000000000000000000, -0.000000000000000000 ) ) ;
#5965 = ORIENTED_EDGE ( 'NONE', *, *, #79151, .T. ) ;
#5966 = DIRECTION ( 'NONE',  ( 0.000000000000000000, -0.000000000000000000, 1.000000000000000000 ) ) ;
#5967 = AXIS2_PLACEMENT_3D ( 'NONE', #113759, #24086, #64005 ) ;
#5968 = DIRECTION ( 'NONE',  ( 0.000000000000000000, -0.9999939076577903929, 0.003490651415223739937 ) ) ;
#5969 = CARTESIAN_POINT ( 'NONE',  ( 6.449999999999933564, 2.500000000000000000, -6.941600689897078347 ) ) ;
#5970 = DIRECTION ( 'NONE',  ( 0.000000000000000000, 1.000000000000000000, 0.000000000000000000 ) ) ;
#5971 =( GEOMETRIC_REPRESENTATION_CONTEXT ( 3 ) GLOBAL_UNCERTAINTY_ASSIGNED_CONTEXT ( ( #2384 ) ) GLOBAL_UNIT_ASSIGNED_CONTEXT ( ( #1978, #22299, #60295 ) ) REPRESENTATION_CONTEXT ( 'NONE', 'WORKASPACE' ) );
#5972 = DIRECTION ( 'NONE',  ( 0.000000000000000000, -0.9999939076577903929, 0.003490651415223739937 ) ) ;
#5973 = CARTESIAN_POINT ( 'NONE',  ( -9.800000000000004263, 2.500000000000000000, 3.983716857408420076 ) ) ;
#5974 = CARTESIAN_POINT ( 'NONE',  ( 187.0677083336747160, -4.367472073101514418, -7.564683531250002702 ) ) ;
#5975 = FACE_OUTER_BOUND ( 'NONE', #11208, .T. ) ;
#5976 = VECTOR ( 'NONE', #32457, 1000.000000000000000 ) ;
#5977 = CARTESIAN_POINT ( 'NONE',  ( -1.250000000000037526, 2.500000000000000000, -5.802370205355749988 ) ) ;
#5978 = VERTEX_POINT ( 'NONE', #96113 ) ;
#5979 = ORIENTED_EDGE ( 'NONE', *, *, #93620, .T. ) ;
#5980 = CARTESIAN_POINT ( 'NONE',  ( 9.999999999999911182, 12.50000000000000000, 4.957854068765711553 ) ) ;
#5981 = ORIENTED_EDGE ( 'NONE', *, *, #9236, .F. ) ;
#5982 = DIRECTION ( 'NONE',  ( 0.000000000000000000, 1.000000000000000000, 0.000000000000000000 ) ) ;
#5983 = ADVANCED_FACE ( 'NONE', ( #6413 ), #12276, .T. ) ;
#5985 = VERTEX_POINT ( 'NONE', #86279 ) ;
#5984 = ORIENTED_EDGE ( 'NONE', *, *, #100999, .F. ) ;
#5986 = ORIENTED_EDGE ( 'NONE', *, *, #41795, .T. ) ;
#5987 = AXIS2_PLACEMENT_3D ( 'NONE', #9363, #19837, #49313 ) ;
#5988 = DIRECTION ( 'NONE',  ( 0.000000000000000000, 0.000000000000000000, 1.000000000000000000 ) ) ;
#5989 = CARTESIAN_POINT ( 'NONE',  ( -6.650000000000014566, 2.500000000000000000, 5.802370205355744659 ) ) ;
#5990 = SURFACE_SIDE_STYLE ('',( #85210 ) ) ;
#5991 = AXIS2_PLACEMENT_3D ( 'NONE', #35402, #36044, #102825 ) ;
#5992 = CARTESIAN_POINT ( 'NONE',  ( 7.899999999999924860, 12.50000000000000000, -5.022947341949754119 ) ) ;
#5993 = DIRECTION ( 'NONE',  ( 0.000000000000000000, 1.000000000000000000, 0.000000000000000000 ) ) ;
#5994 = DIRECTION ( 'NONE',  ( 0.000000000000000000, 1.000000000000000000, 0.000000000000000000 ) ) ;
#5995 = CIRCLE ( 'NONE', #118885, 0.09999999999999982514 ) ;
#5996 = ORIENTED_EDGE ( 'NONE', *, *, #12308, .F. ) ;
#5997 = ADVANCED_FACE ( 'NONE', ( #126226, #56814, #26736 ), #106576, .F. ) ;
#5998 = DIRECTION ( 'NONE',  ( -4.274815082592931898E-19, -0.9999939076577903929, -0.003490651415223739937 ) ) ;
#5999 = ORIENTED_EDGE ( 'NONE', *, *, #913, .T. ) ;
#6000 = ADVANCED_FACE ( 'NONE', ( #7072 ), #114775, .T. ) ;
#6002 = AXIS2_PLACEMENT_3D ( 'NONE', #73853, #24116, #64038 ) ;
#6001 = AXIS2_PLACEMENT_3D ( 'NONE', #44783, #43497, #34327 ) ;
#6003 = ORIENTED_EDGE ( 'NONE', *, *, #61264, .T. ) ;
#6004 = ORIENTED_EDGE ( 'NONE', *, *, #97858, .T. ) ;
#6005 = ORIENTED_EDGE ( 'NONE', *, *, #97270, .F. ) ;
#6006 = ADVANCED_FACE ( 'NONE', ( #58142 ), #26970, .T. ) ;
#6007 = CARTESIAN_POINT ( 'NONE',  ( 130.5000000000000000, -0.5000000000000000000, 7.499999999999998224 ) ) ;
#6008 = ORIENTED_EDGE ( 'NONE', *, *, #72780, .T. ) ;
#6009 = ORIENTED_EDGE ( 'NONE', *, *, #54720, .F. ) ;
#6010 = PLANE ( 'NONE',  #115515 ) ;
#6011 = EDGE_CURVE ( 'NONE', #100878, #84422, #127316, .T. ) ;
#6012 = FACE_OUTER_BOUND ( 'NONE', #70877, .T. ) ;
#6013 = DIRECTION ( 'NONE',  ( 0.000000000000000000, 0.000000000000000000, -1.000000000000000000 ) ) ;
#6014 = DIRECTION ( 'NONE',  ( 0.000000000000000000, 1.000000000000000000, 0.000000000000000000 ) ) ;
#6015 = DIRECTION ( 'NONE',  ( -0.000000000000000000, -1.000000000000000000, -0.000000000000000000 ) ) ;
#6017 = CIRCLE ( 'NONE', #125168, 0.06509327318403745899 ) ;
#6016 = CARTESIAN_POINT ( 'NONE',  ( 3.549999999999944755, 12.50000000000000000, -2.511473670974877948 ) ) ;
#6018 = ORIENTED_EDGE ( 'NONE', *, *, #95348, .F. ) ;
#6019 = DIRECTION ( 'NONE',  ( 0.000000000000000000, 1.000000000000000000, 0.000000000000000000 ) ) ;
#6020 = ORIENTED_EDGE ( 'NONE', *, *, #94886, .F. ) ;
#6022 = DIRECTION ( 'NONE',  ( 0.000000000000000000, 1.000000000000000000, 0.000000000000000000 ) ) ;
#6021 = CIRCLE ( 'NONE', #39519, 0.1000000000000000472 ) ;
#6024 = EDGE_LOOP ( 'NONE', ( #21122, #73375 ) ) ;
#6023 = AXIS2_PLACEMENT_3D ( 'NONE', #88627, #38920, #50635 ) ;
#6025 = CARTESIAN_POINT ( 'NONE',  ( 14.59999999999989484, 12.50000000000000000, -2.276824562219559311E-15 ) ) ;
#6026 = AXIS2_PLACEMENT_3D ( 'NONE', #62055, #31948, #71212 ) ;
#6027 = ORIENTED_EDGE ( 'NONE', *, *, #36244, .F. ) ;
#6028 = EDGE_CURVE ( 'NONE', #39107, #18925, #118983, .T. ) ;
#6029 = VERTEX_POINT ( 'NONE', #21927 ) ;
#6031 = AXIS2_PLACEMENT_3D ( 'NONE', #67700, #118093, #105043 ) ;
#6030 = CARTESIAN_POINT ( 'NONE',  ( 9.149999999999916866, 12.50000000000000000, 7.188010851410848723 ) ) ;
#6032 = DIRECTION ( 'NONE',  ( 0.000000000000000000, 1.000000000000000000, 0.000000000000000000 ) ) ;
#6033 = VECTOR ( 'NONE', #18893, 1000.000000000000000 ) ;
#6034 = DIRECTION ( 'NONE',  ( 0.000000000000000000, 0.000000000000000000, 1.000000000000000000 ) ) ;
#6035 = DIRECTION ( 'NONE',  ( 0.000000000000000000, 0.000000000000000000, 1.000000000000000000 ) ) ;
#6036 = LINE ( 'NONE', #84618, #67933 ) ;
#6037 = VERTEX_POINT ( 'NONE', #121397 ) ;
#6038 = DIRECTION ( 'NONE',  ( 0.000000000000000000, 0.000000000000000000, -1.000000000000000000 ) ) ;
#6039 = FACE_OUTER_BOUND ( 'NONE', #24073, .T. ) ;
#6040 = FACE_OUTER_BOUND ( 'NONE', #15763, .T. ) ;
#6041 = DIRECTION ( 'NONE',  ( 0.000000000000000000, 1.000000000000000000, 0.000000000000000000 ) ) ;
#6042 = DIRECTION ( 'NONE',  ( 0.000000000000000000, 0.000000000000000000, 1.000000000000000000 ) ) ;
#6043 = CIRCLE ( 'NONE', #22809, 0.09999999999999999167 ) ;
#6044 = EDGE_LOOP ( 'NONE', ( #38454, #21595 ) ) ;
#6045 = EDGE_CURVE ( 'NONE', #59553, #49236, #83407, .T. ) ;
#6046 = ORIENTED_EDGE ( 'NONE', *, *, #61421, .F. ) ;
#6047 = UNCERTAINTY_MEASURE_WITH_UNIT (LENGTH_MEASURE( 1.000000000000000082E-05 ), #11976, 'distance_accuracy_value', 'NONE');
#6048 = ORIENTED_EDGE ( 'NONE', *, *, #13327, .F. ) ;
#6049 = DIRECTION ( 'NONE',  ( 0.000000000000000000, 0.000000000000000000, -1.000000000000000000 ) ) ;
#6051 = AXIS2_PLACEMENT_3D ( 'NONE', #2424, #74902, #116105 ) ;
#6050 = DIRECTION ( 'NONE',  ( -0.000000000000000000, 1.000000000000000000, -0.000000000000000000 ) ) ;
#6052 = AXIS2_PLACEMENT_3D ( 'NONE', #61614, #41966, #81865 ) ;
#6053 = CARTESIAN_POINT ( 'NONE',  ( 186.2916666666666856, 4.445597072760120838, -7.699999999999998401 ) ) ;
#6054 = DIRECTION ( 'NONE',  ( -0.000000000000000000, -1.000000000000000000, -0.000000000000000000 ) ) ;
#6055 = DIRECTION ( 'NONE',  ( 0.000000000000000000, 0.000000000000000000, -1.000000000000000000 ) ) ;
#6056 = EDGE_CURVE ( 'NONE', #82618, #121714, #118902, .T. ) ;
#6057 = FILL_AREA_STYLE_COLOUR ( '', #69146 ) ;
#6058 = DIRECTION ( 'NONE',  ( -0.000000000000000000, -1.000000000000000000, -0.000000000000000000 ) ) ;
#6059 = ORIENTED_EDGE ( 'NONE', *, *, #115171, .F. ) ;
#6060 = CARTESIAN_POINT ( 'NONE',  ( -3.350000000000028511, 2.500000000000000000, -1.372243186433550033 ) ) ;
#6061 = DIRECTION ( 'NONE',  ( 0.000000000000000000, 0.000000000000000000, -1.000000000000000000 ) ) ;
#6062 = CIRCLE ( 'NONE', #123155, 0.09999999999999982514 ) ;
#6063 = EDGE_LOOP ( 'NONE', ( #4227, #7198, #72515, #3551 ) ) ;
#6064 = ADVANCED_FACE ( 'NONE', ( #31735 ), #51395, .T. ) ;
#6065 = DIRECTION ( 'NONE',  ( 0.000000000000000000, 0.000000000000000000, 1.000000000000000000 ) ) ;
#6066 = AXIS2_PLACEMENT_3D ( 'NONE', #84743, #24536, #14048 ) ;
#6067 = DIRECTION ( 'NONE',  ( 0.000000000000000000, 1.000000000000000000, 0.000000000000000000 ) ) ;
#6068 = CARTESIAN_POINT ( 'NONE',  ( -1.250000000000036193, 2.500000000000000000, 5.802370205355744659 ) ) ;
#6069 = VECTOR ( 'NONE', #55985, 1000.000000000000000 ) ;
#6070 = ORIENTED_EDGE ( 'NONE', *, *, #90083, .F. ) ;
#6071 = DIRECTION ( 'NONE',  ( 0.000000000000000000, 0.000000000000000000, 1.000000000000000000 ) ) ;
#6072 = VERTEX_POINT ( 'NONE', #71656 ) ;
#6074 = CONICAL_SURFACE ( 'NONE', #87558, 0.1000000000000002554, 0.003490658503988666988 ) ;
#6073 = CARTESIAN_POINT ( 'NONE',  ( 3.749999999999978684, 2.500000000000000000, -6.495190528383302464 ) ) ;
#6075 = DIRECTION ( 'NONE',  ( 0.000000000000000000, 0.000000000000000000, 1.000000000000000000 ) ) ;
#6076 = ORIENTED_EDGE ( 'NONE', *, *, #33309, .F. ) ;
#6077 = CARTESIAN_POINT ( 'NONE',  ( 4.399999999999940847, 2.500000000000000000, -3.983716857408426293 ) ) ;
#6078 = EDGE_CURVE ( 'NONE', #70723, #109689, #72930, .T. ) ;
#6079 = CIRCLE ( 'NONE', #93839, 0.06509327318403745899 ) ;
#6080 = DIRECTION ( 'NONE',  ( -0.000000000000000000, 1.000000000000000000, -0.000000000000000000 ) ) ;
#6081 = ORIENTED_EDGE ( 'NONE', *, *, #22010, .T. ) ;
#6082 = ORIENTED_EDGE ( 'NONE', *, *, #95191, .F. ) ;
#6083 = PLANE ( 'NONE',  #111985 ) ;
#6084 = EDGE_CURVE ( 'NONE', #128192, #90718, #58779, .T. ) ;
#6086 = AXIS2_PLACEMENT_3D ( 'NONE', #12182, #63237, #2351 ) ;
#6085 = AXIS2_PLACEMENT_3D ( 'NONE', #12940, #52891, #33890 ) ;
#6087 = ORIENTED_EDGE ( 'NONE', *, *, #61244, .T. ) ;
#6088 = FACE_OUTER_BOUND ( 'NONE', #72111, .T. ) ;
#6089 = CARTESIAN_POINT ( 'NONE',  ( -12.49999999999995737, 2.500000000000000000, 4.430127018922196847 ) ) ;
#6090 = EDGE_CURVE ( 'NONE', #124494, #42905, #89657, .T. ) ;
#6091 = ADVANCED_FACE ( 'NONE', ( #72949 ), #100124, .T. ) ;
#6092 = ORIENTED_EDGE ( 'NONE', *, *, #60713, .T. ) ;
#6093 = ADVANCED_FACE ( 'NONE', ( #29325 ), #85540, .T. ) ;
#6094 = ADVANCED_FACE ( 'NONE', ( #23191 ), #109146, .T. ) ;
#6095 = CARTESIAN_POINT ( 'NONE',  ( 7.949999999999925571, 2.500000000000000000, -6.495190528383302464 ) ) ;
#6096 = CARTESIAN_POINT ( 'NONE',  ( -13.94999999999998685, 12.50000000000000000, -2.511473670974875727 ) ) ;
#6097 = EDGE_LOOP ( 'NONE', ( #10210, #87511 ) ) ;
#6098 = CARTESIAN_POINT ( 'NONE',  ( -3.550000000000028244, 12.50000000000000000, 2.511473670974873507 ) ) ;
#6099 = CARTESIAN_POINT ( 'NONE',  ( 8.549999999999922551, 2.500000000000000000, -6.048780366869526581 ) ) ;
#6100 = ADVANCED_FACE ( 'NONE', ( #53319 ), #102413, .T. ) ;
#6101 = CARTESIAN_POINT ( 'NONE',  ( 16.56576425165007649, -1.499999999999997113, -6.084390597445788806 ) ) ;
#6102 = CIRCLE ( 'NONE', #73024, 0.1000000000000000056 ) ;
#6103 = FACE_OUTER_BOUND ( 'NONE', #52348, .T. ) ;
#6104 = ADVANCED_FACE ( 'NONE', ( #82121 ), #83422, .T. ) ;
#6105 = CARTESIAN_POINT ( 'NONE',  ( -8.350000000000013856, 2.500000000000000000, 2.165063509461097713 ) ) ;
#6106 = CARTESIAN_POINT ( 'NONE',  ( -7.900000000000011013, 2.500000000000000000, 5.122947341949749323 ) ) ;
#6107 = EDGE_CURVE ( 'NONE', #50779, #62968, #114869, .T. ) ;
#6108 = ADVANCED_FACE ( 'NONE', ( #33044 ), #41576, .T. ) ;
#6109 = VECTOR ( 'NONE', #94127, 1000.000000000000000 ) ;
#6110 = ADVANCED_FACE ( 'NONE', ( #18840 ), #47992, .T. ) ;
#6111 = AXIS2_PLACEMENT_3D ( 'NONE', #49053, #88959, #78514 ) ;
#6112 = ORIENTED_EDGE ( 'NONE', *, *, #39836, .F. ) ;
#6113 = EDGE_LOOP ( 'NONE', ( #71080, #14286 ) ) ;
#6114 = EDGE_LOOP ( 'NONE', ( #47227, #23549 ) ) ;
#6115 = ORIENTED_EDGE ( 'NONE', *, *, #108452, .F. ) ;
#6116 = CARTESIAN_POINT ( 'NONE',  ( 65.38811649227257305, 3.824344232458577242, 5.305600839591995133 ) ) ;
#6117 = DIRECTION ( 'NONE',  ( 0.000000000000000000, -0.9999939076577903929, 0.003490651415223739937 ) ) ;
#6118 = DIRECTION ( 'NONE',  ( 0.000000000000000000, 0.000000000000000000, 1.000000000000000000 ) ) ;
#6119 = ORIENTED_EDGE ( 'NONE', *, *, #56735, .F. ) ;
#6120 = FACE_BOUND ( 'NONE', #53041, .T. ) ;
#6121 = EDGE_CURVE ( 'NONE', #8342, #49328, #86625, .T. ) ;
#6122 = CARTESIAN_POINT ( 'NONE',  ( 10.64999999999991331, 2.500000000000000000, 6.148780366869520897 ) ) ;
#6123 = DIRECTION ( 'NONE',  ( 0.000000000000000000, 1.000000000000000000, 0.000000000000000000 ) ) ;
#6124 = CIRCLE ( 'NONE', #116933, 0.06509327318403745899 ) ;
#6125 = FACE_OUTER_BOUND ( 'NONE', #105982, .T. ) ;
#6126 = CIRCLE ( 'NONE', #79320, 0.06509327318403745899 ) ;
#6127 = CARTESIAN_POINT ( 'NONE',  ( -10.45000000000000107, 2.500000000000000000, 6.395190528383296602 ) ) ;
#6128 = LINE ( 'NONE', #46076, #99421 ) ;
#6129 = DIRECTION ( 'NONE',  ( 0.000000000000000000, 0.000000000000000000, 1.000000000000000000 ) ) ;
#6130 = CARTESIAN_POINT ( 'NONE',  ( -2.499999999999996003, 12.50000000000000000, -4.395220292106239768 ) ) ;
#6131 = FACE_OUTER_BOUND ( 'NONE', #32652, .T. ) ;
#6132 = CARTESIAN_POINT ( 'NONE',  ( -2.300000000000032685, 2.500000000000000000, -4.776537180435978414 ) ) ;
#6133 = AXIS2_PLACEMENT_3D ( 'NONE', #35582, #83393, #75482 ) ;
#6134 = DIRECTION ( 'NONE',  ( 0.000000000000000000, -0.9999939076577903929, 0.003490651415223739937 ) ) ;
#6135 = CIRCLE ( 'NONE', #96036, 0.06509327318403745899 ) ;
#6136 = ORIENTED_EDGE ( 'NONE', *, *, #127672, .F. ) ;
#6137 = EDGE_LOOP ( 'NONE', ( #25763, #44126, #111832, #122322 ) ) ;
#6138 = CONICAL_SURFACE ( 'NONE', #89773, 0.1000000000000000472, 0.003490658503988666988 ) ;
#6139 = ORIENTED_EDGE ( 'NONE', *, *, #40240, .F. ) ;
#6140 = EDGE_LOOP ( 'NONE', ( #21883, #123981, #5088, #4039 ) ) ;
#6141 = DIRECTION ( 'NONE',  ( -4.274815082592931898E-19, -0.9999939076577903929, -0.003490651415223739937 ) ) ;
#6142 = ORIENTED_EDGE ( 'NONE', *, *, #36245, .F. ) ;
#6143 = DIRECTION ( 'NONE',  ( 0.000000000000000000, 0.000000000000000000, -1.000000000000000000 ) ) ;
#6144 = ORIENTED_EDGE ( 'NONE', *, *, #24897, .T. ) ;
#6145 = VERTEX_POINT ( 'NONE', #93877 ) ;
#6146 = CARTESIAN_POINT ( 'NONE',  ( 7.699999999999923794, 12.50000000000000000, -0.4115034346978157509 ) ) ;
#6148 = CARTESIAN_POINT ( 'NONE',  ( 7.180215335588899350, -2.499999999999999556, 8.697219394723605390 ) ) ;
#6147 = PRODUCT_DEFINITION_CONTEXT ( 'detailed design', #84818, 'design' ) ;
#6149 = DIRECTION ( 'NONE',  ( 0.000000000000000000, 0.000000000000000000, -1.000000000000000000 ) ) ;
#6150 = LINE ( 'NONE', #27100, #3281 ) ;
#6151 = CARTESIAN_POINT ( 'NONE',  ( -4.999999999999990230, 12.50000000000000000, -4.265033745738164406 ) ) ;
#6152 = ORIENTED_EDGE ( 'NONE', *, *, #63330, .T. ) ;
#6153 = ORIENTED_EDGE ( 'NONE', *, *, #122112, .F. ) ;
#6154 = ADVANCED_FACE ( 'NONE', ( #53954 ), #64409, .T. ) ;
#6155 = VERTEX_POINT ( 'NONE', #44128 ) ;
#6156 = VERTEX_POINT ( 'NONE', #73572 ) ;
#6157 = EDGE_CURVE ( 'NONE', #1899, #106239, #65697, .T. ) ;
#6158 = CARTESIAN_POINT ( 'NONE',  ( 179.5000000000000000, 0.000000000000000000, 0.000000000000000000 ) ) ;
#6159 = ORIENTED_EDGE ( 'NONE', *, *, #49847, .T. ) ;
#6160 = ORIENTED_EDGE ( 'NONE', *, *, #105601, .F. ) ;
#6161 = CIRCLE ( 'NONE', #79350, 0.1000000000000002554 ) ;
#6162 = DIRECTION ( 'NONE',  ( -0.000000000000000000, -1.000000000000000000, -0.000000000000000000 ) ) ;
#6163 = ADVANCED_FACE ( 'NONE', ( #15935 ), #20795, .T. ) ;
#6164 = CARTESIAN_POINT ( 'NONE',  ( -0.4000000000000392131, 2.500000000000000000, -5.022947341949754119 ) ) ;
#6165 = CARTESIAN_POINT ( 'NONE',  ( 12.29999999999990479, 12.50000000000000000, -3.983716857408426293 ) ) ;
#6166 = DIRECTION ( 'NONE',  ( 0.000000000000000000, 0.000000000000000000, -1.000000000000000000 ) ) ;
#6167 = FACE_OUTER_BOUND ( 'NONE', #74923, .T. ) ;
#6168 = CARTESIAN_POINT ( 'NONE',  ( -2.700000000000029932, 12.50000000000000000, -4.676537180435977881 ) ) ;
#6169 = CONICAL_SURFACE ( 'NONE', #79358, 0.1000000000000002554, 0.003490658503988666988 ) ;
#6170 = EDGE_LOOP ( 'NONE', ( #32732, #28435, #114957, #112577 ) ) ;
#6171 = LINE ( 'NONE', #86013, #1025 ) ;
#6172 = ORIENTED_EDGE ( 'NONE', *, *, #3997, .T. ) ;
#6173 = DIRECTION ( 'NONE',  ( 0.000000000000000000, 0.000000000000000000, 1.000000000000000000 ) ) ;
#6175 = AXIS2_PLACEMENT_3D ( 'NONE', #90120, #119590, #49594 ) ;
#6174 = AXIS2_PLACEMENT_3D ( 'NONE', #82215, #30558, #71102 ) ;
#6176 = EDGE_LOOP ( 'NONE', ( #25164, #59153, #99939, #22610 ) ) ;
#6177 = CARTESIAN_POINT ( 'NONE',  ( 5.449999999999937117, 2.500000000000000000, -6.395190528383301931 ) ) ;
#6178 = FACE_OUTER_BOUND ( 'NONE', #115819, .T. ) ;
#6179 = ORIENTED_EDGE ( 'NONE', *, *, #12622, .F. ) ;
#6180 = AXIS2_PLACEMENT_3D ( 'NONE', #2254, #22583, #73573 ) ;
#6181 = FACE_OUTER_BOUND ( 'NONE', #28408, .T. ) ;
#6182 = DIRECTION ( 'NONE',  ( -4.274815082592931898E-19, -0.9999939076577903929, -0.003490651415223739937 ) ) ;
#6183 = ORIENTED_EDGE ( 'NONE', *, *, #93164, .F. ) ;
#6184 = DIRECTION ( 'NONE',  ( 0.000000000000000000, 1.000000000000000000, 0.000000000000000000 ) ) ;
#6186 = AXIS2_PLACEMENT_3D ( 'NONE', #8170, #38298, #81278 ) ;
#6185 = CIRCLE ( 'NONE', #8246, 0.06509327318403745899 ) ;
#6187 = PLANE ( 'NONE',  #126036 ) ;
#6188 = ORIENTED_EDGE ( 'NONE', *, *, #57240, .T. ) ;
#6189 = ORIENTED_EDGE ( 'NONE', *, *, #94855, .F. ) ;
#6190 = DIRECTION ( 'NONE',  ( 0.000000000000000000, 1.000000000000000000, 0.000000000000000000 ) ) ;
#6191 = LINE ( 'NONE', #105708, #5411 ) ;
#6192 = CARTESIAN_POINT ( 'NONE',  ( 186.7135416670080872, 4.367472073101518859, -7.564683531249999149 ) ) ;
#6193 = FACE_OUTER_BOUND ( 'NONE', #29991, .T. ) ;
#6194 = EDGE_CURVE ( 'NONE', #33099, #47526, #6744, .T. ) ;
#6195 = DIRECTION ( 'NONE',  ( 0.000000000000000000, 0.000000000000000000, 1.000000000000000000 ) ) ;
#6196 = CARTESIAN_POINT ( 'NONE',  ( -1.900000000000034106, 12.50000000000000000, -3.983716857408426293 ) ) ;
#6197 = ORIENTED_EDGE ( 'NONE', *, *, #71054, .T. ) ;
#6198 = DIRECTION ( 'NONE',  ( 0.000000000000000000, 0.000000000000000000, -1.000000000000000000 ) ) ;
#6199 = VECTOR ( 'NONE', #60908, 1000.000000000000000 ) ;
#6200 = CONICAL_SURFACE ( 'NONE', #114876, 0.1000000000000002554, 0.003490658503988666988 ) ;
#6201 = ORIENTED_EDGE ( 'NONE', *, *, #57822, .F. ) ;
#6202 = EDGE_CURVE ( 'NONE', #113352, #36869, #33336, .T. ) ;
#6203 = CARTESIAN_POINT ( 'NONE',  ( 6.249999999999934275, 2.500000000000000000, -7.188010851410854052 ) ) ;
#6204 = FACE_OUTER_BOUND ( 'NONE', #87816, .T. ) ;
#6205 = ADVANCED_FACE ( 'NONE', ( #95804 ), #112745, .T. ) ;
#6206 = DIRECTION ( 'NONE',  ( -0.000000000000000000, -1.000000000000000000, -0.000000000000000000 ) ) ;
#6207 = CIRCLE ( 'NONE', #91618, 0.06509327318403745899 ) ;
#6208 = VERTEX_POINT ( 'NONE', #95166 ) ;
#6210 = AXIS2_PLACEMENT_3D ( 'NONE', #120480, #19036, #100819 ) ;
#6209 = AXIS2_PLACEMENT_3D ( 'NONE', #65099, #73637, #122116 ) ;
#6211 = DIRECTION ( 'NONE',  ( -4.274815082592931898E-19, -0.9999939076577903929, -0.003490651415223739937 ) ) ;
#6212 = CARTESIAN_POINT ( 'NONE',  ( -7.700000000000016165, 12.50000000000000000, 0.3464101615137735735 ) ) ;
#6213 = ADVANCED_FACE ( 'NONE', ( #114791 ), #41743, .T. ) ;
#6214 = AXIS2_PLACEMENT_3D ( 'NONE', #136, #80003, #119934 ) ;
#6215 = ORIENTED_EDGE ( 'NONE', *, *, #2136, .T. ) ;
#6216 = DIRECTION ( 'NONE',  ( 0.000000000000000000, 0.000000000000000000, 1.000000000000000000 ) ) ;
#6217 = CONICAL_SURFACE ( 'NONE', #14625, 0.09999999999999982514, 0.003490658503988666988 ) ;
#6218 = ORIENTED_EDGE ( 'NONE', *, *, #117354, .F. ) ;
#6219 = VERTEX_POINT ( 'NONE', #34980 ) ;
#6220 = DIRECTION ( 'NONE',  ( 1.000000000000000000, -0.000000000000000000, -0.000000000000000000 ) ) ;
#6221 = VERTEX_POINT ( 'NONE', #54575 ) ;
#6222 = CARTESIAN_POINT ( 'NONE',  ( -0.8500000000000390576, 2.500000000000000000, -2.265063509461101798 ) ) ;
#6223 = PLANE ( 'NONE',  #12941 ) ;
#6224 = DIRECTION ( 'NONE',  ( 0.000000000000000000, 0.000000000000000000, -1.000000000000000000 ) ) ;
#6225 = ORIENTED_EDGE ( 'NONE', *, *, #90568, .T. ) ;
#6226 = FACE_BOUND ( 'NONE', #106653, .T. ) ;
#6228 = EDGE_LOOP ( 'NONE', ( #50551, #78646 ) ) ;
#6227 = CARTESIAN_POINT ( 'NONE',  ( 115.5000000000000000, 2.000000000000000000, 5.000000000000003553 ) ) ;
#6229 = CIRCLE ( 'NONE', #73066, 0.09999999999999982514 ) ;
#6230 = DIRECTION ( 'NONE',  ( 0.000000000000000000, 1.000000000000000000, 0.000000000000000000 ) ) ;
#6231 = CARTESIAN_POINT ( 'NONE',  ( -9.600000000000006750, 2.500000000000000000, 5.122947341949749323 ) ) ;
#6232 = ORIENTED_EDGE ( 'NONE', *, *, #53840, .F. ) ;
#6233 = ADVANCED_FACE ( 'NONE', ( #105634 ), #2001, .T. ) ;
#6234 = EDGE_LOOP ( 'NONE', ( #4418, #50719, #44020, #10855 ) ) ;
#6235 = ORIENTED_EDGE ( 'NONE', *, *, #96124, .T. ) ;
#6236 = DIRECTION ( 'NONE',  ( 0.000000000000000000, 1.000000000000000000, 0.000000000000000000 ) ) ;
#6237 = DIRECTION ( 'NONE',  ( 0.000000000000000000, 0.000000000000000000, 1.000000000000000000 ) ) ;
#6238 = DIRECTION ( 'NONE',  ( 0.000000000000000000, 0.000000000000000000, 1.000000000000000000 ) ) ;
#6239 = ADVANCED_FACE ( 'NONE', ( #65034 ), #114164, .T. ) ;
#6240 = FACE_BOUND ( 'NONE', #102700, .T. ) ;
#6241 = VERTEX_POINT ( 'NONE', #23857 ) ;
#6242 = CARTESIAN_POINT ( 'NONE',  ( 186.8177083336747160, 4.367472073101515306, 7.564683531250000925 ) ) ;
#6243 = ADVANCED_FACE ( 'NONE', ( #55247 ), #110670, .T. ) ;
#6244 = CARTESIAN_POINT ( 'NONE',  ( -3.150000000000030553, 2.500000000000000000, 6.048780366869520364 ) ) ;
#6245 = DIRECTION ( 'NONE',  ( 0.000000000000000000, 1.000000000000000000, 0.000000000000000000 ) ) ;
#6246 = DIRECTION ( 'NONE',  ( 0.000000000000000000, 0.000000000000000000, 1.000000000000000000 ) ) ;
#6247 = EDGE_CURVE ( 'NONE', #103899, #49433, #26430, .T. ) ;
#6248 = CARTESIAN_POINT ( 'NONE',  ( -9.800000000000006040, 2.500000000000000000, 4.576537180435972019 ) ) ;
#6249 = ADVANCED_FACE ( 'NONE', ( #25127 ), #18733, .T. ) ;
#6250 = FACE_OUTER_BOUND ( 'NONE', #16444, .T. ) ;
#6251 = AXIS2_PLACEMENT_3D ( 'NONE', #42080, #45785, #55592 ) ;
#6252 = EDGE_CURVE ( 'NONE', #23628, #64551, #6102, .T. ) ;
#6253 = DIRECTION ( 'NONE',  ( -0.000000000000000000, -1.000000000000000000, -0.000000000000000000 ) ) ;
#6254 = DIRECTION ( 'NONE',  ( -0.000000000000000000, 1.000000000000000000, -0.000000000000000000 ) ) ;
#6255 = CARTESIAN_POINT ( 'NONE',  ( -5.000000000000026645, 12.50000000000000000, -3.702399969078687292 ) ) ;
#6258 = ADVANCED_FACE ( 'NONE', ( #75509 ), #55874, .T. ) ;
#6257 = AXIS2_PLACEMENT_3D ( 'NONE', #63907, #103834, #64541 ) ;
#6256 = AXIS2_PLACEMENT_3D ( 'NONE', #33129, #85430, #33753 ) ;
#6259 = ORIENTED_EDGE ( 'NONE', *, *, #38213, .F. ) ;
#6260 = EDGE_LOOP ( 'NONE', ( #55122, #12281 ) ) ;
#6261 = VERTEX_POINT ( 'NONE', #37543 ) ;
#6262 = VERTEX_POINT ( 'NONE', #89845 ) ;
#6263 = EDGE_LOOP ( 'NONE', ( #87844, #62549 ) ) ;
#6264 = CARTESIAN_POINT ( 'NONE',  ( -4.200000000000025935, 2.500000000000000000, 4.230127018922196669 ) ) ;
#6265 = CARTESIAN_POINT ( 'NONE',  ( -11.64999999999999680, 2.500000000000000000, 7.188010851410848723 ) ) ;
#6266 = ORIENTED_EDGE ( 'NONE', *, *, #38818, .T. ) ;
#6267 = FACE_BOUND ( 'NONE', #26959, .T. ) ;
#6268 = EDGE_CURVE ( 'NONE', #78915, #39292, #60525, .T. ) ;
#6269 = PLANE ( 'NONE',  #33316 ) ;
#6270 = CIRCLE ( 'NONE', #94027, 0.06509327318403745899 ) ;
#6271 = CARTESIAN_POINT ( 'NONE',  ( 2.099999999999948574, 2.500000000000000000, 4.330127018922196314 ) ) ;
#6272 = CARTESIAN_POINT ( 'NONE',  ( -1.450000000000035483, 12.50000000000000000, 6.083687093685483660 ) ) ;
#6273 = CARTESIAN_POINT ( 'NONE',  ( -13.34999999999999076, 12.50000000000000000, 2.857883832488652853 ) ) ;
#6274 = CARTESIAN_POINT ( 'NONE',  ( 5.849999999999935696, 2.500000000000000000, -6.495190528383302464 ) ) ;
#6275 = ORIENTED_EDGE ( 'NONE', *, *, #58862, .T. ) ;
#6276 = CARTESIAN_POINT ( 'NONE',  ( 88.00000000000001421, 0.000000000000000000, 0.000000000000000000 ) ) ;
#6277 = ORIENTED_EDGE ( 'NONE', *, *, #24596, .F. ) ;
#6278 = ORIENTED_EDGE ( 'NONE', *, *, #21936, .T. ) ;
#6279 = ORIENTED_EDGE ( 'NONE', *, *, #99567, .F. ) ;
#6280 = CARTESIAN_POINT ( 'NONE',  ( 11.44999999999990692, 2.500000000000000000, 1.918653347947321564 ) ) ;
#6281 = DIRECTION ( 'NONE',  ( 0.000000000000000000, -0.9999939076577903929, 0.003490651415223739937 ) ) ;
#6282 = FACE_OUTER_BOUND ( 'NONE', #2271, .T. ) ;
#6283 = ORIENTED_EDGE ( 'NONE', *, *, #90346, .T. ) ;
#6284 = CARTESIAN_POINT ( 'NONE',  ( 16.04820284965640909, 1.500000000000000888, -6.585610464672832620 ) ) ;
#6285 = VECTOR ( 'NONE', #106630, 1000.000000000000000 ) ;
#6286 = DIRECTION ( 'NONE',  ( -4.274815082592931898E-19, -0.9999939076577903929, -0.003490651415223739937 ) ) ;
#6287 = AXIS2_PLACEMENT_3D ( 'NONE', #108846, #28377, #19165 ) ;
#6288 = DIRECTION ( 'NONE',  ( 0.000000000000000000, 0.000000000000000000, 1.000000000000000000 ) ) ;
#6289 = CARTESIAN_POINT ( 'NONE',  ( 185.1562500006828031, 8.891194145520236347, 5.444286225454521982E-16 ) ) ;
#6290 = DIRECTION ( 'NONE',  ( 0.000000000000000000, 0.000000000000000000, 1.000000000000000000 ) ) ;
#6291 = FACE_OUTER_BOUND ( 'NONE', #39820, .T. ) ;
#6292 = ORIENTED_EDGE ( 'NONE', *, *, #106100, .F. ) ;
#6293 = CARTESIAN_POINT ( 'NONE',  ( -9.400000000000009237, 12.50000000000000000, -3.918623584224384615 ) ) ;
#6294 = CONICAL_SURFACE ( 'NONE', #119196, 0.1000000000000002554, 0.003490658503988666988 ) ;
#6295 = ORIENTED_EDGE ( 'NONE', *, *, #30584, .T. ) ;
#6296 = ADVANCED_FACE ( 'NONE', ( #36897 ), #16561, .T. ) ;
#6297 = ORIENTED_EDGE ( 'NONE', *, *, #15863, .F. ) ;
#6298 = FACE_OUTER_BOUND ( 'NONE', #70262, .T. ) ;
#6299 = CARTESIAN_POINT ( 'NONE',  ( 10.79999999999991012, 12.50000000000000000, 4.330127018922196314 ) ) ;
#6300 = DIRECTION ( 'NONE',  ( 0.000000000000000000, 0.000000000000000000, 1.000000000000000000 ) ) ;
#6301 = CONICAL_SURFACE ( 'NONE', #75277, 0.1000000000000002554, 0.003490658503988666988 ) ;
#6302 = EDGE_LOOP ( 'NONE', ( #85111, #51502 ) ) ;
#6303 = VERTEX_POINT ( 'NONE', #76817 ) ;
#6304 = EDGE_CURVE ( 'NONE', #34635, #79439, #116723, .T. ) ;
#6305 = AXIS2_PLACEMENT_3D ( 'NONE', #84477, #104735, #4584 ) ;
#6306 = DIRECTION ( 'NONE',  ( 0.000000000000000000, 1.000000000000000000, 0.000000000000000000 ) ) ;
#6307 = CIRCLE ( 'NONE', #23067, 0.1000000000000002554 ) ;
#6308 = LINE ( 'NONE', #17422, #110108 ) ;
#6309 = CARTESIAN_POINT ( 'NONE',  ( -10.00000000000000533, 2.500000000000000000, 4.922947341949748257 ) ) ;
#6310 = ORIENTED_EDGE ( 'NONE', *, *, #3382, .T. ) ;
#6311 = ORIENTED_EDGE ( 'NONE', *, *, #65356, .T. ) ;
#6312 = CARTESIAN_POINT ( 'NONE',  ( 7.499999999999925393, 2.500000000000000000, -0.7928203230275542301 ) ) ;
#6313 = VERTEX_POINT ( 'NONE', #27071 ) ;
#6314 = FACE_OUTER_BOUND ( 'NONE', #114419, .T. ) ;
#6315 = CARTESIAN_POINT ( 'NONE',  ( 10.84999999999991260, 12.50000000000000000, 6.495190528383297135 ) ) ;
#6316 = EDGE_LOOP ( 'NONE', ( #24358, #31006, #438, #91883 ) ) ;
#6317 = DIRECTION ( 'NONE',  ( 0.000000000000000000, 1.000000000000000000, 0.000000000000000000 ) ) ;
#6318 = DIRECTION ( 'NONE',  ( -0.000000000000000000, 1.000000000000000000, -0.000000000000000000 ) ) ;
#6319 = AXIS2_PLACEMENT_3D ( 'NONE', #26879, #56961, #79216 ) ;
#6320 = FACE_OUTER_BOUND ( 'NONE', #87531, .T. ) ;
#6321 = LINE ( 'NONE', #106485, #91823 ) ;
#6322 = VERTEX_POINT ( 'NONE', #89207 ) ;
#6323 = CARTESIAN_POINT ( 'NONE',  ( 7.049999999999930544, 12.50000000000000000, -6.495190528383302464 ) ) ;
#6324 = CARTESIAN_POINT ( 'NONE',  ( -8.750000000000010658, 2.500000000000000000, -7.188010851410848723 ) ) ;
#6325 = ORIENTED_EDGE ( 'NONE', *, *, #106005, .T. ) ;
#6326 = EDGE_LOOP ( 'NONE', ( #40917, #44270, #49656, #83862 ) ) ;
#6327 = CARTESIAN_POINT ( 'NONE',  ( 185.6302083336747444, -4.367472073101514418, -7.564683531250002702 ) ) ;
#6328 = DIRECTION ( 'NONE',  ( 0.000000000000000000, 1.000000000000000000, 0.000000000000000000 ) ) ;
#6329 = CARTESIAN_POINT ( 'NONE',  ( 11.64999999999990798, 12.50000000000000000, -1.537336459617587581 ) ) ;
#6330 = CARTESIAN_POINT ( 'NONE',  ( 8.749999999999920064, 2.500000000000000000, 5.802370205355744659 ) ) ;
#6331 = DIRECTION ( 'NONE',  ( -0.000000000000000000, -1.000000000000000000, -0.000000000000000000 ) ) ;
#6332 = DIRECTION ( 'NONE',  ( -0.000000000000000000, -1.000000000000000000, -0.000000000000000000 ) ) ;
#6333 = EDGE_CURVE ( 'NONE', #81732, #87716, #48645, .T. ) ;
#6334 = CARTESIAN_POINT ( 'NONE',  ( 0.1999999999999576006, 2.500000000000000000, -4.676537180435978769 ) ) ;
#6335 = CARTESIAN_POINT ( 'NONE',  ( 9.349999999999919709, 2.500000000000000000, 2.611473670974873151 ) ) ;
#6336 = DIRECTION ( 'NONE',  ( 0.000000000000000000, 0.000000000000000000, -1.000000000000000000 ) ) ;
#6337 = VECTOR ( 'NONE', #29222, 1000.000000000000000 ) ;
#6338 = AXIS2_PLACEMENT_3D ( 'NONE', #96626, #65893, #76375 ) ;
#6339 = CARTESIAN_POINT ( 'NONE',  ( 12.04999999999990479, 2.500000000000000000, 2.065063509461097624 ) ) ;
#6340 = EDGE_CURVE ( 'NONE', #31984, #83877, #62577, .T. ) ;
#6341 = ORIENTED_EDGE ( 'NONE', *, *, #17805, .F. ) ;
#6342 = CIRCLE ( 'NONE', #94114, 0.1000000000000002554 ) ;
#6343 = ORIENTED_EDGE ( 'NONE', *, *, #51640, .T. ) ;
#6344 = CARTESIAN_POINT ( 'NONE',  ( -4.800000000000024691, 2.500000000000000000, 4.676537180435972552 ) ) ;
#6345 = ADVANCED_FACE ( 'NONE', ( #98368 ), #121141, .T. ) ;
#6346 = EDGE_LOOP ( 'NONE', ( #784, #76761 ) ) ;
#6347 = FACE_OUTER_BOUND ( 'NONE', #86731, .T. ) ;
#6348 = ADVANCED_FACE ( 'NONE', ( #119303 ), #10327, .T. ) ;
#6349 = DIRECTION ( 'NONE',  ( 0.000000000000000000, 0.000000000000000000, -1.000000000000000000 ) ) ;
#6350 = PLANE ( 'NONE',  #110555 ) ;
#6351 = VERTEX_POINT ( 'NONE', #17208 ) ;
#6352 = CARTESIAN_POINT ( 'NONE',  ( -3.350000000000028955, 2.500000000000000000, -2.065063509461102065 ) ) ;
#6353 = EDGE_CURVE ( 'NONE', #89491, #81018, #37529, .T. ) ;
#6354 = DIRECTION ( 'NONE',  ( -4.274815082592931898E-19, -0.9999939076577903929, -0.003490651415223739937 ) ) ;
#6356 = VERTEX_POINT ( 'NONE', #8689 ) ;
#6355 = CARTESIAN_POINT ( 'NONE',  ( -4.400000000000025224, 12.50000000000000000, 3.918623584224382839 ) ) ;
#6357 = ADVANCED_FACE ( 'NONE', ( #78109 ), #27054, .T. ) ;
#6358 = CARTESIAN_POINT ( 'NONE',  ( -0.8500000000000395017, 12.50000000000000000, 6.560283801567334372 ) ) ;
#6359 = VERTEX_POINT ( 'NONE', #118018 ) ;
#6360 = EDGE_LOOP ( 'NONE', ( #121206, #127702 ) ) ;
#6361 = ORIENTED_EDGE ( 'NONE', *, *, #44553, .T. ) ;
#6362 = ORIENTED_EDGE ( 'NONE', *, *, #13925, .T. ) ;
#6363 = DIRECTION ( 'NONE',  ( -0.000000000000000000, 1.000000000000000000, -0.000000000000000000 ) ) ;
#6364 = FACE_OUTER_BOUND ( 'NONE', #25845, .T. ) ;
#6365 = DIRECTION ( 'NONE',  ( 0.000000000000000000, 0.000000000000000000, -1.000000000000000000 ) ) ;
#6366 = CARTESIAN_POINT ( 'NONE',  ( -9.400000000000007461, 2.500000000000000000, 3.883716857408420431 ) ) ;
#6367 = CIRCLE ( 'NONE', #35655, 0.1000000000000002554 ) ;
#6368 = ORIENTED_EDGE ( 'NONE', *, *, #90775, .F. ) ;
#6369 = AXIS2_PLACEMENT_3D ( 'NONE', #86834, #67841, #45643 ) ;
#6370 = DIRECTION ( 'NONE',  ( 0.000000000000000000, 1.000000000000000000, 0.000000000000000000 ) ) ;
#6371 = EDGE_LOOP ( 'NONE', ( #109626, #92049 ) ) ;
#6372 = DIRECTION ( 'NONE',  ( 0.000000000000000000, -0.9999939076577903929, 0.003490651415223739937 ) ) ;
#6373 = CARTESIAN_POINT ( 'NONE',  ( 9.549999999999915445, 2.500000000000000000, -2.165063509461101710 ) ) ;
#6374 = FACE_OUTER_BOUND ( 'NONE', #88000, .T. ) ;
#6375 = CARTESIAN_POINT ( 'NONE',  ( 18.78720903128300179, -2.539625591034222918, 4.564429507521819751 ) ) ;
#6376 = AXIS2_PLACEMENT_3D ( 'NONE', #23300, #12821, #104449 ) ;
#6377 = ORIENTED_EDGE ( 'NONE', *, *, #51164, .T. ) ;
#6378 = EDGE_CURVE ( 'NONE', #41663, #104853, #54245, .T. ) ;
#6379 = VERTEX_POINT ( 'NONE', #57167 ) ;
#6380 = ORIENTED_EDGE ( 'NONE', *, *, #30228, .T. ) ;
#6381 = LINE ( 'NONE', #105915, #2204 ) ;
#6382 = CARTESIAN_POINT ( 'NONE',  ( 2.099999999999949463, 2.500000000000000000, 0.7928203230275495672 ) ) ;
#6383 = DIRECTION ( 'NONE',  ( 0.000000000000000000, 0.000000000000000000, 1.000000000000000000 ) ) ;
#6384 = FACE_BOUND ( 'NONE', #126994, .T. ) ;
#6385 = CARTESIAN_POINT ( 'NONE',  ( -7.050000000000016698, 12.50000000000000000, -2.230156782645139391 ) ) ;
#6386 = DIRECTION ( 'NONE',  ( 0.000000000000000000, 1.000000000000000000, 0.000000000000000000 ) ) ;
#6387 = EDGE_CURVE ( 'NONE', #115596, #14399, #24997, .T. ) ;
#6388 = DIRECTION ( 'NONE',  ( -4.274815082592931898E-19, -0.9999939076577903929, -0.003490651415223739937 ) ) ;
#6389 = CARTESIAN_POINT ( 'NONE',  ( -6.050000000000017586, 12.50000000000000000, 1.818653347947321475 ) ) ;
#6390 = CIRCLE ( 'NONE', #29420, 0.1000000000000000472 ) ;
#6391 = AXIS2_PLACEMENT_3D ( 'NONE', #23311, #103177, #13490 ) ;
#6392 = EDGE_CURVE ( 'NONE', #4409, #71810, #62663, .T. ) ;
#6393 = CARTESIAN_POINT ( 'NONE',  ( 184.8385416670080872, 6.551208109652274736, 3.782341765625001351 ) ) ;
#6394 = LINE ( 'NONE', #76469, #75912 ) ;
#6395 = EDGE_CURVE ( 'NONE', #20773, #90204, #78767, .T. ) ;
#6396 = CARTESIAN_POINT ( 'NONE',  ( -2.950000000000029932, 2.500000000000000000, -2.265063509461101798 ) ) ;
#6397 = EDGE_CURVE ( 'NONE', #64508, #116018, #29016, .T. ) ;
#6398 = CARTESIAN_POINT ( 'NONE',  ( 9.999999999999911182, 12.50000000000000000, 5.022947341949748790 ) ) ;
#6399 = EDGE_CURVE ( 'NONE', #33584, #15359, #12468, .T. ) ;
#6400 = VERTEX_POINT ( 'NONE', #29646 ) ;
#6401 = CONICAL_SURFACE ( 'NONE', #33556, 0.1000000000000002554, 0.003490658503988666988 ) ;
#6402 = ORIENTED_EDGE ( 'NONE', *, *, #36594, .T. ) ;
#6403 = VERTEX_POINT ( 'NONE', #69559 ) ;
#6404 = ORIENTED_EDGE ( 'NONE', *, *, #16180, .F. ) ;
#6405 = CARTESIAN_POINT ( 'NONE',  ( -9.150000000000011013, 12.50000000000000000, -5.802370205355744659 ) ) ;
#6406 = FACE_BOUND ( 'NONE', #56960, .T. ) ;
#6407 = CARTESIAN_POINT ( 'NONE',  ( -14.14999999999998614, 12.50000000000000000, -2.792790559304614284 ) ) ;
#6408 = ADVANCED_FACE ( 'NONE', ( #127214 ), #67619, .T. ) ;
#6409 = DIRECTION ( 'NONE',  ( -4.274815082592931898E-19, -0.9999939076577903929, -0.003490651415223739937 ) ) ;
#6410 = EDGE_CURVE ( 'NONE', #78664, #69133, #29220, .T. ) ;
#6411 = ORIENTED_EDGE ( 'NONE', *, *, #9554, .T. ) ;
#6412 = DIRECTION ( 'NONE',  ( -0.000000000000000000, 1.000000000000000000, -0.000000000000000000 ) ) ;
#6413 = FACE_OUTER_BOUND ( 'NONE', #119717, .T. ) ;
#6414 = EDGE_LOOP ( 'NONE', ( #14323, #45218, #67471, #117364 ) ) ;
#6415 = CARTESIAN_POINT ( 'NONE',  ( -11.64999999999999680, 12.50000000000000000, 5.802370205355744659 ) ) ;
#6416 = CARTESIAN_POINT ( 'NONE',  ( -0.6000000000000388356, 12.50000000000000000, 4.676537180435972552 ) ) ;
#6417 = CIRCLE ( 'NONE', #31603, 0.1000000000000002554 ) ;
#6418 = VERTEX_POINT ( 'NONE', #20479 ) ;
#6419 = CIRCLE ( 'NONE', #115093, 0.1000000000000000472 ) ;
#6420 = CARTESIAN_POINT ( 'NONE',  ( 7.099999999999928590, 2.500000000000000000, -4.330127018922201643 ) ) ;
#6421 = AXIS2_PLACEMENT_3D ( 'NONE', #117548, #58029, #27912 ) ;
#6422 = CARTESIAN_POINT ( 'NONE',  ( 8.549999999999922551, 12.50000000000000000, -6.083687093685488989 ) ) ;
#6423 = EDGE_LOOP ( 'NONE', ( #71379, #13587, #44285, #93788 ) ) ;
#6424 = CARTESIAN_POINT ( 'NONE',  ( 4.599999999999935696, 12.50000000000000000, 5.022947341949748790 ) ) ;
#6425 = CIRCLE ( 'NONE', #48234, 0.06509327318403745899 ) ;
#6426 = DIRECTION ( 'NONE',  ( 0.000000000000000000, 0.000000000000000000, -1.000000000000000000 ) ) ;
#6427 = EDGE_LOOP ( 'NONE', ( #43668, #291, #88358, #117742 ) ) ;
#6428 = CARTESIAN_POINT ( 'NONE',  ( 6.049999999999932321, 2.500000000000000000, 1.718653347947321386 ) ) ;
#6429 = ORIENTED_EDGE ( 'NONE', *, *, #10659, .F. ) ;
#6430 = AXIS2_PLACEMENT_3D ( 'NONE', #91978, #120155, #61893 ) ;
#6431 = ORIENTED_EDGE ( 'NONE', *, *, #38676, .F. ) ;
#6432 = DIRECTION ( 'NONE',  ( 0.000000000000000000, 0.000000000000000000, -1.000000000000000000 ) ) ;
#6433 = VERTEX_POINT ( 'NONE', #71496 ) ;
#6434 = CARTESIAN_POINT ( 'NONE',  ( 5.399999999999934630, 12.50000000000000000, -0.6928203230275542523 ) ) ;
#6435 = DIRECTION ( 'NONE',  ( -0.000000000000000000, -1.000000000000000000, -0.000000000000000000 ) ) ;
#6436 = ORIENTED_EDGE ( 'NONE', *, *, #94768, .F. ) ;
#6437 = ADVANCED_FACE ( 'NONE', ( #102880 ), #68901, .T. ) ;
#6438 = CARTESIAN_POINT ( 'NONE',  ( -3.750000000000025757, 2.500000000000000000, -2.957883832488653830 ) ) ;
#6439 = CARTESIAN_POINT ( 'NONE',  ( 87.50000000000001421, 0.000000000000000000, 0.000000000000000000 ) ) ;
#6440 = FACE_OUTER_BOUND ( 'NONE', #24489, .T. ) ;
#6441 = CARTESIAN_POINT ( 'NONE',  ( 12.69999999999989804, 2.500000000000000000, 0.2464101615137735679 ) ) ;
#6442 = CARTESIAN_POINT ( 'NONE',  ( 7.299999999999926104, 2.500000000000000000, -3.983716857408426293 ) ) ;
#6443 = LINE ( 'NONE', #28063, #129043 ) ;
#6444 = ORIENTED_EDGE ( 'NONE', *, *, #126262, .F. ) ;
#6445 = EDGE_CURVE ( 'NONE', #5618, #39246, #119088, .T. ) ;
#6446 = ORIENTED_EDGE ( 'NONE', *, *, #52449, .F. ) ;
#6447 = CONICAL_SURFACE ( 'NONE', #27393, 0.09999999999999982514, 0.003490658503988666988 ) ;
#6448 = DIRECTION ( 'NONE',  ( 0.000000000000000000, 0.000000000000000000, 1.000000000000000000 ) ) ;
#6449 = CARTESIAN_POINT ( 'NONE',  ( -13.14999999999999147, 2.500000000000000000, 2.511473670974877503 ) ) ;
#6450 = DIRECTION ( 'NONE',  ( 0.000000000000000000, 0.000000000000000000, 1.000000000000000000 ) ) ;
#6452 = EDGE_LOOP ( 'NONE', ( #11839, #48250 ) ) ;
#6451 = EDGE_LOOP ( 'NONE', ( #127899, #7119, #67171, #70156 ) ) ;
#6453 = VERTEX_POINT ( 'NONE', #60419 ) ;
#6454 = DIRECTION ( 'NONE',  ( -0.000000000000000000, -1.000000000000000000, -0.000000000000000000 ) ) ;
#6455 = CONICAL_SURFACE ( 'NONE', #48353, 0.1000000000000002554, 0.003490658503988666988 ) ;
#6456 = DIRECTION ( 'NONE',  ( 0.000000000000000000, -0.000000000000000000, 1.000000000000000000 ) ) ;
#6457 = AXIS2_PLACEMENT_3D ( 'NONE', #91997, #21990, #61910 ) ;
#6458 = CARTESIAN_POINT ( 'NONE',  ( 0.3999999999999628852, 12.50000000000000000, 0.6277270498435143509 ) ) ;
#6459 =( NAMED_UNIT ( * ) PLANE_ANGLE_UNIT ( ) SI_UNIT ( $, .RADIAN. ) );
#6460 = DIRECTION ( 'NONE',  ( 0.000000000000000000, 0.000000000000000000, -1.000000000000000000 ) ) ;
#6461 = DIRECTION ( 'NONE',  ( -4.274815082592931898E-19, -0.9999939076577903929, -0.003490651415223739937 ) ) ;
#6462 = LINE ( 'NONE', #97461, #63228 ) ;
#6463 = DIRECTION ( 'NONE',  ( -0.000000000000000000, 1.000000000000000000, -0.000000000000000000 ) ) ;
#6464 = DIRECTION ( 'NONE',  ( 0.000000000000000000, -0.9999939076577903929, 0.003490651415223739937 ) ) ;
#6466 = AXIS2_PLACEMENT_3D ( 'NONE', #102314, #120656, #40171 ) ;
#6465 = CARTESIAN_POINT ( 'NONE',  ( 11.89999999999990798, 2.500000000000000000, 4.676537180435972552 ) ) ;
#6467 = CIRCLE ( 'NONE', #62937, 0.09999999999999982514 ) ;
#6468 = ORIENTED_EDGE ( 'NONE', *, *, #128749, .F. ) ;
#6469 = DIRECTION ( 'NONE',  ( 0.000000000000000000, 1.000000000000000000, 0.000000000000000000 ) ) ;
#6470 = ORIENTED_EDGE ( 'NONE', *, *, #4044, .T. ) ;
#6471 = ORIENTED_EDGE ( 'NONE', *, *, #108780, .F. ) ;
#6472 = DIRECTION ( 'NONE',  ( -0.000000000000000000, -1.000000000000000000, -0.000000000000000000 ) ) ;
#6473 = DIRECTION ( 'NONE',  ( 0.000000000000000000, 0.000000000000000000, 1.000000000000000000 ) ) ;
#6474 = DIRECTION ( 'NONE',  ( -0.000000000000000000, 1.000000000000000000, -0.000000000000000000 ) ) ;
#6475 = CONICAL_SURFACE ( 'NONE', #67118, 0.1000000000000002554, 0.003490658503988666988 ) ;
#6476 = CARTESIAN_POINT ( 'NONE',  ( -9.550000000000006040, 2.500000000000000000, -2.165063509461101710 ) ) ;
#6477 = CIRCLE ( 'NONE', #104786, 0.1000000000000002554 ) ;
#6479 = DIRECTION ( 'NONE',  ( 0.000000000000000000, 0.000000000000000000, 1.000000000000000000 ) ) ;
#6478 = PRODUCT_DEFINITION_SHAPE ( 'NONE', 'NONE',  #129619 ) ;
#6480 = DIRECTION ( 'NONE',  ( 0.000000000000000000, 0.000000000000000000, 1.000000000000000000 ) ) ;
#6481 = DIRECTION ( 'NONE',  ( 0.000000000000000000, -0.9999939076577903929, 0.003490651415223739937 ) ) ;
#6482 = VERTEX_POINT ( 'NONE', #32888 ) ;
#6483 = CARTESIAN_POINT ( 'NONE',  ( 10.84999999999990905, 12.50000000000000000, -5.867463478539787225 ) ) ;
#6484 = AXIS2_PLACEMENT_3D ( 'NONE', #31232, #11568, #10898 ) ;
#6485 = DIRECTION ( 'NONE',  ( -0.000000000000000000, 1.000000000000000000, -0.000000000000000000 ) ) ;
#6486 = VERTEX_POINT ( 'NONE', #72799 ) ;
#6487 = EDGE_CURVE ( 'NONE', #37790, #51184, #26198, .T. ) ;
#6488 = ORIENTED_EDGE ( 'NONE', *, *, #982, .F. ) ;
#6489 = CIRCLE ( 'NONE', #102664, 0.09999999999999999167 ) ;
#6490 = AXIS2_PLACEMENT_3D ( 'NONE', #62707, #63983, #3773 ) ;
#6491 = ORIENTED_EDGE ( 'NONE', *, *, #75975, .T. ) ;
#6492 = ADVANCED_FACE ( 'NONE', ( #21769 ), #88890, .T. ) ;
#6493 = EDGE_LOOP ( 'NONE', ( #105466, #18695, #8857, #57515 ) ) ;
#6494 = EDGE_CURVE ( 'NONE', #45172, #96595, #17867, .T. ) ;
#6495 = PLANE ( 'NONE',  #123553 ) ;
#6496 = DIRECTION ( 'NONE',  ( 0.000000000000000000, 1.000000000000000000, 0.000000000000000000 ) ) ;
#6497 = ORIENTED_EDGE ( 'NONE', *, *, #14737, .F. ) ;
#6498 = DIRECTION ( 'NONE',  ( -0.000000000000000000, 1.000000000000000000, -0.000000000000000000 ) ) ;
#6499 = CARTESIAN_POINT ( 'NONE',  ( 17.50000000000000000, -2.750000000000000444, -3.432456362931489036 ) ) ;
#6500 = EDGE_CURVE ( 'NONE', #62269, #62754, #78542, .T. ) ;
#6501 = FACE_OUTER_BOUND ( 'NONE', #94225, .T. ) ;
#6503 = ORIENTED_EDGE ( 'NONE', *, *, #114097, .T. ) ;
#6502 = EDGE_CURVE ( 'NONE', #114203, #1725, #91040, .T. ) ;
#6504 = EDGE_CURVE ( 'NONE', #76324, #89801, #22105, .T. ) ;
#6505 = CARTESIAN_POINT ( 'NONE',  ( 10.19999999999991225, 12.50000000000000000, -4.676537180435978769 ) ) ;
#6506 = PLANE ( 'NONE',  #114691 ) ;
#6507 = ORIENTED_EDGE ( 'NONE', *, *, #41884, .F. ) ;
#6508 = VERTEX_POINT ( 'NONE', #165 ) ;
#6509 = EDGE_LOOP ( 'NONE', ( #47226, #16697 ) ) ;
#6510 = CIRCLE ( 'NONE', #23263, 0.06509327318403745899 ) ;
#6511 = DIRECTION ( 'NONE',  ( 1.000000000000000000, -0.000000000000000000, -0.000000000000000000 ) ) ;
#6512 = CIRCLE ( 'NONE', #108935, 0.06509327318403745899 ) ;
#6513 = CARTESIAN_POINT ( 'NONE',  ( -5.000000000000022204, 12.50000000000000000, 3.637306695894644726 ) ) ;
#6514 = VECTOR ( 'NONE', #22994, 1000.000000000000000 ) ;
#6515 = CIRCLE ( 'NONE', #14928, 0.09999999999999982514 ) ;
#6517 = ORIENTED_EDGE ( 'NONE', *, *, #62871, .T. ) ;
#6516 = AXIS2_PLACEMENT_3D ( 'NONE', #98406, #48047, #29058 ) ;
#6518 = DIRECTION ( 'NONE',  ( -0.000000000000000000, -1.000000000000000000, -0.000000000000000000 ) ) ;
#6519 = DIRECTION ( 'NONE',  ( 0.000000000000000000, 0.000000000000000000, 1.000000000000000000 ) ) ;
#6520 = DIRECTION ( 'NONE',  ( -0.000000000000000000, 1.000000000000000000, -0.000000000000000000 ) ) ;
#6521 = PLANE ( 'NONE',  #69180 ) ;
#6522 = ORIENTED_EDGE ( 'NONE', *, *, #118697, .F. ) ;
#6523 = DIRECTION ( 'NONE',  ( 0.000000000000000000, 1.000000000000000000, 0.000000000000000000 ) ) ;
#6524 = ORIENTED_EDGE ( 'NONE', *, *, #117499, .F. ) ;
#6525 = ORIENTED_EDGE ( 'NONE', *, *, #127328, .T. ) ;
#6526 = ORIENTED_EDGE ( 'NONE', *, *, #72536, .F. ) ;
#6527 = DIRECTION ( 'NONE',  ( 0.000000000000000000, 0.000000000000000000, -1.000000000000000000 ) ) ;
#6528 = FACE_BOUND ( 'NONE', #8316, .T. ) ;
#6529 = CARTESIAN_POINT ( 'NONE',  ( -10.80000000000000071, 2.500000000000000000, -0.1000000000000022815 ) ) ;
#6530 = DIRECTION ( 'NONE',  ( 0.000000000000000000, 1.000000000000000000, 0.000000000000000000 ) ) ;
#6531 = DIRECTION ( 'NONE',  ( 0.000000000000000000, 0.000000000000000000, -1.000000000000000000 ) ) ;
#6532 = ADVANCED_FACE ( 'NONE', ( #11928 ), #36678, .T. ) ;
#6533 = VERTEX_POINT ( 'NONE', #62340 ) ;
#6534 = EDGE_CURVE ( 'NONE', #118617, #125586, #28351, .T. ) ;
#6535 = CARTESIAN_POINT ( 'NONE',  ( 3.149999999999946176, 12.50000000000000000, -1.818653347947325916 ) ) ;
#6536 = DIRECTION ( 'NONE',  ( 0.000000000000000000, 1.000000000000000000, 0.000000000000000000 ) ) ;
#6537 = CARTESIAN_POINT ( 'NONE',  ( -0.6500000000000403233, 2.500000000000000000, 1.918653347947321564 ) ) ;
#6538 = ADVANCED_FACE ( 'NONE', ( #70220 ), #57600, .T. ) ;
#6539 = DIRECTION ( 'NONE',  ( 0.000000000000000000, -0.9999939076577903929, 0.003490651415223739937 ) ) ;
#6540 = ORIENTED_EDGE ( 'NONE', *, *, #115589, .F. ) ;
#6541 = AXIS2_PLACEMENT_3D ( 'NONE', #27957, #8300, #7655 ) ;
#6542 = CARTESIAN_POINT ( 'NONE',  ( 5.649999999999934630, 2.500000000000000000, 6.941600689897073018 ) ) ;
#6543 = AXIS2_PLACEMENT_3D ( 'NONE', #95226, #114839, #97793 ) ;
#6544 = FACE_BOUND ( 'NONE', #57159, .T. ) ;
#6545 = EDGE_CURVE ( 'NONE', #98108, #100426, #41420, .T. ) ;
#6546 = EDGE_LOOP ( 'NONE', ( #3089, #30733 ) ) ;
#6547 = LINE ( 'NONE', #83232, #56511 ) ;
#6548 = EDGE_CURVE ( 'NONE', #69648, #7472, #55442, .T. ) ;
#6549 = DIRECTION ( 'NONE',  ( -0.000000000000000000, -1.000000000000000000, -0.000000000000000000 ) ) ;
#6550 = FACE_BOUND ( 'NONE', #82283, .T. ) ;
#6551 = AXIS2_PLACEMENT_3D ( 'NONE', #85116, #15724, #35386 ) ;
#6552 = FACE_OUTER_BOUND ( 'NONE', #95018, .T. ) ;
#6553 = EDGE_CURVE ( 'NONE', #65577, #10375, #105621, .T. ) ;
#6554 = AXIS2_PLACEMENT_3D ( 'NONE', #15673, #65430, #45168 ) ;
#6555 = EDGE_CURVE ( 'NONE', #109761, #117860, #126550, .T. ) ;
#6556 = EDGE_CURVE ( 'NONE', #116101, #78026, #45082, .T. ) ;
#6557 = ORIENTED_EDGE ( 'NONE', *, *, #40144, .T. ) ;
#6559 = CARTESIAN_POINT ( 'NONE',  ( -3.150000000000030109, 2.500000000000000000, -2.511473670974877948 ) ) ;
#6558 = CIRCLE ( 'NONE', #115330, 0.06509327318403745899 ) ;
#6560 = DIRECTION ( 'NONE',  ( -0.000000000000000000, -1.000000000000000000, -0.000000000000000000 ) ) ;
#6561 = ORIENTED_EDGE ( 'NONE', *, *, #89308, .T. ) ;
#6562 =( BOUNDED_CURVE ( )  B_SPLINE_CURVE ( 2, ( #18099, #59347, #10225 ),
 .UNSPECIFIED., .F., .F. ) 
 B_SPLINE_CURVE_WITH_KNOTS ( ( 3, 3 ),
 ( 0.000000000000000000, 8.005299705368666859E-05 ),
 .UNSPECIFIED. ) 
 CURVE ( )  GEOMETRIC_REPRESENTATION_ITEM ( )  RATIONAL_B_SPLINE_CURVE ( ( 1.000000000000000000, 0.9972072019273802157, 0.9944676636817105786 ) ) 
 REPRESENTATION_ITEM ( '' )  );
#6563 = ORIENTED_EDGE ( 'NONE', *, *, #82060, .F. ) ;
#6564 = CARTESIAN_POINT ( 'NONE',  ( 186.2916666666666856, 4.445597072760120838, -7.699999999999998401 ) ) ;
#6565 = ADVANCED_FACE ( 'NONE', ( #122544 ), #82647, .T. ) ;
#6566 = ORIENTED_EDGE ( 'NONE', *, *, #51665, .T. ) ;
#6567 = CARTESIAN_POINT ( 'NONE',  ( 185.7552083336747444, 6.551208109652275624, -3.782341765624998686 ) ) ;
#6568 = CARTESIAN_POINT ( 'NONE',  ( 12.69999999999989804, 2.500000000000000000, 0.3464101615137735735 ) ) ;
#6569 = AXIS2_PLACEMENT_3D ( 'NONE', #34697, #113884, #24213 ) ;
#6570 = AXIS2_PLACEMENT_3D ( 'NONE', #17853, #27660, #77425 ) ;
#6571 = CIRCLE ( 'NONE', #29593, 0.06509327318403745899 ) ;
#6572 = CARTESIAN_POINT ( 'NONE',  ( 185.5312500006828031, 9.429780353434619030E-16, -7.700000000000000178 ) ) ;
#6573 = CARTESIAN_POINT ( 'NONE',  ( 10.84999999999991260, 2.500000000000000000, -2.757883832488654097 ) ) ;
#6574 = AXIS2_PLACEMENT_3D ( 'NONE', #103013, #82092, #70987 ) ;
#6575 = ORIENTED_EDGE ( 'NONE', *, *, #22355, .F. ) ;
#6576 = DIRECTION ( 'NONE',  ( 0.000000000000000000, 1.000000000000000000, 0.000000000000000000 ) ) ;
#6577 = CIRCLE ( 'NONE', #79781, 0.09999999999999982514 ) ;
#6578 = FACE_OUTER_BOUND ( 'NONE', #43131, .T. ) ;
#6579 = CARTESIAN_POINT ( 'NONE',  ( -9.800000000000006040, 2.500000000000000000, -4.776537180435973973 ) ) ;
#6580 = CARTESIAN_POINT ( 'NONE',  ( -1.650000000000034772, 2.500000000000000000, 1.472243186433545459 ) ) ;
#6582 = ORIENTED_EDGE ( 'NONE', *, *, #109428, .F. ) ;
#6581 = ORIENTED_EDGE ( 'NONE', *, *, #66384, .T. ) ;
#6583 = FACE_BOUND ( 'NONE', #9146, .T. ) ;
#6584 = EDGE_LOOP ( 'NONE', ( #52544, #19070, #105238, #83919 ) ) ;
#6585 = DIRECTION ( 'NONE',  ( -0.000000000000000000, 1.000000000000000000, -0.000000000000000000 ) ) ;
#6586 = DIRECTION ( 'NONE',  ( 0.000000000000000000, -0.9999939076577903929, 0.003490651415223739937 ) ) ;
#6587 = EDGE_LOOP ( 'NONE', ( #99362, #25948 ) ) ;
#6588 = CARTESIAN_POINT ( 'NONE',  ( -10.40000000000000213, 2.500000000000000000, 0.5928203230275495006 ) ) ;
#6589 = CARTESIAN_POINT ( 'NONE',  ( 0.8499999999999553468, 12.50000000000000000, 2.165063509461097713 ) ) ;
#6590 = DIRECTION ( 'NONE',  ( 0.000000000000000000, 0.000000000000000000, 1.000000000000000000 ) ) ;
#6591 = FACE_OUTER_BOUND ( 'NONE', #55548, .T. ) ;
#6592 = ORIENTED_EDGE ( 'NONE', *, *, #106322, .F. ) ;
#6593 = DIRECTION ( 'NONE',  ( -0.000000000000000000, 1.000000000000000000, -0.000000000000000000 ) ) ;
#6594 = DIRECTION ( 'NONE',  ( -0.000000000000000000, -1.000000000000000000, -0.000000000000000000 ) ) ;
#6595 = CARTESIAN_POINT ( 'NONE',  ( 186.5260416670080588, -6.551208109652273848, -3.782341765625003571 ) ) ;
#6596 = DIRECTION ( 'NONE',  ( 0.000000000000000000, 0.000000000000000000, 1.000000000000000000 ) ) ;
#6597 = DIRECTION ( 'NONE',  ( 0.000000000000000000, 1.000000000000000000, 0.000000000000000000 ) ) ;
#6598 = VERTEX_POINT ( 'NONE', #26276 ) ;
#6599 = EDGE_CURVE ( 'NONE', #105502, #56688, #109820, .T. ) ;
#6600 = ORIENTED_EDGE ( 'NONE', *, *, #25923, .T. ) ;
#6601 = CARTESIAN_POINT ( 'NONE',  ( -5.850000000000021849, 12.50000000000000000, -1.407149913249512663 ) ) ;
#6602 = ORIENTED_EDGE ( 'NONE', *, *, #4953, .F. ) ;
#6603 = AXIS2_PLACEMENT_3D ( 'NONE', #1751, #20762, #111719 ) ;
#6604 = DIRECTION ( 'NONE',  ( -0.000000000000000000, -1.000000000000000000, -0.000000000000000000 ) ) ;
#6605 = CONICAL_SURFACE ( 'NONE', #10819, 0.1000000000000002554, 0.003490658503988666988 ) ;
#6606 = CIRCLE ( 'NONE', #98560, 0.1000000000000002554 ) ;
#6608 = EDGE_LOOP ( 'NONE', ( #50453, #66755, #8810, #1426 ) ) ;
#6607 = ORIENTED_EDGE ( 'NONE', *, *, #2981, .F. ) ;
#6609 = ORIENTED_EDGE ( 'NONE', *, *, #77091, .F. ) ;
#6610 = DIRECTION ( 'NONE',  ( 0.000000000000000000, 1.000000000000000000, 0.000000000000000000 ) ) ;
#6611 = DIRECTION ( 'NONE',  ( 0.000000000000000000, 1.000000000000000000, 0.000000000000000000 ) ) ;
#6612 = VECTOR ( 'NONE', #82419, 1000.000000000000000 ) ;
#6613 = DIRECTION ( 'NONE',  ( 0.000000000000000000, 0.000000000000000000, 1.000000000000000000 ) ) ;
#6614 = AXIS2_PLACEMENT_3D ( 'NONE', #47880, #37415, #74272 ) ;
#6615 = CARTESIAN_POINT ( 'NONE',  ( 1.449999999999952216, 12.50000000000000000, -2.511473670974877948 ) ) ;
#6616 = CARTESIAN_POINT ( 'NONE',  ( -7.050000000000016698, 2.500000000000000000, -2.165063509461101710 ) ) ;
#6617 = CIRCLE ( 'NONE', #33840, 0.06509327318403745899 ) ;
#6618 = DIRECTION ( 'NONE',  ( 0.000000000000000000, 1.000000000000000000, 0.000000000000000000 ) ) ;
#6619 = VERTEX_POINT ( 'NONE', #123191 ) ;
#6620 = DIRECTION ( 'NONE',  ( 0.000000000000000000, 0.000000000000000000, 1.000000000000000000 ) ) ;
#6622 = ORIENTED_EDGE ( 'NONE', *, *, #108928, .T. ) ;
#6621 = AXIS2_PLACEMENT_3D ( 'NONE', #55391, #126049, #114937 ) ;
#6623 = ORIENTED_EDGE ( 'NONE', *, *, #14945, .T. ) ;
#6624 = EDGE_LOOP ( 'NONE', ( #45357, #1540 ) ) ;
#6625 = ORIENTED_EDGE ( 'NONE', *, *, #38352, .T. ) ;
#6626 = DIRECTION ( 'NONE',  ( 0.000000000000000000, 0.000000000000000000, 1.000000000000000000 ) ) ;
#6627 = ORIENTED_EDGE ( 'NONE', *, *, #94490, .T. ) ;
#6628 = VERTEX_POINT ( 'NONE', #75354 ) ;
#6629 = DIRECTION ( 'NONE',  ( 0.000000000000000000, 1.000000000000000000, 0.000000000000000000 ) ) ;
#6630 = CARTESIAN_POINT ( 'NONE',  ( 12.29999999999990301, 2.500000000000000000, -0.4464101615137782142 ) ) ;
#6631 = CARTESIAN_POINT ( 'NONE',  ( -5.650000000000019895, 12.50000000000000000, 1.818653347947321475 ) ) ;
#6632 = DIRECTION ( 'NONE',  ( 0.000000000000000000, 1.000000000000000000, 0.000000000000000000 ) ) ;
#6633 = DIRECTION ( 'NONE',  ( -0.000000000000000000, -1.000000000000000000, -0.000000000000000000 ) ) ;
#6634 = ORIENTED_EDGE ( 'NONE', *, *, #8310, .F. ) ;
#6635 = DIRECTION ( 'NONE',  ( 0.000000000000000000, 0.000000000000000000, 1.000000000000000000 ) ) ;
#6636 = AXIS2_PLACEMENT_3D ( 'NONE', #74967, #52741, #122154 ) ;
#6637 = CONICAL_SURFACE ( 'NONE', #54679, 0.09999999999999999167, 0.003490658503988666988 ) ;
#6638 = VERTEX_POINT ( 'NONE', #113354 ) ;
#6639 = DIRECTION ( 'NONE',  ( 0.000000000000000000, 0.000000000000000000, 1.000000000000000000 ) ) ;
#6640 = ADVANCED_FACE ( 'NONE', ( #14492 ), #65897, .T. ) ;
#6641 = EDGE_LOOP ( 'NONE', ( #74783, #94757 ) ) ;
#6642 = DIRECTION ( 'NONE',  ( 0.000000000000000000, 0.000000000000000000, -1.000000000000000000 ) ) ;
#6643 = ORIENTED_EDGE ( 'NONE', *, *, #21784, .T. ) ;
#6644 = ADVANCED_FACE ( 'NONE', ( #114637 ), #95652, .T. ) ;
#6645 = ORIENTED_EDGE ( 'NONE', *, *, #51280, .F. ) ;
#6646 = AXIS2_PLACEMENT_3D ( 'NONE', #2358, #32519, #23303 ) ;
#6647 = ADVANCED_FACE ( 'NONE', ( #64888 ), #128628, .T. ) ;
#6648 = DIRECTION ( 'NONE',  ( 0.000000000000000000, 1.000000000000000000, 0.000000000000000000 ) ) ;
#6649 = PLANE ( 'NONE',  #119547 ) ;
#6650 = AXIS2_PLACEMENT_3D ( 'NONE', #52699, #122098, #70413 ) ;
#6651 = AXIS2_PLACEMENT_3D ( 'NONE', #37455, #45987, #56427 ) ;
#6652 = LINE ( 'NONE', #126475, #13170 ) ;
#6653 = CARTESIAN_POINT ( 'NONE',  ( 0.1999999999999567124, 2.500000000000000000, -4.083716857408426826 ) ) ;
#6654 = ADVANCED_FACE ( 'NONE', ( #23692 ), #93112, .T. ) ;
#6655 = CARTESIAN_POINT ( 'NONE',  ( 13.74999999999993427, 2.500000000000000000, 2.165063509461097713 ) ) ;
#6657 = EDGE_LOOP ( 'NONE', ( #46361, #6592 ) ) ;
#6656 = EDGE_CURVE ( 'NONE', #36089, #120893, #122353, .T. ) ;
#6658 = CARTESIAN_POINT ( 'NONE',  ( -7.500000000000013323, 12.50000000000000000, 5.022947341949748790 ) ) ;
#6659 = DIRECTION ( 'NONE',  ( 0.000000000000000000, 0.000000000000000000, 1.000000000000000000 ) ) ;
#6660 = ADVANCED_FACE ( 'NONE', ( #44621 ), #95153, .T. ) ;
#6661 = CARTESIAN_POINT ( 'NONE',  ( -3.300000000000027800, 2.500000000000000000, -4.330127018922201643 ) ) ;
#6662 = ADVANCED_FACE ( 'NONE', ( #45919 ), #73424, .T. ) ;
#6663 = ADVANCED_FACE ( 'NONE', ( #5328 ), #116072, .T. ) ;
#6664 = CARTESIAN_POINT ( 'NONE',  ( -0.4500000000000402012, 12.50000000000000000, 2.165063509461097713 ) ) ;
#6665 = CIRCLE ( 'NONE', #40162, 0.1000000000000002554 ) ;
#6666 = AXIS2_PLACEMENT_3D ( 'NONE', #51203, #89819, #91115 ) ;
#6667 = CARTESIAN_POINT ( 'NONE',  ( -6.900000000000019007, 2.500000000000000000, -4.676537180435978769 ) ) ;
#6668 = VERTEX_POINT ( 'NONE', #34165 ) ;
#6669 = AXIS2_PLACEMENT_3D ( 'NONE', #115390, #36875, #114769 ) ;
#6670 = VECTOR ( 'NONE', #83591, 1000.000000000000000 ) ;
#6671 = EDGE_LOOP ( 'NONE', ( #57556, #104047, #95892, #93036 ) ) ;
#6672 = CARTESIAN_POINT ( 'NONE',  ( -9.999999999999971578, 2.500000000000000000, -4.230127018922197557 ) ) ;
#6673 = EDGE_CURVE ( 'NONE', #58516, #125196, #3220, .T. ) ;
#6674 = AXIS2_PLACEMENT_3D ( 'NONE', #73547, #54547, #46506 ) ;
#6675 = ORIENTED_EDGE ( 'NONE', *, *, #110974, .T. ) ;
#6676 = DIRECTION ( 'NONE',  ( -0.000000000000000000, -1.000000000000000000, -0.000000000000000000 ) ) ;
#6677 = DIRECTION ( 'NONE',  ( 0.000000000000000000, 1.000000000000000000, 0.000000000000000000 ) ) ;
#6678 = EDGE_CURVE ( 'NONE', #126401, #27968, #86827, .T. ) ;
#6679 = ORIENTED_EDGE ( 'NONE', *, *, #126610, .T. ) ;
#6680 = CARTESIAN_POINT ( 'NONE',  ( 186.1250000000000000, -8.891194145520236347, -1.633285867636356693E-15 ) ) ;
#6681 = DIRECTION ( 'NONE',  ( 0.000000000000000000, 0.000000000000000000, 1.000000000000000000 ) ) ;
#6682 = CARTESIAN_POINT ( 'NONE',  ( -6.050000000000017586, 12.50000000000000000, 6.213873640053558134 ) ) ;
#6683 = DIRECTION ( 'NONE',  ( 0.000000000000000000, 1.000000000000000000, 0.000000000000000000 ) ) ;
#6684 = EDGE_LOOP ( 'NONE', ( #99168, #115384, #53763, #93789 ) ) ;
#6685 = DIRECTION ( 'NONE',  ( 0.000000000000000000, 1.000000000000000000, 0.000000000000000000 ) ) ;
#6686 = DIRECTION ( 'NONE',  ( 0.000000000000000000, 1.000000000000000000, 0.000000000000000000 ) ) ;
#6687 = ORIENTED_EDGE ( 'NONE', *, *, #75700, .F. ) ;
#6688 = CARTESIAN_POINT ( 'NONE',  ( 11.04999999999991189, 12.50000000000000000, 6.148780366869520897 ) ) ;
#6689 = CARTESIAN_POINT ( 'NONE',  ( 0.8499999999999545697, 2.500000000000000000, -1.572243186433550211 ) ) ;
#6690 = CARTESIAN_POINT ( 'NONE',  ( -3.550000000000028244, 12.50000000000000000, 2.576566944158910744 ) ) ;
#6691 = EDGE_LOOP ( 'NONE', ( #9714, #3701, #40850, #99585 ) ) ;
#6692 = DIRECTION ( 'NONE',  ( 0.000000000000000000, 0.000000000000000000, 1.000000000000000000 ) ) ;
#6693 = CONICAL_SURFACE ( 'NONE', #73621, 0.09999999999999999167, 0.003490658503988666988 ) ;
#6694 = CIRCLE ( 'NONE', #79895, 0.06509327318403743123 ) ;
#6695 = CIRCLE ( 'NONE', #111176, 0.06509327318403745899 ) ;
#6696 = VERTEX_POINT ( 'NONE', #114013 ) ;
#6697 = ADVANCED_FACE ( 'NONE', ( #45272 ), #24339, .T. ) ;
#6698 = CARTESIAN_POINT ( 'NONE',  ( -11.64999999999999680, 2.500000000000000000, -7.288010851410851032 ) ) ;
#6699 = DIRECTION ( 'NONE',  ( 0.000000000000000000, 0.000000000000000000, -1.000000000000000000 ) ) ;
#6700 = DIRECTION ( 'NONE',  ( 0.000000000000000000, 0.000000000000000000, 1.000000000000000000 ) ) ;
#6701 = EDGE_CURVE ( 'NONE', #72606, #76567, #70121, .T. ) ;
#6702 = VERTEX_POINT ( 'NONE', #84543 ) ;
#6704 = LINE ( 'NONE', #86583, #55195 ) ;
#6703 = VECTOR ( 'NONE', #112834, 1000.000000000000000 ) ;
#6705 = CONICAL_SURFACE ( 'NONE', #2517, 0.1000000000000000472, 0.003490658503988666988 ) ;
#6706 = EDGE_CURVE ( 'NONE', #69018, #40490, #124474, .T. ) ;
#6707 = AXIS2_PLACEMENT_3D ( 'NONE', #31458, #93591, #92291 ) ;
#6708 = AXIS2_PLACEMENT_3D ( 'NONE', #87914, #89228, #8080 ) ;
#6709 = ORIENTED_EDGE ( 'NONE', *, *, #56234, .F. ) ;
#6710 = AXIS2_PLACEMENT_3D ( 'NONE', #70573, #39852, #89568 ) ;
#6711 = EDGE_CURVE ( 'NONE', #43890, #93582, #55085, .T. ) ;
#6712 = ORIENTED_EDGE ( 'NONE', *, *, #44526, .F. ) ;
#6713 = CIRCLE ( 'NONE', #84107, 0.06509327318403745899 ) ;
#6714 = CARTESIAN_POINT ( 'NONE',  ( 7.499999999999925393, 2.500000000000000000, 4.922947341949748257 ) ) ;
#6715 = EDGE_CURVE ( 'NONE', #2794, #86533, #105715, .T. ) ;
#6716 = EDGE_CURVE ( 'NONE', #119339, #5078, #32573, .T. ) ;
#6717 = EDGE_LOOP ( 'NONE', ( #89397, #39942 ) ) ;
#6718 = DIRECTION ( 'NONE',  ( 0.000000000000000000, 0.000000000000000000, 1.000000000000000000 ) ) ;
#6719 = DIRECTION ( 'NONE',  ( 0.000000000000000000, 0.000000000000000000, 1.000000000000000000 ) ) ;
#6720 = ORIENTED_EDGE ( 'NONE', *, *, #43202, .T. ) ;
#6721 = EDGE_LOOP ( 'NONE', ( #80549, #97148, #114257, #33417 ) ) ;
#6722 = CARTESIAN_POINT ( 'NONE',  ( -8.150000000000014566, 2.500000000000000000, -6.248780366869521430 ) ) ;
#6723 = DIRECTION ( 'NONE',  ( 0.000000000000000000, 1.000000000000000000, 0.000000000000000000 ) ) ;
#6724 = EDGE_LOOP ( 'NONE', ( #99634, #100338 ) ) ;
#6725 = ADVANCED_FACE ( 'NONE', ( #56361 ), #108041, .T. ) ;
#6726 = FACE_OUTER_BOUND ( 'NONE', #110354, .T. ) ;
#6727 = DIRECTION ( 'NONE',  ( -4.274815082592931898E-19, -0.9999939076577903929, -0.003490651415223739937 ) ) ;
#6728 = CARTESIAN_POINT ( 'NONE',  ( 17.45652781226495875, -2.453230724138371954, -4.494708854621484839 ) ) ;
#6729 = LINE ( 'NONE', #35594, #113569 ) ;
#6730 = DIRECTION ( 'NONE',  ( 0.000000000000000000, -0.9999939076577903929, 0.003490651415223739937 ) ) ;
#6731 = DIRECTION ( 'NONE',  ( 0.000000000000000000, 0.000000000000000000, 1.000000000000000000 ) ) ;
#6732 = CIRCLE ( 'NONE', #23491, 0.09999999999999982514 ) ;
#6733 = ORIENTED_EDGE ( 'NONE', *, *, #60576, .F. ) ;
#6734 = EDGE_LOOP ( 'NONE', ( #14271, #52690, #121581, #9561 ) ) ;
#6735 = VERTEX_POINT ( 'NONE', #76658 ) ;
#6736 = ORIENTED_EDGE ( 'NONE', *, *, #112977, .F. ) ;
#6737 = CARTESIAN_POINT ( 'NONE',  ( -13.94999999999998863, 12.50000000000000000, 2.511473670974877503 ) ) ;
#6738 = CARTESIAN_POINT ( 'NONE',  ( -11.24999999999996447, 2.500000000000000000, -6.395190528383298378 ) ) ;
#6739 = DIRECTION ( 'NONE',  ( 0.000000000000000000, 0.000000000000000000, 1.000000000000000000 ) ) ;
#6740 = ORIENTED_EDGE ( 'NONE', *, *, #32620, .F. ) ;
#6741 = FACE_BOUND ( 'NONE', #29353, .T. ) ;
#6742 = EDGE_CURVE ( 'NONE', #118052, #83264, #126644, .T. ) ;
#6743 = AXIS2_PLACEMENT_3D ( 'NONE', #28481, #89332, #97847 ) ;
#6744 = LINE ( 'NONE', #104338, #91897 ) ;
#6745 = DIRECTION ( 'NONE',  ( 0.000000000000000000, 1.000000000000000000, 0.000000000000000000 ) ) ;
#6746 = AXIS2_PLACEMENT_3D ( 'NONE', #86667, #47406, #28409 ) ;
#6748 = CARTESIAN_POINT ( 'NONE',  ( 2.099999999999948574, 2.500000000000000000, 3.637306695894644726 ) ) ;
#6747 = AXIS2_PLACEMENT_3D ( 'NONE', #1468, #9367, #99693 ) ;
#6749 = AXIS2_PLACEMENT_3D ( 'NONE', #120049, #111504, #80120 ) ;
#6750 = CARTESIAN_POINT ( 'NONE',  ( -7.300000000000016698, 2.500000000000000000, -4.676537180435978769 ) ) ;
#6751 = CARTESIAN_POINT ( 'NONE',  ( 10.59999999999990905, 12.50000000000000000, 4.741630453620009789 ) ) ;
#6752 = PLANE ( 'NONE',  #104022 ) ;
#6753 = DIRECTION ( 'NONE',  ( 0.000000000000000000, 1.000000000000000000, 0.000000000000000000 ) ) ;
#6754 = FACE_OUTER_BOUND ( 'NONE', #26727, .T. ) ;
#6755 = CARTESIAN_POINT ( 'NONE',  ( -0.4000000000000331624, 12.50000000000000000, 0.000000000000000000 ) ) ;
#6756 = CIRCLE ( 'NONE', #107029, 0.06509327318403745899 ) ;
#6757 = LINE ( 'NONE', #93895, #20893 ) ;
#6758 = AXIS2_PLACEMENT_3D ( 'NONE', #20441, #80002, #30280 ) ;
#6759 = VERTEX_POINT ( 'NONE', #38018 ) ;
#6760 = EDGE_LOOP ( 'NONE', ( #22469, #86308, #59191, #98544 ) ) ;
#6761 = EDGE_CURVE ( 'NONE', #83109, #935, #59762, .T. ) ;
#6762 = VERTEX_POINT ( 'NONE', #87110 ) ;
#6764 = VERTEX_POINT ( 'NONE', #116567 ) ;
#6763 = CONICAL_SURFACE ( 'NONE', #52757, 0.09999999999999982514, 0.003490658503988666988 ) ;
#6765 = AXIS2_PLACEMENT_3D ( 'NONE', #70104, #41941, #79918 ) ;
#6766 = AXIS2_PLACEMENT_3D ( 'NONE', #77311, #48497, #7914 ) ;
#6767 = CARTESIAN_POINT ( 'NONE',  ( 3.949999999999941558, 12.50000000000000000, -6.148780366869526226 ) ) ;
#6768 = DIRECTION ( 'NONE',  ( -4.274815082592931898E-19, -0.9999939076577903929, -0.003490651415223739937 ) ) ;
#6770 = VERTEX_POINT ( 'NONE', #8534 ) ;
#6769 = ORIENTED_EDGE ( 'NONE', *, *, #44076, .F. ) ;
#6771 = ORIENTED_EDGE ( 'NONE', *, *, #95816, .T. ) ;
#6772 = CIRCLE ( 'NONE', #123863, 0.06509327318403745899 ) ;
#6773 = CARTESIAN_POINT ( 'NONE',  ( 0.4499999999999552136, 2.500000000000000000, 6.395190528383296602 ) ) ;
#6774 = CIRCLE ( 'NONE', #86205, 0.1000000000000002554 ) ;
#6775 = CARTESIAN_POINT ( 'NONE',  ( 8.512291507278442637, -1.500000000000000222, 9.502944100741331113 ) ) ;
#6776 = DIRECTION ( 'NONE',  ( 0.000000000000000000, 0.000000000000000000, 1.000000000000000000 ) ) ;
#6777 = CARTESIAN_POINT ( 'NONE',  ( -3.100000000000028511, 12.50000000000000000, 0.2813168883297362810 ) ) ;
#6778 = CARTESIAN_POINT ( 'NONE',  ( 187.1562500006828316, 8.891194145520236347, 5.444286225454521982E-16 ) ) ;
#6779 = EDGE_CURVE ( 'NONE', #108500, #69856, #36771, .T. ) ;
#6780 = ORIENTED_EDGE ( 'NONE', *, *, #36732, .T. ) ;
#6781 = EDGE_LOOP ( 'NONE', ( #5148, #9228, #101139, #91964 ) ) ;
#6782 = ORIENTED_EDGE ( 'NONE', *, *, #29320, .F. ) ;
#6783 = ORIENTED_EDGE ( 'NONE', *, *, #11565, .T. ) ;
#6784 = CARTESIAN_POINT ( 'NONE',  ( 184.7500000000000000, 9.429780353434619030E-16, -7.700000000000000178 ) ) ;
#6785 = AXIS2_PLACEMENT_3D ( 'NONE', #22965, #49860, #101523 ) ;
#6786 = ORIENTED_EDGE ( 'NONE', *, *, #30374, .T. ) ;
#6787 = ORIENTED_EDGE ( 'NONE', *, *, #56026, .F. ) ;
#6788 = FACE_OUTER_BOUND ( 'NONE', #83110, .T. ) ;
#6789 = FACE_OUTER_BOUND ( 'NONE', #78288, .T. ) ;
#6790 = DIRECTION ( 'NONE',  ( 0.000000000000000000, 0.000000000000000000, 1.000000000000000000 ) ) ;
#6792 = FACE_OUTER_BOUND ( 'NONE', #103509, .T. ) ;
#6791 = AXIS2_PLACEMENT_3D ( 'NONE', #18017, #45568, #105768 ) ;
#6793 = VECTOR ( 'NONE', #72656, 1000.000000000000000 ) ;
#6794 = AXIS2_PLACEMENT_3D ( 'NONE', #45812, #85714, #6479 ) ;
#6795 = DIRECTION ( 'NONE',  ( 0.000000000000000000, 1.000000000000000000, 0.000000000000000000 ) ) ;
#6796 = ORIENTED_EDGE ( 'NONE', *, *, #23589, .F. ) ;
#6797 = LINE ( 'NONE', #15341, #90817 ) ;
#6798 = AXIS2_PLACEMENT_3D ( 'NONE', #1354, #22946, #12462 ) ;
#6800 = EDGE_LOOP ( 'NONE', ( #110603, #78866, #89663, #95867 ) ) ;
#6799 = AXIS2_PLACEMENT_3D ( 'NONE', #13613, #53559, #3807 ) ;
#6801 = CARTESIAN_POINT ( 'NONE',  ( 186.2500000000000000, 9.429780353434619030E-16, -7.700000000000000178 ) ) ;
#6803 = EDGE_CURVE ( 'NONE', #6219, #66296, #53487, .T. ) ;
#6802 = AXIS2_PLACEMENT_3D ( 'NONE', #33122, #84121, #124053 ) ;
#6804 = ORIENTED_EDGE ( 'NONE', *, *, #8550, .T. ) ;
#6805 = CARTESIAN_POINT ( 'NONE',  ( 9.349999999999916156, 12.50000000000000000, -1.818653347947326138 ) ) ;
#6806 = LINE ( 'NONE', #86686, #42820 ) ;
#6807 = CONICAL_SURFACE ( 'NONE', #94654, 0.09999999999999982514, 0.003490658503988666988 ) ;
#6808 = EDGE_LOOP ( 'NONE', ( #333, #42894 ) ) ;
#6809 = AXIS2_PLACEMENT_3D ( 'NONE', #62059, #121594, #82988 ) ;
#6810 = CARTESIAN_POINT ( 'NONE',  ( 3.549999999999944755, 12.50000000000000000, -2.511473670974877948 ) ) ;
#6811 = LINE ( 'NONE', #77514, #12185 ) ;
#6812 = EDGE_LOOP ( 'NONE', ( #16203, #103969, #101660, #63309 ) ) ;
#6813 = ADVANCED_FACE ( 'NONE', ( #118503 ), #70203, .T. ) ;
#6814 = DIRECTION ( 'NONE',  ( -0.000000000000000000, 1.000000000000000000, -0.000000000000000000 ) ) ;
#6815 = EDGE_LOOP ( 'NONE', ( #71189, #21105 ) ) ;
#6816 = EDGE_CURVE ( 'NONE', #100735, #2439, #68760, .T. ) ;
#6818 = ORIENTED_EDGE ( 'NONE', *, *, #76349, .T. ) ;
#6817 = ADVANCED_FACE ( 'NONE', ( #77939 ), #39893, .T. ) ;
#6819 = CARTESIAN_POINT ( 'NONE',  ( -6.249999999999984901, 12.50000000000000000, -2.165063509461101710 ) ) ;
#6820 = CARTESIAN_POINT ( 'NONE',  ( 6.249999999999930722, 12.50000000000000000, 1.537336459617582918 ) ) ;
#6821 = EDGE_CURVE ( 'NONE', #73823, #69623, #40982, .T. ) ;
#6822 = CARTESIAN_POINT ( 'NONE',  ( 185.4635416670080872, -4.367472073101519747, 7.564683531249999149 ) ) ;
#6823 = ADVANCED_FACE ( 'NONE', ( #17047 ), #56998, .T. ) ;
#6824 = DIRECTION ( 'NONE',  ( 0.000000000000000000, 0.000000000000000000, 1.000000000000000000 ) ) ;
#6825 = DIRECTION ( 'NONE',  ( 0.000000000000000000, 0.000000000000000000, 1.000000000000000000 ) ) ;
#6826 = ADVANCED_FACE ( 'NONE', ( #127055 ), #72271, .T. ) ;
#6827 = FACE_OUTER_BOUND ( 'NONE', #43561, .T. ) ;
#6828 = EDGE_CURVE ( 'NONE', #79421, #11460, #57692, .T. ) ;
#6829 = EDGE_CURVE ( 'NONE', #37333, #92919, #114110, .T. ) ;
#6830 = CIRCLE ( 'NONE', #80021, 0.1000000000000002554 ) ;
#6831 = EDGE_LOOP ( 'NONE', ( #4269, #57537, #50905, #35957 ) ) ;
#6832 = ADVANCED_FACE ( 'NONE', ( #71328 ), #111243, .T. ) ;
#6833 = CARTESIAN_POINT ( 'NONE',  ( 11.69999999999990514, 12.50000000000000000, 0.06509327318403515528 ) ) ;
#6834 = EDGE_CURVE ( 'NONE', #56267, #118565, #20039, .T. ) ;
#6835 = VERTEX_POINT ( 'NONE', #21605 ) ;
#6836 = CARTESIAN_POINT ( 'NONE',  ( 2.699999999999946443, 2.500000000000000000, 0.3464101615137735735 ) ) ;
#6837 = DIRECTION ( 'NONE',  ( 0.000000000000000000, 1.000000000000000000, 0.000000000000000000 ) ) ;
#6838 = CARTESIAN_POINT ( 'NONE',  ( 9.999999999999948486, 12.50000000000000000, -4.330127018922201643 ) ) ;
#6839 = LINE ( 'NONE', #78205, #16714 ) ;
#6841 = EDGE_CURVE ( 'NONE', #36786, #114224, #43043, .T. ) ;
#6840 = AXIS2_PLACEMENT_3D ( 'NONE', #100128, #60844, #10447 ) ;
#6843 = AXIS2_PLACEMENT_3D ( 'NONE', #68652, #9735, #60148 ) ;
#6842 = DIRECTION ( 'NONE',  ( 0.000000000000000000, 0.000000000000000000, 1.000000000000000000 ) ) ;
#6844 = ORIENTED_EDGE ( 'NONE', *, *, #79714, .T. ) ;
#6845 = AXIS2_PLACEMENT_3D ( 'NONE', #122552, #32895, #17722 ) ;
#6846 = AXIS2_PLACEMENT_3D ( 'NONE', #80619, #68850, #89780 ) ;
#6847 = FACE_OUTER_BOUND ( 'NONE', #65928, .T. ) ;
#6848 = CARTESIAN_POINT ( 'NONE',  ( 12.69999999999989804, 2.500000000000000000, 0.3464101615137735735 ) ) ;
#6849 = AXIS2_PLACEMENT_3D ( 'NONE', #100121, #60215, #38644 ) ;
#6850 = ORIENTED_EDGE ( 'NONE', *, *, #79145, .F. ) ;
#6851 = DIRECTION ( 'NONE',  ( -4.274815082592931898E-19, -0.9999939076577903929, -0.003490651415223739937 ) ) ;
#6852 = ORIENTED_EDGE ( 'NONE', *, *, #125936, .T. ) ;
#6853 = AXIS2_PLACEMENT_3D ( 'NONE', #91508, #102607, #23398 ) ;
#6855 = ORIENTED_EDGE ( 'NONE', *, *, #65579, .T. ) ;
#6854 = AXIS2_PLACEMENT_3D ( 'NONE', #39231, #123387, #33723 ) ;
#6856 = CARTESIAN_POINT ( 'NONE',  ( -7.100000000000017408, 2.500000000000000000, -5.022947341949754119 ) ) ;
#6858 = ORIENTED_EDGE ( 'NONE', *, *, #51244, .T. ) ;
#6857 = AXIS2_PLACEMENT_3D ( 'NONE', #50246, #109135, #69215 ) ;
#6859 = CARTESIAN_POINT ( 'NONE',  ( -8.950000000000008171, 2.500000000000000000, 1.718653347947321386 ) ) ;
#6860 = DIRECTION ( 'NONE',  ( 0.000000000000000000, 0.000000000000000000, 1.000000000000000000 ) ) ;
#6861 = CARTESIAN_POINT ( 'NONE',  ( -8.150000000000012790, 2.500000000000000000, 2.611473670974873151 ) ) ;
#6862 = VERTEX_POINT ( 'NONE', #89696 ) ;
#6863 = FACE_BOUND ( 'NONE', #34324, .T. ) ;
#6864 = AXIS2_PLACEMENT_3D ( 'NONE', #98688, #106585, #9025 ) ;
#6866 = EDGE_LOOP ( 'NONE', ( #69901, #116492, #50831, #43463 ) ) ;
#6865 = DIRECTION ( 'NONE',  ( 0.000000000000000000, 0.000000000000000000, -1.000000000000000000 ) ) ;
#6867 = FACE_OUTER_BOUND ( 'NONE', #41202, .T. ) ;
#6868 = DIRECTION ( 'NONE',  ( 0.4999999999999471534, 0.000000000000000000, -0.8660254037844692387 ) ) ;
#6869 = VERTEX_POINT ( 'NONE', #30151 ) ;
#6870 = ADVANCED_FACE ( 'NONE', ( #61539 ), #59621, .T. ) ;
#6871 = ORIENTED_EDGE ( 'NONE', *, *, #490, .F. ) ;
#6872 = EDGE_CURVE ( 'NONE', #125434, #120460, #11704, .T. ) ;
#6873 = EDGE_LOOP ( 'NONE', ( #115402, #58640 ) ) ;
#6874 = DIRECTION ( 'NONE',  ( 0.000000000000000000, 0.000000000000000000, -1.000000000000000000 ) ) ;
#6875 = DIRECTION ( 'NONE',  ( 0.000000000000000000, 0.000000000000000000, 1.000000000000000000 ) ) ;
#6877 = CARTESIAN_POINT ( 'NONE',  ( 0.4499999999999569344, 12.50000000000000000, 2.230156782645134950 ) ) ;
#6876 = CONICAL_SURFACE ( 'NONE', #15201, 0.09999999999999982514, 0.003490658503988666988 ) ;
#6878 = AXIS2_PLACEMENT_3D ( 'NONE', #68679, #27450, #67358 ) ;
#6879 = FACE_BOUND ( 'NONE', #13108, .T. ) ;
#6880 = ORIENTED_EDGE ( 'NONE', *, *, #48913, .F. ) ;
#6881 = DIRECTION ( 'NONE',  ( -0.000000000000000000, -1.000000000000000000, -0.000000000000000000 ) ) ;
#6882 = DIRECTION ( 'NONE',  ( 0.000000000000000000, 0.000000000000000000, 1.000000000000000000 ) ) ;
#6883 = EDGE_CURVE ( 'NONE', #54857, #102205, #70700, .T. ) ;
#6885 = LINE ( 'NONE', #76308, #90973 ) ;
#6884 = CONICAL_SURFACE ( 'NONE', #13152, 0.09999999999999982514, 0.003490658503988666988 ) ;
#6886 = VECTOR ( 'NONE', #112552, 1000.000000000000000 ) ;
#6887 = VECTOR ( 'NONE', #87608, 1000.000000000000000 ) ;
#6889 = CIRCLE ( 'NONE', #25698, 0.06509327318403745899 ) ;
#6888 = CARTESIAN_POINT ( 'NONE',  ( -4.400000000000025224, 2.500000000000000000, 0.4464101615137735513 ) ) ;
#6890 = DIRECTION ( 'NONE',  ( 0.000000000000000000, -0.000000000000000000, 1.000000000000000000 ) ) ;
#6891 = CARTESIAN_POINT ( 'NONE',  ( 1.649999999999950617, 12.50000000000000000, -2.230156782645139391 ) ) ;
#6892 = DIRECTION ( 'NONE',  ( 0.000000000000000000, 0.000000000000000000, -1.000000000000000000 ) ) ;
#6893 = VECTOR ( 'NONE', #42296, 1000.000000000000000 ) ;
#6894 = CONICAL_SURFACE ( 'NONE', #50847, 8.699999999999999289, 0.08726646259971666819 ) ;
#6895 = ORIENTED_EDGE ( 'NONE', *, *, #17643, .T. ) ;
#6896 = ORIENTED_EDGE ( 'NONE', *, *, #95147, .T. ) ;
#6897 = EDGE_LOOP ( 'NONE', ( #121186, #123526 ) ) ;
#6898 = ORIENTED_EDGE ( 'NONE', *, *, #68787, .T. ) ;
#6900 = ORIENTED_EDGE ( 'NONE', *, *, #100584, .T. ) ;
#6899 = AXIS2_PLACEMENT_3D ( 'NONE', #105166, #55433, #115624 ) ;
#6901 = DIRECTION ( 'NONE',  ( -0.000000000000000000, -1.000000000000000000, -0.000000000000000000 ) ) ;
#6902 = AXIS2_PLACEMENT_3D ( 'NONE', #25668, #47262, #48541 ) ;
#6903 = CARTESIAN_POINT ( 'NONE',  ( 1.249999999999954259, 2.500000000000000000, -7.088010851410853519 ) ) ;
#6904 = ORIENTED_EDGE ( 'NONE', *, *, #29176, .T. ) ;
#6905 = FACE_BOUND ( 'NONE', #94056, .T. ) ;
#6906 = CONICAL_SURFACE ( 'NONE', #107282, 0.1000000000000002554, 0.003490658503988666988 ) ;
#6907 = DIRECTION ( 'NONE',  ( 0.000000000000000000, 1.000000000000000000, 0.000000000000000000 ) ) ;
#6908 = LINE ( 'NONE', #16729, #999 ) ;
#6909 = PLANE ( 'NONE',  #103840 ) ;
#6910 = CARTESIAN_POINT ( 'NONE',  ( -3.150000000000029665, 2.500000000000000000, 6.941600689897073018 ) ) ;
#6911 = DIRECTION ( 'NONE',  ( 0.000000000000000000, -0.9999939076577903929, 0.003490651415223739937 ) ) ;
#6912 = ORIENTED_EDGE ( 'NONE', *, *, #22092, .T. ) ;
#6913 = PLANE ( 'NONE',  #82755 ) ;
#6914 = VECTOR ( 'NONE', #60987, 1000.000000000000000 ) ;
#6915 = ORIENTED_EDGE ( 'NONE', *, *, #48209, .T. ) ;
#6916 = ORIENTED_EDGE ( 'NONE', *, *, #50030, .F. ) ;
#6917 = ORIENTED_EDGE ( 'NONE', *, *, #34342, .T. ) ;
#6918 = CARTESIAN_POINT ( 'NONE',  ( -8.300000000000009592, 12.50000000000000000, 4.330127018922196314 ) ) ;
#6919 = FACE_OUTER_BOUND ( 'NONE', #74764, .T. ) ;
#6920 = PLANE ( 'NONE',  #101163 ) ;
#6921 = ORIENTED_EDGE ( 'NONE', *, *, #37486, .F. ) ;
#6922 = CARTESIAN_POINT ( 'NONE',  ( 10.04522989421396417, 2.499999999999999556, -8.164691043410849502 ) ) ;
#6923 = AXIS2_PLACEMENT_3D ( 'NONE', #128112, #37794, #58727 ) ;
#6924 = AXIS2_PLACEMENT_3D ( 'NONE', #83408, #12698, #102399 ) ;
#6926 = DIRECTION ( 'NONE',  ( -4.274815082592931898E-19, -0.9999939076577903929, -0.003490651415223739937 ) ) ;
#6925 = VECTOR ( 'NONE', #90765, 1000.000000000000000 ) ;
#6927 = CARTESIAN_POINT ( 'NONE',  ( -4.150000000000024336, 2.500000000000000000, 2.165063509461097713 ) ) ;
#6928 = CARTESIAN_POINT ( 'NONE',  ( 187.1510416670080303, 4.367472073101518859, -7.564683531249999149 ) ) ;
#6929 = DIRECTION ( 'NONE',  ( -0.000000000000000000, 1.000000000000000000, -0.000000000000000000 ) ) ;
#6930 = CARTESIAN_POINT ( 'NONE',  ( -9.150000000000009237, 12.50000000000000000, 2.857883832488649301 ) ) ;
#6931 = ADVANCED_FACE ( 'NONE', ( #92260 ), #2583, .T. ) ;
#6932 = CARTESIAN_POINT ( 'NONE',  ( 8.749999999999923617, 2.500000000000000000, 1.472243186433545459 ) ) ;
#6933 = EDGE_CURVE ( 'NONE', #95501, #76430, #41262, .T. ) ;
#6934 = CIRCLE ( 'NONE', #42587, 0.06509327318403745899 ) ;
#6935 = ORIENTED_EDGE ( 'NONE', *, *, #8471, .T. ) ;
#6936 = LINE ( 'NONE', #127394, #88099 ) ;
#6937 = ORIENTED_EDGE ( 'NONE', *, *, #112797, .T. ) ;
#6938 = CONICAL_SURFACE ( 'NONE', #4895, 0.1000000000000002554, 0.003490658503988666988 ) ;
#6939 = EDGE_LOOP ( 'NONE', ( #77915, #97773, #93984, #54452 ) ) ;
#6940 = DIRECTION ( 'NONE',  ( 0.000000000000000000, 0.000000000000000000, 1.000000000000000000 ) ) ;
#6941 = DIRECTION ( 'NONE',  ( 0.000000000000000000, 0.000000000000000000, -1.000000000000000000 ) ) ;
#6943 = ADVANCED_FACE ( 'NONE', ( #60877 ), #30519, .T. ) ;
#6942 = PLANE ( 'NONE',  #119892 ) ;
#6944 = ORIENTED_EDGE ( 'NONE', *, *, #115060, .F. ) ;
#6945 = ORIENTED_EDGE ( 'NONE', *, *, #50269, .T. ) ;
#6946 = LINE ( 'NONE', #56695, #1612 ) ;
#6948 = CIRCLE ( 'NONE', #113595, 0.06509327318403745899 ) ;
#6947 = FACE_OUTER_BOUND ( 'NONE', #4221, .T. ) ;
#6949 = AXIS2_PLACEMENT_3D ( 'NONE', #94567, #105697, #55303 ) ;
#6950 = AXIS2_PLACEMENT_3D ( 'NONE', #10964, #12899, #22129 ) ;
#6951 = CARTESIAN_POINT ( 'NONE',  ( 8.149999999999920419, 2.500000000000000000, -1.818653347947325916 ) ) ;
#6952 = ORIENTED_EDGE ( 'NONE', *, *, #39830, .F. ) ;
#6953 = ORIENTED_EDGE ( 'NONE', *, *, #99648, .T. ) ;
#6954 = CARTESIAN_POINT ( 'NONE',  ( -5.800000000000018474, 2.500000000000000000, 4.430127018922196847 ) ) ;
#6955 = AXIS2_PLACEMENT_3D ( 'NONE', #116869, #107052, #48154 ) ;
#6956 = EDGE_LOOP ( 'NONE', ( #44316, #11865, #36966, #39751 ) ) ;
#6957 = DIRECTION ( 'NONE',  ( 0.000000000000000000, 0.000000000000000000, -1.000000000000000000 ) ) ;
#6958 = FACE_OUTER_BOUND ( 'NONE', #111752, .T. ) ;
#6959 = ORIENTED_EDGE ( 'NONE', *, *, #4945, .T. ) ;
#6960 = DIRECTION ( 'NONE',  ( 0.000000000000000000, 1.000000000000000000, 0.000000000000000000 ) ) ;
#6961 = EDGE_CURVE ( 'NONE', #9598, #2580, #128728, .T. ) ;
#6962 = CARTESIAN_POINT ( 'NONE',  ( -9.200000000000006395, 2.500000000000000000, -2.385244779468109755E-15 ) ) ;
#6963 = CARTESIAN_POINT ( 'NONE',  ( 5.399999999999936406, 2.500000000000000000, -3.537306695894649966 ) ) ;
#6964 = DIRECTION ( 'NONE',  ( -4.274815082592931898E-19, -0.9999939076577903929, -0.003490651415223739937 ) ) ;
#6965 = EDGE_LOOP ( 'NONE', ( #83440, #68214, #37688, #13118 ) ) ;
#6966 = EDGE_CURVE ( 'NONE', #71302, #76450, #20, .T. ) ;
#6967 = DIRECTION ( 'NONE',  ( 0.000000000000000000, 1.000000000000000000, 0.000000000000000000 ) ) ;
#6968 = CARTESIAN_POINT ( 'NONE',  ( -3.750000000000027978, 12.50000000000000000, 7.188010851410848723 ) ) ;
#6969 = ORIENTED_EDGE ( 'NONE', *, *, #69043, .T. ) ;
#6970 = ORIENTED_EDGE ( 'NONE', *, *, #29345, .F. ) ;
#6971 = EDGE_CURVE ( 'NONE', #37002, #122488, #84864, .T. ) ;
#6972 = CIRCLE ( 'NONE', #19518, 0.06509327318403745899 ) ;
#6973 = EDGE_CURVE ( 'NONE', #15557, #33416, #50411, .T. ) ;
#6974 = CARTESIAN_POINT ( 'NONE',  ( 184.5885416670080872, -6.551208109652273848, -3.782341765625003571 ) ) ;
#6975 = DIRECTION ( 'NONE',  ( 0.000000000000000000, 0.000000000000000000, 1.000000000000000000 ) ) ;
#6976 = DIRECTION ( 'NONE',  ( -4.274815082592931898E-19, -0.9999939076577903929, -0.003490651415223739937 ) ) ;
#6977 = EDGE_CURVE ( 'NONE', #78871, #72078, #47228, .T. ) ;
#6978 = LINE ( 'NONE', #18754, #77216 ) ;
#6979 = EDGE_CURVE ( 'NONE', #62883, #1523, #81170, .T. ) ;
#6980 = PLANE ( 'NONE',  #105485 ) ;
#6981 = DIRECTION ( 'NONE',  ( 0.000000000000000000, 1.000000000000000000, 0.000000000000000000 ) ) ;
#6982 = AXIS2_PLACEMENT_3D ( 'NONE', #65796, #14740, #5575 ) ;
#6983 = CIRCLE ( 'NONE', #86415, 0.5000000000000000000 ) ;
#6984 = DIRECTION ( 'NONE',  ( 0.000000000000000000, 1.000000000000000000, 0.000000000000000000 ) ) ;
#6985 = CONICAL_SURFACE ( 'NONE', #78126, 0.09999999999999999167, 0.003490658503988666988 ) ;
#6986 = CARTESIAN_POINT ( 'NONE',  ( 2.499999999999945377, 12.50000000000000000, 5.022947341949748790 ) ) ;
#6988 = CONICAL_SURFACE ( 'NONE', #92694, 0.1000000000000002554, 0.003490658503988666988 ) ;
#6987 = DIRECTION ( 'NONE',  ( -0.000000000000000000, 1.000000000000000000, -0.000000000000000000 ) ) ;
#6989 = EDGE_CURVE ( 'NONE', #34015, #116265, #63944, .T. ) ;
#6990 = AXIS2_PLACEMENT_3D ( 'NONE', #129231, #17953, #78180 ) ;
#6991 = ADVANCED_FACE ( 'NONE', ( #1309 ), #124582, .T. ) ;
#6992 = LINE ( 'NONE', #87491, #73125 ) ;
#6993 = VECTOR ( 'NONE', #52426, 1000.000000000000000 ) ;
#6994 = AXIS2_PLACEMENT_3D ( 'NONE', #52120, #87921, #80062 ) ;
#6995 = VECTOR ( 'NONE', #108172, 1000.000000000000000 ) ;
#6996 = ADVANCED_FACE ( 'NONE', ( #25441 ), #102718, .F. ) ;
#6997 = EDGE_LOOP ( 'NONE', ( #55547, #1217 ) ) ;
#6998 = VECTOR ( 'NONE', #39047, 1000.000000000000000 ) ;
#6999 = FACE_OUTER_BOUND ( 'NONE', #81090, .T. ) ;
#7000 = CONICAL_SURFACE ( 'NONE', #15411, 0.09999999999999982514, 0.003490658503988666988 ) ;
#7001 = VERTEX_POINT ( 'NONE', #34004 ) ;
#7002 = ADVANCED_FACE ( 'NONE', ( #53002 ), #28446, .T. ) ;
#7003 = DIRECTION ( 'NONE',  ( 0.000000000000000000, 0.000000000000000000, -1.000000000000000000 ) ) ;
#7004 = DIRECTION ( 'NONE',  ( 0.000000000000000000, 1.000000000000000000, 0.000000000000000000 ) ) ;
#7005 = DIRECTION ( 'NONE',  ( 0.000000000000000000, -0.9999939076577903929, 0.003490651415223739937 ) ) ;
#7006 = EDGE_CURVE ( 'NONE', #91287, #2089, #34667, .T. ) ;
#7007 = ORIENTED_EDGE ( 'NONE', *, *, #112535, .T. ) ;
#7008 = LINE ( 'NONE', #54828, #96796 ) ;
#7009 = DIRECTION ( 'NONE',  ( -0.000000000000000000, -1.000000000000000000, -0.000000000000000000 ) ) ;
#7011 = ORIENTED_EDGE ( 'NONE', *, *, #71151, .T. ) ;
#7010 = CARTESIAN_POINT ( 'NONE',  ( 97.50000000000000000, -1.500000000000000222, -1.322875655532295136 ) ) ;
#7013 = DIRECTION ( 'NONE',  ( -0.000000000000000000, 1.000000000000000000, -0.000000000000000000 ) ) ;
#7012 = AXIS2_PLACEMENT_3D ( 'NONE', #36705, #47807, #16373 ) ;
#7014 = ORIENTED_EDGE ( 'NONE', *, *, #113076, .F. ) ;
#7015 = EDGE_LOOP ( 'NONE', ( #103845, #126622 ) ) ;
#7016 = EDGE_LOOP ( 'NONE', ( #15025, #40705, #49606, #68569 ) ) ;
#7017 = VERTEX_POINT ( 'NONE', #23525 ) ;
#7018 = CARTESIAN_POINT ( 'NONE',  ( -8.100000000000013856, 12.50000000000000000, -4.676537180435977881 ) ) ;
#7020 = DIRECTION ( 'NONE',  ( 0.000000000000000000, 0.000000000000000000, 1.000000000000000000 ) ) ;
#7019 = VECTOR ( 'NONE', #63235, 1000.000000000000000 ) ;
#7021 = DIRECTION ( 'NONE',  ( 0.000000000000000000, -0.000000000000000000, 1.000000000000000000 ) ) ;
#7022 = AXIS2_PLACEMENT_3D ( 'NONE', #52480, #119947, #102859 ) ;
#7023 = LINE ( 'NONE', #128114, #120935 ) ;
#7024 = AXIS2_PLACEMENT_3D ( 'NONE', #76288, #113636, #36384 ) ;
#7025 = ORIENTED_EDGE ( 'NONE', *, *, #61176, .T. ) ;
#7026 = DIRECTION ( 'NONE',  ( 0.000000000000000000, 1.000000000000000000, 0.000000000000000000 ) ) ;
#7027 = ORIENTED_EDGE ( 'NONE', *, *, #19449, .F. ) ;
#7028 = CARTESIAN_POINT ( 'NONE',  ( 12.49999999999990052, 2.500000000000000000, 0.6928203230275494784 ) ) ;
#7029 = CARTESIAN_POINT ( 'NONE',  ( -2.100000000000033396, 2.500000000000000000, -0.7928203230275543412 ) ) ;
#7030 = DIRECTION ( 'NONE',  ( -4.274815082592931898E-19, -0.9999939076577903929, -0.003490651415223739937 ) ) ;
#7031 = DIRECTION ( 'NONE',  ( -0.000000000000000000, -1.000000000000000000, -0.000000000000000000 ) ) ;
#7032 = VECTOR ( 'NONE', #71144, 1000.000000000000000 ) ;
#7033 = VECTOR ( 'NONE', #9580, 1000.000000000000000 ) ;
#7034 = AXIS2_PLACEMENT_3D ( 'NONE', #40964, #79578, #120781 ) ;
#7035 = ORIENTED_EDGE ( 'NONE', *, *, #19450, .F. ) ;
#7036 = VECTOR ( 'NONE', #81573, 1000.000000000000000 ) ;
#7037 = EDGE_CURVE ( 'NONE', #19146, #30332, #53640, .T. ) ;
#7038 = VERTEX_POINT ( 'NONE', #92933 ) ;
#7039 = VERTEX_POINT ( 'NONE', #124960 ) ;
#7040 = EDGE_CURVE ( 'NONE', #53498, #128103, #22197, .T. ) ;
#7041 = ORIENTED_EDGE ( 'NONE', *, *, #55143, .F. ) ;
#7042 = DIRECTION ( 'NONE',  ( -0.000000000000000000, -1.000000000000000000, -0.000000000000000000 ) ) ;
#7043 = CARTESIAN_POINT ( 'NONE',  ( 76.44836599003085098, 3.583082429763411625, 6.086789565880034836 ) ) ;
#7044 = DIRECTION ( 'NONE',  ( 0.000000000000000000, 0.000000000000000000, 1.000000000000000000 ) ) ;
#7045 = FACE_BOUND ( 'NONE', #106291, .T. ) ;
#7046 = AXIS2_PLACEMENT_3D ( 'NONE', #89387, #20008, #129334 ) ;
#7047 = DIRECTION ( 'NONE',  ( -0.000000000000000000, 1.000000000000000000, -0.000000000000000000 ) ) ;
#7048 = CARTESIAN_POINT ( 'NONE',  ( 9.149999999999916866, 12.50000000000000000, 7.188010851410848723 ) ) ;
#7049 = DIRECTION ( 'NONE',  ( 0.000000000000000000, 0.000000000000000000, -1.000000000000000000 ) ) ;
#7050 = DIRECTION ( 'NONE',  ( 0.000000000000000000, 0.000000000000000000, 1.000000000000000000 ) ) ;
#7051 = CIRCLE ( 'NONE', #48944, 0.1000000000000002554 ) ;
#7052 = AXIS2_PLACEMENT_3D ( 'NONE', #51936, #2170, #7893 ) ;
#7053 = CIRCLE ( 'NONE', #4910, 0.06509327318403745899 ) ;
#7054 = CARTESIAN_POINT ( 'NONE',  ( 184.2552083336747444, 6.551208109652275624, -3.782341765624998686 ) ) ;
#7055 = DIRECTION ( 'NONE',  ( 0.000000000000000000, 1.000000000000000000, 0.000000000000000000 ) ) ;
#7056 = CIRCLE ( 'NONE', #94909, 0.06509327318403745899 ) ;
#7057 = DIRECTION ( 'NONE',  ( 0.000000000000000000, 0.000000000000000000, 1.000000000000000000 ) ) ;
#7058 = AXIS2_PLACEMENT_3D ( 'NONE', #36230, #73549, #64384 ) ;
#7059 = DIRECTION ( 'NONE',  ( 0.000000000000000000, 0.000000000000000000, -1.000000000000000000 ) ) ;
#7060 = ORIENTED_EDGE ( 'NONE', *, *, #102567, .T. ) ;
#7061 = EDGE_LOOP ( 'NONE', ( #21290, #56050 ) ) ;
#7062 = ORIENTED_EDGE ( 'NONE', *, *, #2127, .T. ) ;
#7063 = ORIENTED_EDGE ( 'NONE', *, *, #85580, .F. ) ;
#7064 = CARTESIAN_POINT ( 'NONE',  ( -12.49999999999999289, 2.500000000000000000, -4.922947341949750921 ) ) ;
#7065 = FACE_BOUND ( 'NONE', #104403, .T. ) ;
#7066 = DIRECTION ( 'NONE',  ( -4.274815082592931898E-19, -0.9999939076577903929, -0.003490651415223739937 ) ) ;
#7067 = CARTESIAN_POINT ( 'NONE',  ( 1.649999999999951505, 2.500000000000000000, 1.472243186433545459 ) ) ;
#7069 = ORIENTED_EDGE ( 'NONE', *, *, #12098, .F. ) ;
#7068 = AXIS2_PLACEMENT_3D ( 'NONE', #113074, #52240, #41792 ) ;
#7071 = AXIS2_PLACEMENT_3D ( 'NONE', #95490, #26112, #66024 ) ;
#7070 = CARTESIAN_POINT ( 'NONE',  ( -3.550000000000027356, 2.500000000000000000, 1.918653347947321564 ) ) ;
#7072 = FACE_OUTER_BOUND ( 'NONE', #113542, .T. ) ;
#7073 = VERTEX_POINT ( 'NONE', #24824 ) ;
#7074 = CARTESIAN_POINT ( 'NONE',  ( 12.09999999999990550, 2.500000000000000000, 4.430127018922196847 ) ) ;
#7075 = CARTESIAN_POINT ( 'NONE',  ( -4.400000000000025224, 2.500000000000000000, 3.883716857408420431 ) ) ;
#7076 = EDGE_CURVE ( 'NONE', #50039, #44638, #95336, .T. ) ;
#7077 = AXIS2_PLACEMENT_3D ( 'NONE', #120072, #30420, #101071 ) ;
#7078 = CIRCLE ( 'NONE', #53077, 0.1000000000000002554 ) ;
#7079 = VECTOR ( 'NONE', #11376, 1000.000000000000000 ) ;
#7080 = AXIS2_PLACEMENT_3D ( 'NONE', #44162, #35017, #84078 ) ;
#7081 = AXIS2_PLACEMENT_3D ( 'NONE', #81242, #11837, #60943 ) ;
#7082 = EDGE_LOOP ( 'NONE', ( #44611, #5300, #22087, #124119 ) ) ;
#7083 = PLANE ( 'NONE',  #73790 ) ;
#7084 = DIRECTION ( 'NONE',  ( -0.000000000000000000, -1.000000000000000000, -0.000000000000000000 ) ) ;
#7085 = EDGE_CURVE ( 'NONE', #22780, #21628, #44460, .T. ) ;
#7086 = CIRCLE ( 'NONE', #128313, 0.06509327318403745899 ) ;
#7088 = VERTEX_POINT ( 'NONE', #93568 ) ;
#7087 = CIRCLE ( 'NONE', #42645, 0.06509327318403745899 ) ;
#7089 = AXIS2_PLACEMENT_3D ( 'NONE', #81930, #73404, #13184 ) ;
#7090 = CARTESIAN_POINT ( 'NONE',  ( 2.049999999999948308, 2.500000000000000000, 6.495190528383297135 ) ) ;
#7091 = DIRECTION ( 'NONE',  ( 0.000000000000000000, 0.000000000000000000, 1.000000000000000000 ) ) ;
#7092 = ORIENTED_EDGE ( 'NONE', *, *, #29012, .T. ) ;
#7093 = CARTESIAN_POINT ( 'NONE',  ( -9.150000000000009237, 2.500000000000000000, 2.265063509461097357 ) ) ;
#7095 = ORIENTED_EDGE ( 'NONE', *, *, #10518, .T. ) ;
#7094 = CIRCLE ( 'NONE', #117816, 0.06509327318403745899 ) ;
#7096 = EDGE_CURVE ( 'NONE', #113294, #58747, #13842, .T. ) ;
#7097 = VERTEX_POINT ( 'NONE', #113855 ) ;
#7098 = EDGE_CURVE ( 'NONE', #104335, #48350, #51521, .T. ) ;
#7099 = CARTESIAN_POINT ( 'NONE',  ( 5.399999999999934630, 2.500000000000000000, 0.6928203230275494784 ) ) ;
#7100 = VERTEX_POINT ( 'NONE', #13699 ) ;
#7101 = DIRECTION ( 'NONE',  ( 0.000000000000000000, 0.000000000000000000, 1.000000000000000000 ) ) ;
#7102 = CARTESIAN_POINT ( 'NONE',  ( 3.299999999999944755, 12.50000000000000000, 0.06509327318403504425 ) ) ;
#7103 = ORIENTED_EDGE ( 'NONE', *, *, #85728, .F. ) ;
#7104 = DIRECTION ( 'NONE',  ( 0.000000000000000000, 1.000000000000000000, 0.000000000000000000 ) ) ;
#7105 = ORIENTED_EDGE ( 'NONE', *, *, #63345, .F. ) ;
#7106 = DIRECTION ( 'NONE',  ( -0.000000000000000000, 1.000000000000000000, -0.000000000000000000 ) ) ;
#7107 = AXIS2_PLACEMENT_3D ( 'NONE', #33848, #92116, #102580 ) ;
#7108 = CARTESIAN_POINT ( 'NONE',  ( -0.4000000000000401013, 2.500000000000000000, -3.637306695894650055 ) ) ;
#7109 = FACE_OUTER_BOUND ( 'NONE', #4483, .T. ) ;
#7111 = EDGE_CURVE ( 'NONE', #2654, #79541, #45257, .T. ) ;
#7110 = DIRECTION ( 'NONE',  ( -4.274815082592931898E-19, -0.9999939076577903929, -0.003490651415223739937 ) ) ;
#7112 = DIRECTION ( 'NONE',  ( 0.000000000000000000, -0.9999939076577903929, 0.003490651415223739937 ) ) ;
#7113 = AXIS2_PLACEMENT_3D ( 'NONE', #88111, #85563, #37758 ) ;
#7114 = VERTEX_POINT ( 'NONE', #73923 ) ;
#7115 = VERTEX_POINT ( 'NONE', #115108 ) ;
#7116 = FACE_OUTER_BOUND ( 'NONE', #59392, .T. ) ;
#7117 = CARTESIAN_POINT ( 'NONE',  ( -12.89999999999999147, 2.500000000000000000, -4.330127018922198978 ) ) ;
#7118 = DIRECTION ( 'NONE',  ( -4.274815082592931898E-19, -0.9999939076577903929, -0.003490651415223739937 ) ) ;
#7120 = EDGE_LOOP ( 'NONE', ( #74979, #122568 ) ) ;
#7119 = ORIENTED_EDGE ( 'NONE', *, *, #125365, .F. ) ;
#7121 = ORIENTED_EDGE ( 'NONE', *, *, #32601, .F. ) ;
#7122 = CARTESIAN_POINT ( 'NONE',  ( -6.650000000000018119, 12.50000000000000000, -2.230156782645139391 ) ) ;
#7123 = CIRCLE ( 'NONE', #105439, 0.1000000000000002554 ) ;
#7124 = CARTESIAN_POINT ( 'NONE',  ( -3.950000000000024603, 2.500000000000000000, -2.511473670974877948 ) ) ;
#7125 = CIRCLE ( 'NONE', #36403, 0.1000000000000002554 ) ;
#7126 = CARTESIAN_POINT ( 'NONE',  ( -13.94999999999998685, 2.500000000000000000, -2.411473670974875638 ) ) ;
#7127 = CARTESIAN_POINT ( 'NONE',  ( 1.649999999999951505, 2.500000000000000000, 2.857883832488649301 ) ) ;
#7128 = LINE ( 'NONE', #66059, #6285 ) ;
#7129 = CARTESIAN_POINT ( 'NONE',  ( 0.8499999999999553468, 12.50000000000000000, 2.165063509461097713 ) ) ;
#7130 = CARTESIAN_POINT ( 'NONE',  ( -8.150000000000014566, 2.500000000000000000, -6.841600689897073373 ) ) ;
#7131 = CARTESIAN_POINT ( 'NONE',  ( -8.150000000000014566, 12.50000000000000000, -6.148780366869520897 ) ) ;
#7132 = DIRECTION ( 'NONE',  ( 0.000000000000000000, 0.000000000000000000, 1.000000000000000000 ) ) ;
#7133 = EDGE_LOOP ( 'NONE', ( #41566, #109180, #41717, #80305 ) ) ;
#7134 = CIRCLE ( 'NONE', #21843, 0.06509327318403745899 ) ;
#7135 = ADVANCED_FACE ( 'NONE', ( #3886 ), #43844, .T. ) ;
#7136 = DIRECTION ( 'NONE',  ( 0.000000000000000000, 0.000000000000000000, -1.000000000000000000 ) ) ;
#7137 = ORIENTED_EDGE ( 'NONE', *, *, #119319, .F. ) ;
#7138 = VERTEX_POINT ( 'NONE', #104033 ) ;
#7139 = EDGE_CURVE ( 'NONE', #129332, #78385, #14339, .T. ) ;
#7140 = DIRECTION ( 'NONE',  ( -0.000000000000000000, 1.000000000000000000, -0.000000000000000000 ) ) ;
#7141 = CARTESIAN_POINT ( 'NONE',  ( 15.19999999999989271, 12.50000000000000000, -0.2813168883297409439 ) ) ;
#7142 = DIRECTION ( 'NONE',  ( 0.000000000000000000, 0.000000000000000000, -1.000000000000000000 ) ) ;
#7143 = ADVANCED_FACE ( 'NONE', ( #74568 ), #53576, .T. ) ;
#7144 = CARTESIAN_POINT ( 'NONE',  ( -13.14999999999999147, 12.50000000000000000, 2.511473670974877503 ) ) ;
#7145 = DIRECTION ( 'NONE',  ( 0.000000000000000000, 0.000000000000000000, 1.000000000000000000 ) ) ;
#7146 = VECTOR ( 'NONE', #74686, 1000.000000000000000 ) ;
#7147 = DIRECTION ( 'NONE',  ( 0.000000000000000000, 0.000000000000000000, 1.000000000000000000 ) ) ;
#7148 = AXIS2_PLACEMENT_3D ( 'NONE', #9321, #79367, #30274 ) ;
#7149 = CARTESIAN_POINT ( 'NONE',  ( 14.34999999999989306, 2.500000000000000000, -2.611473670974877592 ) ) ;
#7150 = ORIENTED_EDGE ( 'NONE', *, *, #91105, .T. ) ;
#7151 = CARTESIAN_POINT ( 'NONE',  ( 1.049999999999953637, 2.500000000000000000, 2.511473670974873507 ) ) ;
#7152 = ADVANCED_FACE ( 'NONE', ( #95496 ), #76558, .T. ) ;
#7153 = ADVANCED_FACE ( 'NONE', ( #115778 ), #105962, .T. ) ;
#7154 = CONICAL_SURFACE ( 'NONE', #82494, 0.1000000000000002554, 0.003490658503988666988 ) ;
#7155 = ADVANCED_FACE ( 'NONE', ( #75843 ), #93281, .T. ) ;
#7156 = ADVANCED_FACE ( 'NONE', ( #27378 ), #128814, .T. ) ;
#7157 = AXIS2_PLACEMENT_3D ( 'NONE', #57468, #87553, #50233 ) ;
#7158 = DIRECTION ( 'NONE',  ( -4.274815082592931898E-19, -0.9999939076577903929, -0.003490651415223739937 ) ) ;
#7159 = ORIENTED_EDGE ( 'NONE', *, *, #43555, .F. ) ;
#7160 = ADVANCED_FACE ( 'NONE', ( #18859 ), #15897, .T. ) ;
#7161 = EDGE_LOOP ( 'NONE', ( #21529, #9268, #66233, #100365 ) ) ;
#7162 = VERTEX_POINT ( 'NONE', #97421 ) ;
#7163 = ORIENTED_EDGE ( 'NONE', *, *, #36078, .T. ) ;
#7164 = LINE ( 'NONE', #108601, #46199 ) ;
#7165 = DIRECTION ( 'NONE',  ( 0.000000000000000000, 1.000000000000000000, 0.000000000000000000 ) ) ;
#7166 = EDGE_CURVE ( 'NONE', #27968, #129597, #16895, .T. ) ;
#7167 = EDGE_LOOP ( 'NONE', ( #44695, #53554, #64970, #4318 ) ) ;
#7168 = DIRECTION ( 'NONE',  ( 0.000000000000000000, 0.000000000000000000, 1.000000000000000000 ) ) ;
#7169 = DIRECTION ( 'NONE',  ( 0.000000000000000000, 1.000000000000000000, 0.000000000000000000 ) ) ;
#7170 = CONICAL_SURFACE ( 'NONE', #101271, 0.1000000000000002554, 0.003490658503988666988 ) ;
#7171 = AXIS2_PLACEMENT_3D ( 'NONE', #55472, #6331, #116301 ) ;
#7172 = CARTESIAN_POINT ( 'NONE',  ( 7.299999999999926104, 2.500000000000000000, -3.883716857408426648 ) ) ;
#7173 = EDGE_LOOP ( 'NONE', ( #34390, #39269 ) ) ;
#7174 = AXIS2_PLACEMENT_3D ( 'NONE', #78334, #68486, #108408 ) ;
#7175 = VECTOR ( 'NONE', #75057, 1000.000000000000000 ) ;
#7176 = DIRECTION ( 'NONE',  ( 0.000000000000000000, 0.000000000000000000, 1.000000000000000000 ) ) ;
#7177 = DIRECTION ( 'NONE',  ( -1.000000000000000000, 0.000000000000000000, 0.000000000000000000 ) ) ;
#7178 = ORIENTED_EDGE ( 'NONE', *, *, #16275, .T. ) ;
#7179 = VECTOR ( 'NONE', #9309, 1000.000000000000000 ) ;
#7180 = CONICAL_SURFACE ( 'NONE', #23934, 0.1000000000000002554, 0.003490658503988666988 ) ;
#7181 = VERTEX_POINT ( 'NONE', #58800 ) ;
#7182 = EDGE_LOOP ( 'NONE', ( #85221, #123465, #97254, #129422 ) ) ;
#7183 = CARTESIAN_POINT ( 'NONE',  ( 4.799999999999934097, 2.500000000000000000, 4.676537180435972552 ) ) ;
#7184 = CARTESIAN_POINT ( 'NONE',  ( -1.650000000000035660, 12.50000000000000000, 7.122917578226811486 ) ) ;
#7185 = CONICAL_SURFACE ( 'NONE', #9262, 0.1000000000000000472, 0.003490658503988666988 ) ;
#7186 = AXIS2_PLACEMENT_3D ( 'NONE', #5787, #46365, #26739 ) ;
#7187 = VECTOR ( 'NONE', #121622, 1000.000000000000000 ) ;
#7188 = ORIENTED_EDGE ( 'NONE', *, *, #38743, .T. ) ;
#7189 = DIRECTION ( 'NONE',  ( -4.274815082592931898E-19, -0.9999939076577903929, -0.003490651415223739937 ) ) ;
#7190 = CARTESIAN_POINT ( 'NONE',  ( -9.200000000000006395, 12.50000000000000000, 4.265033745738159077 ) ) ;
#7191 = DIRECTION ( 'NONE',  ( -0.000000000000000000, -1.000000000000000000, -0.000000000000000000 ) ) ;
#7192 = DIRECTION ( 'NONE',  ( -0.000000000000000000, -1.000000000000000000, -0.000000000000000000 ) ) ;
#7193 = ORIENTED_EDGE ( 'NONE', *, *, #97659, .T. ) ;
#7194 = DIRECTION ( 'NONE',  ( -0.000000000000000000, 1.000000000000000000, -0.000000000000000000 ) ) ;
#7195 = ADVANCED_FACE ( 'NONE', ( #98066 ), #18212, .T. ) ;
#7196 = ORIENTED_EDGE ( 'NONE', *, *, #64781, .F. ) ;
#7197 = ORIENTED_EDGE ( 'NONE', *, *, #28903, .F. ) ;
#7198 = ORIENTED_EDGE ( 'NONE', *, *, #32344, .F. ) ;
#7199 = DIRECTION ( 'NONE',  ( 0.000000000000000000, 1.000000000000000000, 0.000000000000000000 ) ) ;
#7200 = FACE_BOUND ( 'NONE', #63566, .T. ) ;
#7201 = LINE ( 'NONE', #47800, #22122 ) ;
#7202 = AXIS2_PLACEMENT_3D ( 'NONE', #65692, #16573, #77448 ) ;
#7203 = CARTESIAN_POINT ( 'NONE',  ( 14.14999999999989555, 2.500000000000000000, 2.165063509461097713 ) ) ;
#7204 = DIRECTION ( 'NONE',  ( -0.000000000000000000, 1.000000000000000000, -0.000000000000000000 ) ) ;
#7205 = EDGE_CURVE ( 'NONE', #41083, #87429, #47310, .T. ) ;
#7206 = ORIENTED_EDGE ( 'NONE', *, *, #2807, .T. ) ;
#7207 = CARTESIAN_POINT ( 'NONE',  ( 11.24999999999990763, 2.500000000000000000, -7.188010851410854052 ) ) ;
#7208 = CARTESIAN_POINT ( 'NONE',  ( -6.650000000000018119, 12.50000000000000000, -7.253104124594891289 ) ) ;
#7209 = CARTESIAN_POINT ( 'NONE',  ( 17.49862860983209956, 2.500000000000000000, 4.081131818001135336 ) ) ;
#7210 = DIRECTION ( 'NONE',  ( 0.000000000000000000, 0.000000000000000000, 1.000000000000000000 ) ) ;
#7211 = ORIENTED_EDGE ( 'NONE', *, *, #97695, .F. ) ;
#7212 = VECTOR ( 'NONE', #12379, 1000.000000000000000 ) ;
#7213 = DIRECTION ( 'NONE',  ( 1.000000000000000000, -0.000000000000000000, -0.000000000000000000 ) ) ;
#7214 = DIRECTION ( 'NONE',  ( -0.000000000000000000, -1.000000000000000000, -0.000000000000000000 ) ) ;
#7215 = ORIENTED_EDGE ( 'NONE', *, *, #12766, .F. ) ;
#7216 = DIRECTION ( 'NONE',  ( 0.000000000000000000, 0.000000000000000000, -1.000000000000000000 ) ) ;
#7217 = DIRECTION ( 'NONE',  ( 0.000000000000000000, 1.000000000000000000, 0.000000000000000000 ) ) ;
#7218 = FACE_BOUND ( 'NONE', #72971, .T. ) ;
#7219 = CARTESIAN_POINT ( 'NONE',  ( 12.89999999999990088, 2.500000000000000000, -4.330127018922201643 ) ) ;
#7220 = AXIS2_PLACEMENT_3D ( 'NONE', #13960, #122001, #92527 ) ;
#7221 = VERTEX_POINT ( 'NONE', #67283 ) ;
#7222 = CARTESIAN_POINT ( 'NONE',  ( -14.39999999999998614, 12.50000000000000000, 0.3464101615137758494 ) ) ;
#7223 = AXIS2_PLACEMENT_3D ( 'NONE', #119782, #27516, #117830 ) ;
#7224 = ORIENTED_EDGE ( 'NONE', *, *, #58871, .T. ) ;
#7225 = EDGE_LOOP ( 'NONE', ( #89757, #117652 ) ) ;
#7226 = DIRECTION ( 'NONE',  ( 0.000000000000000000, -0.000000000000000000, 1.000000000000000000 ) ) ;
#7227 = CARTESIAN_POINT ( 'NONE',  ( 186.7500000000000000, 9.429780353434619030E-16, -7.700000000000000178 ) ) ;
#7228 = ORIENTED_EDGE ( 'NONE', *, *, #52058, .F. ) ;
#7229 = CARTESIAN_POINT ( 'NONE',  ( 185.4218750003414016, 0.000000000000000000, 7.564683531250000925 ) ) ;
#7230 = DIRECTION ( 'NONE',  ( 0.000000000000000000, -0.9999939076577903929, 0.003490651415223739937 ) ) ;
#7231 = EDGE_CURVE ( 'NONE', #35583, #102949, #9653, .T. ) ;
#7232 = AXIS2_PLACEMENT_3D ( 'NONE', #79211, #98827, #18971 ) ;
#7233 = AXIS2_PLACEMENT_3D ( 'NONE', #15454, #95322, #24650 ) ;
#7234 = LINE ( 'NONE', #63934, #101229 ) ;
#7235 = CIRCLE ( 'NONE', #95096, 0.09999999999999982514 ) ;
#7236 = CARTESIAN_POINT ( 'NONE',  ( 185.6145833340161175, 6.668395609140177704, -3.849999999999998312 ) ) ;
#7237 = AXIS2_PLACEMENT_3D ( 'NONE', #18011, #27190, #78249 ) ;
#7238 = EDGE_CURVE ( 'NONE', #12542, #51573, #36853, .T. ) ;
#7239 = ORIENTED_EDGE ( 'NONE', *, *, #71906, .F. ) ;
#7240 = CARTESIAN_POINT ( 'NONE',  ( 8.149999999999920419, 2.500000000000000000, -2.511473670974877948 ) ) ;
#7241 = CARTESIAN_POINT ( 'NONE',  ( 5.849999999999933031, 12.50000000000000000, 7.122917578226811486 ) ) ;
#7242 = FACE_OUTER_BOUND ( 'NONE', #40721, .T. ) ;
#7243 = CARTESIAN_POINT ( 'NONE',  ( 10.19999999999991225, 2.500000000000000000, 3.983716857408420076 ) ) ;
#7244 = EDGE_LOOP ( 'NONE', ( #62942, #63922, #43575, #19900 ) ) ;
#7245 = EDGE_CURVE ( 'NONE', #51302, #94018, #32670, .T. ) ;
#7246 = DIRECTION ( 'NONE',  ( -0.000000000000000000, 1.000000000000000000, -0.000000000000000000 ) ) ;
#7247 = ORIENTED_EDGE ( 'NONE', *, *, #79319, .T. ) ;
#7248 = EDGE_CURVE ( 'NONE', #78678, #50948, #114211, .T. ) ;
#7249 = DIRECTION ( 'NONE',  ( 0.000000000000000000, 1.000000000000000000, 0.000000000000000000 ) ) ;
#7250 = CARTESIAN_POINT ( 'NONE',  ( 1.699999999999950218, 12.50000000000000000, 4.330127018922196314 ) ) ;
#7251 = ORIENTED_EDGE ( 'NONE', *, *, #18073, .T. ) ;
#7252 = FACE_OUTER_BOUND ( 'NONE', #45506, .T. ) ;
#7253 = CARTESIAN_POINT ( 'NONE',  ( 10.44999999999991402, 2.500000000000000000, -2.065063509461102065 ) ) ;
#7254 = DIRECTION ( 'NONE',  ( -0.000000000000000000, -1.000000000000000000, -0.000000000000000000 ) ) ;
#7256 = CARTESIAN_POINT ( 'NONE',  ( -4.350000000000023626, 12.50000000000000000, 6.841600689897072485 ) ) ;
#7255 = AXIS2_PLACEMENT_3D ( 'NONE', #116462, #125636, #6480 ) ;
#7257 = ORIENTED_EDGE ( 'NONE', *, *, #65843, .T. ) ;
#7258 = ADVANCED_FACE ( 'NONE', ( #76507 ), #122526, .T. ) ;
#7259 = AXIS2_PLACEMENT_3D ( 'NONE', #18108, #40354, #28590 ) ;
#7260 = CARTESIAN_POINT ( 'NONE',  ( 11.04999999999991012, 2.500000000000000000, -1.718653347947326049 ) ) ;
#7261 = FACE_OUTER_BOUND ( 'NONE', #25716, .T. ) ;
#7262 = AXIS2_PLACEMENT_3D ( 'NONE', #14702, #76236, #64463 ) ;
#7263 = CIRCLE ( 'NONE', #118085, 0.06509327318403745899 ) ;
#7264 = CARTESIAN_POINT ( 'NONE',  ( 185.2343750003414016, 8.734944146203032389, 5.348610694689227483E-16 ) ) ;
#7265 = CARTESIAN_POINT ( 'NONE',  ( 7.899999999999924860, 2.500000000000000000, -4.330127018922201643 ) ) ;
#7266 = EDGE_CURVE ( 'NONE', #9428, #93110, #103749, .T. ) ;
#7267 = CARTESIAN_POINT ( 'NONE',  ( 5.849999999999935696, 2.500000000000000000, -6.595190528383302109 ) ) ;
#7268 = CIRCLE ( 'NONE', #80462, 0.06509327318403741736 ) ;
#7269 = EDGE_LOOP ( 'NONE', ( #61812, #5739 ) ) ;
#7270 = EDGE_LOOP ( 'NONE', ( #122029, #46509 ) ) ;
#7272 = CARTESIAN_POINT ( 'NONE',  ( 11.89999999999990443, 2.500000000000000000, -0.3464101615137782364 ) ) ;
#7271 = CIRCLE ( 'NONE', #113908, 0.06509327318403745899 ) ;
#7273 = ORIENTED_EDGE ( 'NONE', *, *, #121200, .F. ) ;
#7274 = CARTESIAN_POINT ( 'NONE',  ( -14.59999999999998366, 2.500000000000000000, -1.084202172485504434E-16 ) ) ;
#7277 = ORIENTED_EDGE ( 'NONE', *, *, #91362, .T. ) ;
#7276 = ORIENTED_EDGE ( 'NONE', *, *, #96380, .T. ) ;
#7275 = AXIS2_PLACEMENT_3D ( 'NONE', #119549, #61295, #109752 ) ;
#7278 = ORIENTED_EDGE ( 'NONE', *, *, #129130, .F. ) ;
#7279 = CARTESIAN_POINT ( 'NONE',  ( -15.39999999999997904, 2.500000000000000000, -0.1000000000000000056 ) ) ;
#7280 = CIRCLE ( 'NONE', #21987, 0.1000000000000000472 ) ;
#7282 = CIRCLE ( 'NONE', #116049, 0.06509327318403745899 ) ;
#7281 = CARTESIAN_POINT ( 'NONE',  ( 6.449999999999928235, 12.50000000000000000, 2.511473670974873507 ) ) ;
#7283 = DIRECTION ( 'NONE',  ( 0.000000000000000000, 0.000000000000000000, 1.000000000000000000 ) ) ;
#7284 = CARTESIAN_POINT ( 'NONE',  ( 9.149999999999916866, 12.50000000000000000, -2.857883832488653741 ) ) ;
#7285 = DIRECTION ( 'NONE',  ( 0.000000000000000000, 0.000000000000000000, 1.000000000000000000 ) ) ;
#7286 = VECTOR ( 'NONE', #104566, 1000.000000000000000 ) ;
#7287 = PLANE ( 'NONE',  #47651 ) ;
#7288 = ORIENTED_EDGE ( 'NONE', *, *, #129076, .T. ) ;
#7289 = CARTESIAN_POINT ( 'NONE',  ( 13.29999999999990301, 2.500000000000000000, -4.430127018922202176 ) ) ;
#7290 = ORIENTED_EDGE ( 'NONE', *, *, #74829, .T. ) ;
#7291 = ORIENTED_EDGE ( 'NONE', *, *, #108108, .T. ) ;
#7292 = ORIENTED_EDGE ( 'NONE', *, *, #83179, .T. ) ;
#7293 = ORIENTED_EDGE ( 'NONE', *, *, #32181, .T. ) ;
#7294 = DIRECTION ( 'NONE',  ( 0.000000000000000000, 0.000000000000000000, -1.000000000000000000 ) ) ;
#7295 = ORIENTED_EDGE ( 'NONE', *, *, #36520, .T. ) ;
#7296 = ORIENTED_EDGE ( 'NONE', *, *, #62355, .T. ) ;
#7297 = AXIS2_PLACEMENT_3D ( 'NONE', #1456, #79395, #50554 ) ;
#7298 = DIRECTION ( 'NONE',  ( 0.000000000000000000, 0.000000000000000000, 1.000000000000000000 ) ) ;
#7299 = DIRECTION ( 'NONE',  ( -0.000000000000000000, 1.000000000000000000, -0.000000000000000000 ) ) ;
#7301 = LINE ( 'NONE', #88442, #54654 ) ;
#7300 = PRODUCT ( 'Inductive Wireless Charging Base', 'Inductive Wireless Charging Base', '', ( #106626 ) ) ;
#7302 = FACE_OUTER_BOUND ( 'NONE', #4448, .T. ) ;
#7303 = ADVANCED_FACE ( 'NONE', ( #87596 ), #18048, .T. ) ;
#7304 = DIRECTION ( 'NONE',  ( -0.000000000000000000, 1.000000000000000000, -0.000000000000000000 ) ) ;
#7305 = EDGE_LOOP ( 'NONE', ( #122179, #105513 ) ) ;
#7306 = EDGE_CURVE ( 'NONE', #71809, #104716, #97483, .T. ) ;
#7307 = EDGE_CURVE ( 'NONE', #62993, #107468, #118407, .T. ) ;
#7308 = DIRECTION ( 'NONE',  ( 0.000000000000000000, 0.000000000000000000, 1.000000000000000000 ) ) ;
#7309 = AXIS2_PLACEMENT_3D ( 'NONE', #94517, #85350, #24500 ) ;
#7310 = ADVANCED_FACE ( 'NONE', ( #38539 ), #3388, .T. ) ;
#7311 = CIRCLE ( 'NONE', #95156, 0.09999999999999999167 ) ;
#7312 = EDGE_LOOP ( 'NONE', ( #3928, #86218, #39468, #29700 ) ) ;
#7313 = CARTESIAN_POINT ( 'NONE',  ( -1.050000000000037792, 12.50000000000000000, 6.213873640053558134 ) ) ;
#7314 = ORIENTED_EDGE ( 'NONE', *, *, #50167, .T. ) ;
#7315 = CARTESIAN_POINT ( 'NONE',  ( 11.44999999999990514, 2.500000000000000000, -6.148780366869526226 ) ) ;
#7316 = ADVANCED_FACE ( 'NONE', ( #11622 ), #78715, .T. ) ;
#7317 = ORIENTED_EDGE ( 'NONE', *, *, #57930, .T. ) ;
#7318 = ORIENTED_EDGE ( 'NONE', *, *, #41614, .T. ) ;
#7319 = DIRECTION ( 'NONE',  ( 0.000000000000000000, -0.9999939076577903929, 0.003490651415223739937 ) ) ;
#7320 = DIRECTION ( 'NONE',  ( 0.000000000000000000, 0.000000000000000000, -1.000000000000000000 ) ) ;
#7321 = ADVANCED_FACE ( 'NONE', ( #60735 ), #128906, .T. ) ;
#7322 = AXIS2_PLACEMENT_3D ( 'NONE', #54377, #33474, #84496 ) ;
#7323 = EDGE_CURVE ( 'NONE', #71326, #98343, #55706, .T. ) ;
#7324 = DIRECTION ( 'NONE',  ( -4.274815082592931898E-19, -0.9999939076577903929, -0.003490651415223739937 ) ) ;
#7325 = LINE ( 'NONE', #66891, #56973 ) ;
#7326 = VECTOR ( 'NONE', #41246, 1000.000000000000000 ) ;
#7327 = DIRECTION ( 'NONE',  ( 0.000000000000000000, 1.000000000000000000, 0.000000000000000000 ) ) ;
#7328 = ORIENTED_EDGE ( 'NONE', *, *, #95250, .F. ) ;
#7329 = FACE_OUTER_BOUND ( 'NONE', #7754, .T. ) ;
#7330 = DIRECTION ( 'NONE',  ( -0.000000000000000000, -1.000000000000000000, -0.000000000000000000 ) ) ;
#7331 = CARTESIAN_POINT ( 'NONE',  ( -10.80000000000000071, 2.500000000000000000, 4.330127018922196314 ) ) ;
#7332 = CARTESIAN_POINT ( 'NONE',  ( -0.4500000000000397571, 12.50000000000000000, -6.560283801567339701 ) ) ;
#7333 = CARTESIAN_POINT ( 'NONE',  ( 2.699999999999944666, 2.500000000000000000, 4.576537180435972019 ) ) ;
#7334 = ORIENTED_EDGE ( 'NONE', *, *, #80756, .T. ) ;
#7335 = AXIS2_PLACEMENT_3D ( 'NONE', #95942, #67768, #46194 ) ;
#7336 = AXIS2_PLACEMENT_3D ( 'NONE', #71659, #61199, #101122 ) ;
#7337 = EDGE_LOOP ( 'NONE', ( #95649, #81461, #7692, #112398 ) ) ;
#7338 = FACE_OUTER_BOUND ( 'NONE', #117262, .T. ) ;
#7339 = EDGE_CURVE ( 'NONE', #40266, #55057, #66082, .T. ) ;
#7340 = VERTEX_POINT ( 'NONE', #49638 ) ;
#7341 = PLANE ( 'NONE',  #17309 ) ;
#7342 = DIRECTION ( 'NONE',  ( 0.000000000000000000, 0.000000000000000000, 1.000000000000000000 ) ) ;
#7343 = ORIENTED_EDGE ( 'NONE', *, *, #13009, .F. ) ;
#7344 = CARTESIAN_POINT ( 'NONE',  ( 184.9583333333333144, 4.445597072760117285, 7.699999999999999289 ) ) ;
#7345 = FACE_OUTER_BOUND ( 'NONE', #50276, .T. ) ;
#7346 = CARTESIAN_POINT ( 'NONE',  ( -5.850000000000019185, 2.500000000000000000, 6.595190528383296780 ) ) ;
#7347 = DIRECTION ( 'NONE',  ( -0.000000000000000000, 1.000000000000000000, -0.000000000000000000 ) ) ;
#7348 = CYLINDRICAL_SURFACE ( 'NONE', #103980, 7.700000000000000178 ) ;
#7349 = VERTEX_POINT ( 'NONE', #121568 ) ;
#7351 = DIRECTION ( 'NONE',  ( -0.000000000000000000, -1.000000000000000000, -0.000000000000000000 ) ) ;
#7350 = CIRCLE ( 'NONE', #17822, 0.1000000000000000472 ) ;
#7352 = PLANE ( 'NONE',  #108300 ) ;
#7353 = AXIS2_PLACEMENT_3D ( 'NONE', #115499, #75583, #67039 ) ;
#7354 = VERTEX_POINT ( 'NONE', #111090 ) ;
#7355 = AXIS2_PLACEMENT_3D ( 'NONE', #44640, #84563, #104822 ) ;
#7356 =( BOUNDED_CURVE ( )  B_SPLINE_CURVE ( 2, ( #44147, #36283, #95829 ),
 .UNSPECIFIED., .F., .F. ) 
 B_SPLINE_CURVE_WITH_KNOTS ( ( 3, 3 ),
 ( -6.000000000053022403E-08, 0.01482991977946481257 ),
 .UNSPECIFIED. ) 
 CURVE ( )  GEOMETRIC_REPRESENTATION_ITEM ( )  RATIONAL_B_SPLINE_CURVE ( ( 1.000000000000000000, 0.7762344340431478473, 0.8943752373141966583 ) ) 
 REPRESENTATION_ITEM ( '' )  );
#7357 = DIRECTION ( 'NONE',  ( 0.000000000000000000, 0.000000000000000000, -1.000000000000000000 ) ) ;
#7358 = DIRECTION ( 'NONE',  ( 0.000000000000000000, 0.000000000000000000, -1.000000000000000000 ) ) ;
#7359 = DIRECTION ( 'NONE',  ( 0.000000000000000000, 1.000000000000000000, 0.000000000000000000 ) ) ;
#7360 = ADVANCED_FACE ( 'NONE', ( #29992 ), #49478, .T. ) ;
#7361 = AXIS2_PLACEMENT_3D ( 'NONE', #30643, #70543, #61384 ) ;
#7362 = ORIENTED_EDGE ( 'NONE', *, *, #65468, .F. ) ;
#7363 = CIRCLE ( 'NONE', #78509, 0.1000000000000002554 ) ;
#7364 = DIRECTION ( 'NONE',  ( -0.000000000000000000, 1.000000000000000000, -0.000000000000000000 ) ) ;
#7365 = AXIS2_PLACEMENT_3D ( 'NONE', #64503, #124717, #112326 ) ;
#7366 = EDGE_LOOP ( 'NONE', ( #101263, #24557, #12457, #66313 ) ) ;
#7367 = LINE ( 'NONE', #86578, #60557 ) ;
#7368 = DIRECTION ( 'NONE',  ( 0.000000000000000000, 0.000000000000000000, 1.000000000000000000 ) ) ;
#7369 = DIRECTION ( 'NONE',  ( 0.000000000000000000, 0.000000000000000000, -1.000000000000000000 ) ) ;
#7370 = ORIENTED_EDGE ( 'NONE', *, *, #107637, .F. ) ;
#7371 = CIRCLE ( 'NONE', #61875, 0.09999999999999982514 ) ;
#7372 = VECTOR ( 'NONE', #23696, 1000.000000000000000 ) ;
#7373 = CARTESIAN_POINT ( 'NONE',  ( -5.650000000000023448, 2.500000000000000000, -6.841600689897078702 ) ) ;
#7374 = CARTESIAN_POINT ( 'NONE',  ( -1.250000000000036193, 2.500000000000000000, 5.902370205355745192 ) ) ;
#7375 = CONICAL_SURFACE ( 'NONE', #80566, 0.1000000000000002554, 0.003490658503988666988 ) ;
#7376 = ORIENTED_EDGE ( 'NONE', *, *, #83548, .F. ) ;
#7377 = DIRECTION ( 'NONE',  ( 0.000000000000000000, 0.000000000000000000, -1.000000000000000000 ) ) ;
#7378 = ORIENTED_EDGE ( 'NONE', *, *, #94601, .F. ) ;
#7379 = DIRECTION ( 'NONE',  ( 0.000000000000000000, -0.9999939076577903929, 0.003490651415223739937 ) ) ;
#7380 = ORIENTED_EDGE ( 'NONE', *, *, #6399, .F. ) ;
#7381 = CARTESIAN_POINT ( 'NONE',  ( 2.949999999999946887, 2.500000000000000000, -2.165063509461101710 ) ) ;
#7382 = FACE_OUTER_BOUND ( 'NONE', #104088, .T. ) ;
#7383 = EDGE_LOOP ( 'NONE', ( #108038, #7103, #97109, #30433 ) ) ;
#7384 = ORIENTED_EDGE ( 'NONE', *, *, #81185, .T. ) ;
#7385 = CARTESIAN_POINT ( 'NONE',  ( 8.949999999999919353, 12.50000000000000000, -6.213873640053564351 ) ) ;
#7386 = CARTESIAN_POINT ( 'NONE',  ( 3.349999999999943689, 12.50000000000000000, 2.230156782645134950 ) ) ;
#7387 = AXIS2_PLACEMENT_3D ( 'NONE', #122536, #32882, #53783 ) ;
#7388 = ORIENTED_EDGE ( 'NONE', *, *, #120116, .F. ) ;
#7389 = DIRECTION ( 'NONE',  ( 0.000000000000000000, 0.000000000000000000, 1.000000000000000000 ) ) ;
#7390 = LINE ( 'NONE', #17190, #70147 ) ;
#7391 = CARTESIAN_POINT ( 'NONE',  ( -3.469446951953614189E-14, 2.500000000000000000, -0.5928203230275518321 ) ) ;
#7392 = CARTESIAN_POINT ( 'NONE',  ( 7.899999999999924860, 2.500000000000000000, -4.430127018922202176 ) ) ;
#7393 = DIRECTION ( 'NONE',  ( -0.000000000000000000, 1.000000000000000000, -0.000000000000000000 ) ) ;
#7394 = DIRECTION ( 'NONE',  ( -0.000000000000000000, 1.000000000000000000, -0.000000000000000000 ) ) ;
#7395 = CIRCLE ( 'NONE', #51355, 0.06509327318403745899 ) ;
#7396 = CONICAL_SURFACE ( 'NONE', #53397, 0.09999999999999999167, 0.003490658503988666988 ) ;
#7397 = ADVANCED_FACE ( 'NONE', ( #60106 ), #100014, .T. ) ;
#7398 = ORIENTED_EDGE ( 'NONE', *, *, #124326, .T. ) ;
#7399 = ORIENTED_EDGE ( 'NONE', *, *, #20357, .F. ) ;
#7400 = ORIENTED_EDGE ( 'NONE', *, *, #41893, .F. ) ;
#7401 = ORIENTED_EDGE ( 'NONE', *, *, #17034, .F. ) ;
#7402 = DIRECTION ( 'NONE',  ( 0.000000000000000000, 0.000000000000000000, 1.000000000000000000 ) ) ;
#7403 = FACE_OUTER_BOUND ( 'NONE', #60146, .T. ) ;
#7404 = CARTESIAN_POINT ( 'NONE',  ( -13.74999999999995381, 2.500000000000000000, -2.165063509461099489 ) ) ;
#7405 = ORIENTED_EDGE ( 'NONE', *, *, #114862, .F. ) ;
#7406 = EDGE_CURVE ( 'NONE', #64905, #26903, #15986, .T. ) ;
#7407 = FACE_BOUND ( 'NONE', #92262, .T. ) ;
#7408 = ADVANCED_FACE ( 'NONE', ( #1791 ), #26479, .T. ) ;
#7409 = DIRECTION ( 'NONE',  ( -0.000000000000000000, 1.000000000000000000, -0.000000000000000000 ) ) ;
#7410 = CARTESIAN_POINT ( 'NONE',  ( 4.349999999999940137, 12.50000000000000000, -2.576566944158915184 ) ) ;
#7411 = VECTOR ( 'NONE', #60214, 1000.000000000000000 ) ;
#7412 = PLANE ( 'NONE',  #95131 ) ;
#7413 = DIRECTION ( 'NONE',  ( 0.000000000000000000, 1.000000000000000000, 0.000000000000000000 ) ) ;
#7414 = AXIS2_PLACEMENT_3D ( 'NONE', #52820, #61366, #121549 ) ;
#7415 = CARTESIAN_POINT ( 'NONE',  ( 4.349999999999940137, 12.50000000000000000, -6.841600689897078702 ) ) ;
#7416 = EDGE_CURVE ( 'NONE', #32914, #58724, #10337, .T. ) ;
#7417 = CARTESIAN_POINT ( 'NONE',  ( 12.49999999999993960, 12.50000000000000000, -4.265033745738164406 ) ) ;
#7418 = ADVANCED_FACE ( 'NONE', ( #110468 ), #72446, .T. ) ;
#7419 = PLANE ( 'NONE',  #43628 ) ;
#7420 = DIRECTION ( 'NONE',  ( -0.000000000000000000, 1.000000000000000000, -0.000000000000000000 ) ) ;
#7421 = ADVANCED_FACE ( 'NONE', ( #1159 ), #59470, .T. ) ;
#7422 = CARTESIAN_POINT ( 'NONE',  ( 6.449999999999933564, 2.500000000000000000, -6.841600689897078702 ) ) ;
#7423 = ADVANCED_FACE ( 'NONE', ( #111767 ), #53694, .T. ) ;
#7424 = EDGE_CURVE ( 'NONE', #76377, #103647, #12259, .T. ) ;
#7425 = DIRECTION ( 'NONE',  ( 0.000000000000000000, 0.000000000000000000, -1.000000000000000000 ) ) ;
#7426 = CIRCLE ( 'NONE', #47156, 0.06509327318403745899 ) ;
#7427 = ORIENTED_EDGE ( 'NONE', *, *, #3436, .T. ) ;
#7428 = ORIENTED_EDGE ( 'NONE', *, *, #71201, .T. ) ;
#7429 = CIRCLE ( 'NONE', #103600, 0.1000000000000000056 ) ;
#7430 = ORIENTED_EDGE ( 'NONE', *, *, #108036, .T. ) ;
#7431 = ORIENTED_EDGE ( 'NONE', *, *, #88462, .T. ) ;
#7432 = CARTESIAN_POINT ( 'NONE',  ( -14.54999999999998472, 12.50000000000000000, 2.165063509461101265 ) ) ;
#7433 = DIRECTION ( 'NONE',  ( 0.000000000000000000, 0.000000000000000000, -1.000000000000000000 ) ) ;
#7435 = ORIENTED_EDGE ( 'NONE', *, *, #76613, .T. ) ;
#7434 = ORIENTED_EDGE ( 'NONE', *, *, #123458, .F. ) ;
#7436 = EDGE_CURVE ( 'NONE', #114403, #19267, #5648, .T. ) ;
#7437 = EDGE_LOOP ( 'NONE', ( #57736, #483, #3373, #47186 ) ) ;
#7438 = PLANE ( 'NONE',  #98101 ) ;
#7439 = CIRCLE ( 'NONE', #67989, 0.1000000000000002554 ) ;
#7440 = DIRECTION ( 'NONE',  ( 0.000000000000000000, 0.000000000000000000, 1.000000000000000000 ) ) ;
#7441 = DIRECTION ( 'NONE',  ( 0.000000000000000000, 0.000000000000000000, -1.000000000000000000 ) ) ;
#7442 = CARTESIAN_POINT ( 'NONE',  ( 4.149999999999939959, 2.500000000000000000, 2.757883832488649656 ) ) ;
#7443 = DIRECTION ( 'NONE',  ( -4.274815082592931898E-19, -0.9999939076577903929, -0.003490651415223739937 ) ) ;
#7444 = AXIS2_PLACEMENT_3D ( 'NONE', #92146, #61427, #50301 ) ;
#7445 = ORIENTED_EDGE ( 'NONE', *, *, #19886, .F. ) ;
#7446 = DIRECTION ( 'NONE',  ( -0.000000000000000000, 1.000000000000000000, -0.000000000000000000 ) ) ;
#7447 = EDGE_LOOP ( 'NONE', ( #18985, #108648 ) ) ;
#7449 = ORIENTED_EDGE ( 'NONE', *, *, #90029, .F. ) ;
#7448 = CIRCLE ( 'NONE', #124544, 7.700000000000000178 ) ;
#7450 = ORIENTED_EDGE ( 'NONE', *, *, #20140, .T. ) ;
#7451 = AXIS2_PLACEMENT_3D ( 'NONE', #21851, #33598, #113434 ) ;
#7452 = DIRECTION ( 'NONE',  ( 0.000000000000000000, 1.000000000000000000, 0.000000000000000000 ) ) ;
#7453 = VERTEX_POINT ( 'NONE', #109162 ) ;
#7454 = EDGE_LOOP ( 'NONE', ( #53254, #54741 ) ) ;
#7455 = DIRECTION ( 'NONE',  ( 0.000000000000000000, 1.000000000000000000, 0.000000000000000000 ) ) ;
#7456 = VECTOR ( 'NONE', #40677, 1000.000000000000000 ) ;
#7457 = DIRECTION ( 'NONE',  ( 0.000000000000000000, 0.000000000000000000, 1.000000000000000000 ) ) ;
#7458 = DIRECTION ( 'NONE',  ( 0.000000000000000000, 0.000000000000000000, 1.000000000000000000 ) ) ;
#7459 = CARTESIAN_POINT ( 'NONE',  ( -12.89999999999999325, 2.500000000000000000, 0.6928203230275535862 ) ) ;
#7460 = AXIS2_PLACEMENT_3D ( 'NONE', #101060, #109599, #19932 ) ;
#7461 = CARTESIAN_POINT ( 'NONE',  ( -6.050000000000022027, 2.500000000000000000, -6.048780366869526581 ) ) ;
#7462 = ADVANCED_FACE ( 'NONE', ( #89540 ), #55836, .T. ) ;
#7463 = EDGE_LOOP ( 'NONE', ( #14561, #29056 ) ) ;
#7464 = ADVANCED_FACE ( 'NONE', ( #119632 ), #69910, .T. ) ;
#7465 = CARTESIAN_POINT ( 'NONE',  ( -7.100000000000017408, 2.500000000000000000, 0.7928203230275495672 ) ) ;
#7466 = AXIS2_PLACEMENT_3D ( 'NONE', #46790, #48726, #88637 ) ;
#7467 = AXIS2_PLACEMENT_3D ( 'NONE', #41422, #14495, #102262 ) ;
#7468 = ORIENTED_EDGE ( 'NONE', *, *, #72617, .F. ) ;
#7470 = ADVANCED_FACE ( 'NONE', ( #33842 ), #112287, .T. ) ;
#7469 = DIRECTION ( 'NONE',  ( 0.000000000000000000, 1.000000000000000000, 0.000000000000000000 ) ) ;
#7471 = CIRCLE ( 'NONE', #57660, 0.1000000000000002554 ) ;
#7472 = VERTEX_POINT ( 'NONE', #83601 ) ;
#7473 = DIRECTION ( 'NONE',  ( -0.000000000000000000, 1.000000000000000000, -0.000000000000000000 ) ) ;
#7474 = PLANE ( 'NONE',  #96331 ) ;
#7475 = CONICAL_SURFACE ( 'NONE', #26270, 0.09999999999999982514, 0.003490658503988666988 ) ;
#7476 = ORIENTED_EDGE ( 'NONE', *, *, #117951, .F. ) ;
#7477 = CARTESIAN_POINT ( 'NONE',  ( -0.6500000000000403233, 2.500000000000000000, 6.148780366869520009 ) ) ;
#7478 = EDGE_CURVE ( 'NONE', #76479, #128465, #123503, .T. ) ;
#7479 = DIRECTION ( 'NONE',  ( 0.000000000000000000, 0.000000000000000000, 1.000000000000000000 ) ) ;
#7480 = VERTEX_POINT ( 'NONE', #73129 ) ;
#7481 = ADVANCED_FACE ( 'NONE', ( #14186 ), #54133, .T. ) ;
#7482 = EDGE_CURVE ( 'NONE', #95937, #116494, #53497, .T. ) ;
#7483 = ADVANCED_FACE ( 'NONE', ( #104513 ), #65223, .T. ) ;
#7484 = DIRECTION ( 'NONE',  ( 0.000000000000000000, -0.9999939076577903929, 0.003490651415223739937 ) ) ;
#7485 = ORIENTED_EDGE ( 'NONE', *, *, #34689, .T. ) ;
#7486 = EDGE_LOOP ( 'NONE', ( #19052, #71427 ) ) ;
#7487 = FACE_OUTER_BOUND ( 'NONE', #43313, .T. ) ;
#7488 = CARTESIAN_POINT ( 'NONE',  ( -5.850000000000021849, 2.500000000000000000, -5.902370205355750521 ) ) ;
#7489 = CARTESIAN_POINT ( 'NONE',  ( 187.1302083336747444, -4.367472073101514418, -7.564683531250002702 ) ) ;
#7490 = CIRCLE ( 'NONE', #20114, 0.06509327318403745899 ) ;
#7491 = DIRECTION ( 'NONE',  ( 0.000000000000000000, -0.9999939076577903929, 0.003490651415223739937 ) ) ;
#7492 = EDGE_CURVE ( 'NONE', #103959, #30016, #43694, .T. ) ;
#7493 = CARTESIAN_POINT ( 'NONE',  ( 1.249999999999952038, 2.500000000000000000, 2.857883832488649301 ) ) ;
#7494 = CARTESIAN_POINT ( 'NONE',  ( 0.3999999999999563904, 12.50000000000000000, 3.702399969078682407 ) ) ;
#7495 = VECTOR ( 'NONE', #1945, 1000.000000000000000 ) ;
#7496 = AXIS2_PLACEMENT_3D ( 'NONE', #117322, #56498, #65677 ) ;
#7497 = ORIENTED_EDGE ( 'NONE', *, *, #100245, .T. ) ;
#7498 = CIRCLE ( 'NONE', #53491, 0.06509327318403741736 ) ;
#7499 = DIRECTION ( 'NONE',  ( -0.000000000000000000, -1.000000000000000000, -0.000000000000000000 ) ) ;
#7500 = LINE ( 'NONE', #74483, #14541 ) ;
#7501 = AXIS2_PLACEMENT_3D ( 'NONE', #119134, #128981, #39317 ) ;
#7502 = EDGE_LOOP ( 'NONE', ( #54775, #113387 ) ) ;
#7503 = CARTESIAN_POINT ( 'NONE',  ( 10.19999999999991047, 2.500000000000000000, 4.676537180435972552 ) ) ;
#7505 = EDGE_CURVE ( 'NONE', #114231, #73752, #30735, .T. ) ;
#7504 = DIRECTION ( 'NONE',  ( -0.000000000000000000, 1.000000000000000000, -0.000000000000000000 ) ) ;
#7506 = CARTESIAN_POINT ( 'NONE',  ( 10.39999999999991154, 12.50000000000000000, 5.022947341949748790 ) ) ;
#7507 = DIRECTION ( 'NONE',  ( 0.000000000000000000, 0.000000000000000000, -1.000000000000000000 ) ) ;
#7508 = PLANE ( 'NONE',  #3529 ) ;
#7509 = ORIENTED_EDGE ( 'NONE', *, *, #32031, .F. ) ;
#7510 = VECTOR ( 'NONE', #78560, 1000.000000000000000 ) ;
#7512 = AXIS2_PLACEMENT_3D ( 'NONE', #13862, #83891, #53165 ) ;
#7511 = CONICAL_SURFACE ( 'NONE', #26318, 0.1000000000000000472, 0.003490658503988666988 ) ;
#7513 = DIRECTION ( 'NONE',  ( -0.000000000000000000, -1.000000000000000000, -0.000000000000000000 ) ) ;
#7514 = EDGE_LOOP ( 'NONE', ( #70167, #50361 ) ) ;
#7515 = DIRECTION ( 'NONE',  ( -4.274815082592931898E-19, -0.9999939076577903929, -0.003490651415223739937 ) ) ;
#7516 = CIRCLE ( 'NONE', #36795, 0.1000000000000002554 ) ;
#7517 = CIRCLE ( 'NONE', #99487, 2.000000000000000000 ) ;
#7518 = ADVANCED_FACE ( 'NONE', ( #113701 ), #129033, .T. ) ;
#7519 = ORIENTED_EDGE ( 'NONE', *, *, #106482, .F. ) ;
#7520 = VERTEX_POINT ( 'NONE', #2431 ) ;
#7521 = DIRECTION ( 'NONE',  ( 0.000000000000000000, 1.000000000000000000, 0.000000000000000000 ) ) ;
#7522 = VERTEX_POINT ( 'NONE', #44304 ) ;
#7523 = DIRECTION ( 'NONE',  ( 0.000000000000000000, 0.000000000000000000, -1.000000000000000000 ) ) ;
#7524 = LINE ( 'NONE', #59889, #123658 ) ;
#7525 = CARTESIAN_POINT ( 'NONE',  ( -9.150000000000005684, 2.500000000000000000, 7.288010851410849256 ) ) ;
#7526 = ORIENTED_EDGE ( 'NONE', *, *, #86363, .T. ) ;
#7527 = FACE_BOUND ( 'NONE', #116477, .T. ) ;
#7529 = ORIENTED_EDGE ( 'NONE', *, *, #45438, .F. ) ;
#7528 = CARTESIAN_POINT ( 'NONE',  ( 7.299999999999927880, 2.500000000000000000, -4.676537180435977881 ) ) ;
#7530 = LINE ( 'NONE', #27180, #94591 ) ;
#7531 = ADVANCED_FACE ( 'NONE', ( #82315 ), #43333, .T. ) ;
#7532 = DIRECTION ( 'NONE',  ( 0.000000000000000000, 0.000000000000000000, 1.000000000000000000 ) ) ;
#7533 = ORIENTED_EDGE ( 'NONE', *, *, #8218, .F. ) ;
#7534 = AXIS2_PLACEMENT_3D ( 'NONE', #73434, #102896, #83280 ) ;
#7535 = ORIENTED_EDGE ( 'NONE', *, *, #123900, .T. ) ;
#7536 = CIRCLE ( 'NONE', #3349, 0.06509327318403745899 ) ;
#7537 = ORIENTED_EDGE ( 'NONE', *, *, #121169, .T. ) ;
#7538 = DIRECTION ( 'NONE',  ( 0.000000000000000000, -0.9999939076577903929, 0.003490651415223739937 ) ) ;
#7539 = LINE ( 'NONE', #37019, #24837 ) ;
#7540 = CARTESIAN_POINT ( 'NONE',  ( -6.650000000000018119, 2.500000000000000000, -7.088010851410853519 ) ) ;
#7541 = FACE_BOUND ( 'NONE', #105696, .T. ) ;
#7542 = ORIENTED_EDGE ( 'NONE', *, *, #28007, .T. ) ;
#7543 = CARTESIAN_POINT ( 'NONE',  ( 10.19999999999991047, 12.50000000000000000, 4.741630453620009789 ) ) ;
#7544 = PLANE ( 'NONE',  #39759 ) ;
#7545 = ORIENTED_EDGE ( 'NONE', *, *, #96313, .F. ) ;
#7547 = AXIS2_PLACEMENT_3D ( 'NONE', #117648, #65995, #36562 ) ;
#7546 = AXIS2_PLACEMENT_3D ( 'NONE', #37634, #77533, #118752 ) ;
#7548 = CARTESIAN_POINT ( 'NONE',  ( 4.999999999999973355, 12.50000000000000000, -4.330127018922201643 ) ) ;
#7549 = FACE_OUTER_BOUND ( 'NONE', #55279, .T. ) ;
#7550 = DIRECTION ( 'NONE',  ( 0.000000000000000000, 1.000000000000000000, 0.000000000000000000 ) ) ;
#7551 = DIRECTION ( 'NONE',  ( 0.000000000000000000, 1.000000000000000000, 0.000000000000000000 ) ) ;
#7552 = DIRECTION ( 'NONE',  ( -0.000000000000000000, 1.000000000000000000, -0.000000000000000000 ) ) ;
#7553 = CONICAL_SURFACE ( 'NONE', #122502, 0.1000000000000002554, 0.003490658503988666988 ) ;
#7555 = EDGE_CURVE ( 'NONE', #106700, #53221, #84220, .T. ) ;
#7554 = CONICAL_SURFACE ( 'NONE', #1303, 0.1000000000000002554, 0.003490658503988666988 ) ;
#7556 = EDGE_LOOP ( 'NONE', ( #30673, #67472 ) ) ;
#7557 = ORIENTED_EDGE ( 'NONE', *, *, #89676, .T. ) ;
#7558 = VERTEX_POINT ( 'NONE', #74421 ) ;
#7559 = ORIENTED_EDGE ( 'NONE', *, *, #41169, .T. ) ;
#7560 = ORIENTED_EDGE ( 'NONE', *, *, #27902, .T. ) ;
#7561 = CARTESIAN_POINT ( 'NONE',  ( 9.149999999999918643, 2.500000000000000000, 2.265063509461097357 ) ) ;
#7562 = DIRECTION ( 'NONE',  ( 0.000000000000000000, 0.000000000000000000, -1.000000000000000000 ) ) ;
#7563 = ORIENTED_EDGE ( 'NONE', *, *, #71294, .T. ) ;
#7564 = FACE_BOUND ( 'NONE', #73346, .T. ) ;
#7565 = EDGE_CURVE ( 'NONE', #113013, #89246, #120590, .T. ) ;
#7566 = CARTESIAN_POINT ( 'NONE',  ( -2.900000000000029221, 2.500000000000000000, -0.6928203230275541413 ) ) ;
#7567 = DIRECTION ( 'NONE',  ( 0.000000000000000000, 0.000000000000000000, -1.000000000000000000 ) ) ;
#7568 = EDGE_CURVE ( 'NONE', #82944, #77871, #80894, .T. ) ;
#7569 = CARTESIAN_POINT ( 'NONE',  ( -9.350000000000006750, 2.500000000000000000, 1.718653347947321386 ) ) ;
#7570 = ADVANCED_FACE ( 'NONE', ( #42385 ), #72495, .T. ) ;
#7571 = DIRECTION ( 'NONE',  ( 0.000000000000000000, -0.000000000000000000, 1.000000000000000000 ) ) ;
#7572 = ADVANCED_FACE ( 'NONE', ( #122242 ), #35156, .T. ) ;
#7573 = CARTESIAN_POINT ( 'NONE',  ( 15.59999999999988951, 12.50000000000000000, -0.3464101615137783474 ) ) ;
#7574 = ADVANCED_FACE ( 'NONE', ( #112415 ), #16103, .T. ) ;
#7576 = ORIENTED_EDGE ( 'NONE', *, *, #113560, .T. ) ;
#7575 = CIRCLE ( 'NONE', #57772, 0.06509327318403745899 ) ;
#7577 = DIRECTION ( 'NONE',  ( -0.000000000000000000, -1.000000000000000000, -0.000000000000000000 ) ) ;
#7578 = VERTEX_POINT ( 'NONE', #105811 ) ;
#7579 = CONICAL_SURFACE ( 'NONE', #51519, 0.1000000000000002554, 0.003490658503988666988 ) ;
#7580 = ORIENTED_EDGE ( 'NONE', *, *, #119425, .T. ) ;
#7581 = VERTEX_POINT ( 'NONE', #37720 ) ;
#7582 = FACE_OUTER_BOUND ( 'NONE', #18545, .T. ) ;
#7583 = CARTESIAN_POINT ( 'NONE',  ( -7.900000000000014566, 2.500000000000000000, -4.330127018922201643 ) ) ;
#7584 = AXIS2_PLACEMENT_3D ( 'NONE', #66665, #127539, #28051 ) ;
#7585 = FACE_OUTER_BOUND ( 'NONE', #93493, .T. ) ;
#7586 = ORIENTED_EDGE ( 'NONE', *, *, #107788, .F. ) ;
#7587 = EDGE_CURVE ( 'NONE', #112225, #77376, #77624, .T. ) ;
#7588 = CARTESIAN_POINT ( 'NONE',  ( 10.61495711640361073, 2.500000000000000000, -8.020491764207555718 ) ) ;
#7589 = VECTOR ( 'NONE', #89520, 1000.000000000000000 ) ;
#7590 = CIRCLE ( 'NONE', #13845, 0.09999999999999982514 ) ;
#7591 = EDGE_CURVE ( 'NONE', #39666, #33436, #116900, .T. ) ;
#7592 = DIRECTION ( 'NONE',  ( -0.000000000000000000, 1.000000000000000000, -0.000000000000000000 ) ) ;
#7593 = EDGE_CURVE ( 'NONE', #88166, #6702, #56683, .T. ) ;
#7594 = AXIS2_PLACEMENT_3D ( 'NONE', #121698, #52972, #12391 ) ;
#7595 = DIRECTION ( 'NONE',  ( -4.274815082592931898E-19, -0.9999939076577903929, -0.003490651415223739937 ) ) ;
#7596 = CARTESIAN_POINT ( 'NONE',  ( 187.0260416670080588, -6.551208109652273848, -3.782341765625003571 ) ) ;
#7597 = CARTESIAN_POINT ( 'NONE',  ( -6.850000000000013856, 12.50000000000000000, 6.841600689897072485 ) ) ;
#7598 = CARTESIAN_POINT ( 'NONE',  ( 11.24999999999990585, 12.50000000000000000, 2.792790559304612064 ) ) ;
#7599 = CARTESIAN_POINT ( 'NONE',  ( 1.249999999999952482, 2.500000000000000000, -5.902370205355750521 ) ) ;
#7600 = ORIENTED_EDGE ( 'NONE', *, *, #101081, .F. ) ;
#7601 = DIRECTION ( 'NONE',  ( -0.000000000000000000, 1.000000000000000000, -0.000000000000000000 ) ) ;
#7602 = AXIS2_PLACEMENT_3D ( 'NONE', #18169, #58115, #98020 ) ;
#7603 = VERTEX_POINT ( 'NONE', #108384 ) ;
#7605 = CIRCLE ( 'NONE', #28552, 0.1000000000000002554 ) ;
#7604 = AXIS2_PLACEMENT_3D ( 'NONE', #103897, #121586, #52862 ) ;
#7606 = VERTEX_POINT ( 'NONE', #95349 ) ;
#7607 = CARTESIAN_POINT ( 'NONE',  ( 9.549999999999915445, 2.500000000000000000, -2.065063509461102065 ) ) ;
#7608 = CARTESIAN_POINT ( 'NONE',  ( -8.350000000000008527, 2.500000000000000000, 5.702370205355745014 ) ) ;
#7609 = DIRECTION ( 'NONE',  ( -4.274815082592931898E-19, -0.9999939076577903929, -0.003490651415223739937 ) ) ;
#7610 = ORIENTED_EDGE ( 'NONE', *, *, #41003, .T. ) ;
#7611 = ORIENTED_EDGE ( 'NONE', *, *, #102433, .T. ) ;
#7612 = CARTESIAN_POINT ( 'NONE',  ( 184.7812500006828031, 0.000000000000000000, 7.700000000000000178 ) ) ;
#7613 = CARTESIAN_POINT ( 'NONE',  ( -8.300000000000009592, 2.500000000000000000, 4.430127018922196847 ) ) ;
#7614 = LINE ( 'NONE', #47563, #115095 ) ;
#7615 = VERTEX_POINT ( 'NONE', #27891 ) ;
#7616 = ORIENTED_EDGE ( 'NONE', *, *, #93050, .T. ) ;
#7617 = DIRECTION ( 'NONE',  ( 0.000000000000000000, 0.000000000000000000, 1.000000000000000000 ) ) ;
#7618 = VERTEX_POINT ( 'NONE', #96612 ) ;
#7619 = CARTESIAN_POINT ( 'NONE',  ( 9.549999999999915445, 2.500000000000000000, 6.495190528383297135 ) ) ;
#7620 = LINE ( 'NONE', #66543, #53358 ) ;
#7621 = ORIENTED_EDGE ( 'NONE', *, *, #9785, .T. ) ;
#7622 = DIRECTION ( 'NONE',  ( 0.000000000000000000, 0.000000000000000000, -1.000000000000000000 ) ) ;
#7623 = DIRECTION ( 'NONE',  ( 0.000000000000000000, 1.000000000000000000, 0.000000000000000000 ) ) ;
#7624 = LINE ( 'NONE', #76388, #48880 ) ;
#7625 = EDGE_CURVE ( 'NONE', #75839, #49848, #108067, .T. ) ;
#7626 = CARTESIAN_POINT ( 'NONE',  ( -15.59999999999998010, 2.500000000000000000, -0.2464101615137759549 ) ) ;
#7627 = ORIENTED_EDGE ( 'NONE', *, *, #126383, .F. ) ;
#7628 = EDGE_CURVE ( 'NONE', #8482, #39568, #26600, .T. ) ;
#7629 = CARTESIAN_POINT ( 'NONE',  ( 9.149999999999920419, 2.500000000000000000, -5.902370205355750521 ) ) ;
#7630 = CIRCLE ( 'NONE', #101733, 0.06509327318403741736 ) ;
#7631 = VECTOR ( 'NONE', #92183, 1000.000000000000000 ) ;
#7632 = EDGE_CURVE ( 'NONE', #110466, #93340, #124803, .T. ) ;
#7633 = ORIENTED_EDGE ( 'NONE', *, *, #82253, .T. ) ;
#7634 = ORIENTED_EDGE ( 'NONE', *, *, #125670, .F. ) ;
#7635 = PLANE ( 'NONE',  #52064 ) ;
#7636 = PLANE ( 'NONE',  #26087 ) ;
#7637 = PLANE ( 'NONE',  #105522 ) ;
#7638 = CARTESIAN_POINT ( 'NONE',  ( -13.54999999999999005, 2.500000000000000000, 2.611473670974877148 ) ) ;
#7639 = CARTESIAN_POINT ( 'NONE',  ( -6.050000000000018474, 12.50000000000000000, 2.446380397790835826 ) ) ;
#7640 = EDGE_CURVE ( 'NONE', #17235, #14780, #27239, .T. ) ;
#7642 = CARTESIAN_POINT ( 'NONE',  ( 3.349999999999942801, 2.500000000000000000, 2.857883832488649301 ) ) ;
#7641 = VECTOR ( 'NONE', #9938, 1000.000000000000000 ) ;
#7643 = PLANE ( 'NONE',  #107351 ) ;
#7644 = DIRECTION ( 'NONE',  ( -0.000000000000000000, 1.000000000000000000, -0.000000000000000000 ) ) ;
#7645 = FACE_OUTER_BOUND ( 'NONE', #33920, .T. ) ;
#7646 = LINE ( 'NONE', #106505, #77231 ) ;
#7648 = VECTOR ( 'NONE', #100285, 1000.000000000000000 ) ;
#7647 = CONICAL_SURFACE ( 'NONE', #112221, 0.1000000000000002554, 0.003490658503988666988 ) ;
#7649 = CONICAL_SURFACE ( 'NONE', #59921, 0.09999999999999982514, 0.003490658503988666988 ) ;
#7650 = ORIENTED_EDGE ( 'NONE', *, *, #75133, .F. ) ;
#7651 = FACE_OUTER_BOUND ( 'NONE', #7016, .T. ) ;
#7652 = DIRECTION ( 'NONE',  ( 0.000000000000000000, 0.000000000000000000, 1.000000000000000000 ) ) ;
#7653 = CARTESIAN_POINT ( 'NONE',  ( -3.100000000000028955, 2.500000000000000000, 4.576537180435972019 ) ) ;
#7654 = ADVANCED_FACE ( 'NONE', ( #76994 ), #85523, .T. ) ;
#7655 = DIRECTION ( 'NONE',  ( 0.000000000000000000, -0.000000000000000000, 1.000000000000000000 ) ) ;
#7656 = DIRECTION ( 'NONE',  ( 0.000000000000000000, 0.000000000000000000, -1.000000000000000000 ) ) ;
#7657 = ORIENTED_EDGE ( 'NONE', *, *, #101344, .F. ) ;
#7658 = CARTESIAN_POINT ( 'NONE',  ( -0.8000000000000315747, 12.50000000000000000, -0.06509327318403743123 ) ) ;
#7659 = PLANE ( 'NONE',  #76344 ) ;
#7661 = EDGE_LOOP ( 'NONE', ( #75281, #40433 ) ) ;
#7660 = CARTESIAN_POINT ( 'NONE',  ( -6.650000000000019007, 12.50000000000000000, -1.472243186433550122 ) ) ;
#7662 = ORIENTED_EDGE ( 'NONE', *, *, #59030, .F. ) ;
#7663 = AXIS2_PLACEMENT_3D ( 'NONE', #107574, #17892, #89854 ) ;
#7665 = VERTEX_POINT ( 'NONE', #67141 ) ;
#7664 = EDGE_CURVE ( 'NONE', #55928, #126709, #89290, .T. ) ;
#7666 = ORIENTED_EDGE ( 'NONE', *, *, #4953, .T. ) ;
#7667 = EDGE_LOOP ( 'NONE', ( #12501, #49577, #108710, #72637 ) ) ;
#7668 = DIRECTION ( 'NONE',  ( 0.000000000000000000, 1.000000000000000000, 0.000000000000000000 ) ) ;
#7669 = ADVANCED_FACE ( 'NONE', ( #118208 ), #122739, .T. ) ;
#7670 = CIRCLE ( 'NONE', #16073, 0.09999999999999982514 ) ;
#7671 = FACE_OUTER_BOUND ( 'NONE', #1547, .T. ) ;
#7672 = DIRECTION ( 'NONE',  ( 0.000000000000000000, 1.000000000000000000, 0.000000000000000000 ) ) ;
#7673 = AXIS2_PLACEMENT_3D ( 'NONE', #84527, #123172, #124458 ) ;
#7674 = CARTESIAN_POINT ( 'NONE',  ( 12.49999999999990408, 2.500000000000000000, 5.022947341949748790 ) ) ;
#7675 = VERTEX_POINT ( 'NONE', #86810 ) ;
#7676 = CONICAL_SURFACE ( 'NONE', #9838, 0.1000000000000002554, 0.003490658503988666988 ) ;
#7677 = CARTESIAN_POINT ( 'NONE',  ( -12.89999999999999147, 2.500000000000000000, 5.122947341949749323 ) ) ;
#7678 = EDGE_LOOP ( 'NONE', ( #114807, #27182, #2412, #43129 ) ) ;
#7679 = CARTESIAN_POINT ( 'NONE',  ( 26.76314062981183639, -1.072173157152068734, -4.440523076946065295 ) ) ;
#7680 = CARTESIAN_POINT ( 'NONE',  ( 5.199999999999935341, 2.500000000000000000, -0.2464101615137783419 ) ) ;
#7681 = CARTESIAN_POINT ( 'NONE',  ( 195.5000000000000000, 0.000000000000000000, 0.000000000000000000 ) ) ;
#7682 = DIRECTION ( 'NONE',  ( 0.000000000000000000, 0.000000000000000000, 1.000000000000000000 ) ) ;
#7683 = AXIS2_PLACEMENT_3D ( 'NONE', #108061, #18393, #58341 ) ;
#7684 = EDGE_CURVE ( 'NONE', #101675, #28068, #25967, .T. ) ;
#7685 = DIRECTION ( 'NONE',  ( 0.000000000000000000, 1.000000000000000000, 0.000000000000000000 ) ) ;
#7686 = CONICAL_SURFACE ( 'NONE', #78734, 0.1000000000000002554, 0.003490658503988666988 ) ;
#7687 = VERTEX_POINT ( 'NONE', #56049 ) ;
#7689 = AXIS2_PLACEMENT_3D ( 'NONE', #81800, #61542, #41265 ) ;
#7688 = CIRCLE ( 'NONE', #78833, 0.06509327318403745899 ) ;
#7690 = ORIENTED_EDGE ( 'NONE', *, *, #52984, .T. ) ;
#7691 = EDGE_LOOP ( 'NONE', ( #54018, #124313 ) ) ;
#7692 = ORIENTED_EDGE ( 'NONE', *, *, #107796, .T. ) ;
#7693 = DIRECTION ( 'NONE',  ( 0.000000000000000000, 1.000000000000000000, 0.000000000000000000 ) ) ;
#7694 = LINE ( 'NONE', #27994, #45682 ) ;
#7695 = EDGE_CURVE ( 'NONE', #114560, #87328, #57354, .T. ) ;
#7696 = PLANE ( 'NONE',  #98447 ) ;
#7697 = FACE_BOUND ( 'NONE', #18858, .T. ) ;
#7698 = DIRECTION ( 'NONE',  ( 0.000000000000000000, 0.000000000000000000, -1.000000000000000000 ) ) ;
#7699 = CARTESIAN_POINT ( 'NONE',  ( -0.4500000000000397571, 2.500000000000000000, -2.165063509461101710 ) ) ;
#7700 = CARTESIAN_POINT ( 'NONE',  ( 0.8499999999999553468, 2.500000000000000000, -2.957883832488653830 ) ) ;
#7701 = DIRECTION ( 'NONE',  ( 0.000000000000000000, 0.000000000000000000, 1.000000000000000000 ) ) ;
#7702 = CARTESIAN_POINT ( 'NONE',  ( 183.9218750003414016, 0.000000000000000000, 7.564683531250000925 ) ) ;
#7703 = DIRECTION ( 'NONE',  ( -0.000000000000000000, -1.000000000000000000, -0.000000000000000000 ) ) ;
#7704 = AXIS2_PLACEMENT_3D ( 'NONE', #128030, #45616, #95993 ) ;
#7705 = CARTESIAN_POINT ( 'NONE',  ( -7.499999999999980460, 2.500000000000000000, -4.230127018922201998 ) ) ;
#7706 = LINE ( 'NONE', #105927, #118366 ) ;
#7707 = ADVANCED_FACE ( 'NONE', ( #6291 ), #38379, .T. ) ;
#7708 = ORIENTED_EDGE ( 'NONE', *, *, #95264, .F. ) ;
#7709 = ORIENTED_EDGE ( 'NONE', *, *, #26637, .T. ) ;
#7710 = EDGE_LOOP ( 'NONE', ( #124299, #97535 ) ) ;
#7711 = ORIENTED_EDGE ( 'NONE', *, *, #114273, .F. ) ;
#7712 = CARTESIAN_POINT ( 'NONE',  ( -15.39999999999997904, 12.50000000000000000, -0.6277270498435144619 ) ) ;
#7713 = FACE_BOUND ( 'NONE', #80345, .T. ) ;
#7714 = DIRECTION ( 'NONE',  ( 0.000000000000000000, 1.000000000000000000, 0.000000000000000000 ) ) ;
#7715 = EDGE_CURVE ( 'NONE', #75374, #83523, #46239, .T. ) ;
#7716 = CONICAL_SURFACE ( 'NONE', #80904, 0.09999999999999999167, 0.003490658503988666988 ) ;
#7717 = AXIS2_PLACEMENT_3D ( 'NONE', #22831, #100089, #31359 ) ;
#7718 = EDGE_LOOP ( 'NONE', ( #64382, #57063, #46579, #48442 ) ) ;
#7719 = EDGE_CURVE ( 'NONE', #50950, #119162, #99764, .T. ) ;
#7720 = DIRECTION ( 'NONE',  ( 0.000000000000000000, 0.000000000000000000, 1.000000000000000000 ) ) ;
#7721 = EDGE_CURVE ( 'NONE', #69080, #67022, #66299, .T. ) ;
#7722 = CARTESIAN_POINT ( 'NONE',  ( 6.649999999999927525, 12.50000000000000000, 2.165063509461097713 ) ) ;
#7723 = EDGE_CURVE ( 'NONE', #40625, #37050, #99672, .T. ) ;
#7724 = DIRECTION ( 'NONE',  ( -0.000000000000000000, -1.000000000000000000, -0.000000000000000000 ) ) ;
#7725 = EDGE_CURVE ( 'NONE', #79666, #122612, #59986, .T. ) ;
#7726 = ORIENTED_EDGE ( 'NONE', *, *, #20464, .T. ) ;
#7727 = DIRECTION ( 'NONE',  ( -0.000000000000000000, 1.000000000000000000, -0.000000000000000000 ) ) ;
#7728 = DIRECTION ( 'NONE',  ( 0.000000000000000000, 0.000000000000000000, -1.000000000000000000 ) ) ;
#7730 = VECTOR ( 'NONE', #61465, 1000.000000000000000 ) ;
#7729 = AXIS2_PLACEMENT_3D ( 'NONE', #73361, #93657, #113283 ) ;
#7731 = ADVANCED_FACE ( 'NONE', ( #19347 ), #49490, .T. ) ;
#7732 = ORIENTED_EDGE ( 'NONE', *, *, #7715, .F. ) ;
#7733 = DIRECTION ( 'NONE',  ( 0.000000000000000000, -0.9999939076577903929, 0.003490651415223739937 ) ) ;
#7734 = EDGE_CURVE ( 'NONE', #87808, #123263, #74710, .T. ) ;
#7735 = DIRECTION ( 'NONE',  ( 0.000000000000000000, 0.000000000000000000, 1.000000000000000000 ) ) ;
#7736 = ADVANCED_FACE ( 'NONE', ( #129346 ), #88749, .F. ) ;
#7738 = CONICAL_SURFACE ( 'NONE', #24480, 0.1000000000000000472, 0.003490658503988666988 ) ;
#7737 = CIRCLE ( 'NONE', #43279, 0.09999999999999982514 ) ;
#7739 = EDGE_CURVE ( 'NONE', #126164, #10889, #97689, .T. ) ;
#7740 = ORIENTED_EDGE ( 'NONE', *, *, #62978, .T. ) ;
#7741 = CIRCLE ( 'NONE', #43282, 0.06509327318403745899 ) ;
#7742 = CARTESIAN_POINT ( 'NONE',  ( 14.39999999999989555, 2.500000000000000000, -0.2464101615137782308 ) ) ;
#7743 = EDGE_CURVE ( 'NONE', #29933, #45761, #83139, .T. ) ;
#7744 = CARTESIAN_POINT ( 'NONE',  ( 8.349999999999919709, 2.500000000000000000, 5.802370205355744659 ) ) ;
#7745 = ORIENTED_EDGE ( 'NONE', *, *, #67387, .T. ) ;
#7746 = LINE ( 'NONE', #69906, #5513 ) ;
#7747 = VERTEX_POINT ( 'NONE', #118849 ) ;
#7748 = ORIENTED_EDGE ( 'NONE', *, *, #55762, .F. ) ;
#7749 = DIRECTION ( 'NONE',  ( 0.000000000000000000, 0.000000000000000000, 1.000000000000000000 ) ) ;
#7750 = ADVANCED_FACE ( 'NONE', ( #59313 ), #91434, .T. ) ;
#7751 = ORIENTED_EDGE ( 'NONE', *, *, #104056, .T. ) ;
#7752 = DIRECTION ( 'NONE',  ( 0.000000000000000000, 0.000000000000000000, 1.000000000000000000 ) ) ;
#7753 = FACE_BOUND ( 'NONE', #23998, .T. ) ;
#7754 = EDGE_LOOP ( 'NONE', ( #70761, #97724, #60995, #84845 ) ) ;
#7755 = CARTESIAN_POINT ( 'NONE',  ( 111.3044611531193766, 6.721044513813564159, 3.765782231328828722 ) ) ;
#7756 = ORIENTED_EDGE ( 'NONE', *, *, #35102, .F. ) ;
#7757 = DIRECTION ( 'NONE',  ( -4.274815082592931898E-19, -0.9999939076577903929, -0.003490651415223739937 ) ) ;
#7758 = CARTESIAN_POINT ( 'NONE',  ( -6.900000000000019007, 2.500000000000000000, -4.083716857408426826 ) ) ;
#7759 = CARTESIAN_POINT ( 'NONE',  ( 17.49862860983209956, 2.500000000000000000, 4.081131818001135336 ) ) ;
#7760 = CARTESIAN_POINT ( 'NONE',  ( 10.39999999999991509, 2.500000000000000000, 0.6928203230275494784 ) ) ;
#7762 = CIRCLE ( 'NONE', #70554, 0.06509327318403745899 ) ;
#7761 = DIRECTION ( 'NONE',  ( 7.228014483236698281E-17, 0.000000000000000000, 1.000000000000000000 ) ) ;
#7763 = AXIS2_PLACEMENT_3D ( 'NONE', #114648, #103562, #84556 ) ;
#7764 = VERTEX_POINT ( 'NONE', #57121 ) ;
#7765 = EDGE_LOOP ( 'NONE', ( #86108, #91422 ) ) ;
#7766 = CARTESIAN_POINT ( 'NONE',  ( 4.999999999999936939, 2.500000000000000000, -3.637306695894650055 ) ) ;
#7767 = CIRCLE ( 'NONE', #126917, 0.09999999999999999167 ) ;
#7768 = DIRECTION ( 'NONE',  ( -0.000000000000000000, 1.000000000000000000, -0.000000000000000000 ) ) ;
#7769 = DIRECTION ( 'NONE',  ( 0.000000000000000000, 1.000000000000000000, 0.000000000000000000 ) ) ;
#7771 = EDGE_LOOP ( 'NONE', ( #62878, #118701, #54082, #59593 ) ) ;
#7770 = VERTEX_POINT ( 'NONE', #17841 ) ;
#7772 = EDGE_LOOP ( 'NONE', ( #121306, #69307 ) ) ;
#7773 = DIRECTION ( 'NONE',  ( -0.000000000000000000, 1.000000000000000000, -0.000000000000000000 ) ) ;
#7774 = AXIS2_PLACEMENT_3D ( 'NONE', #74244, #114171, #14652 ) ;
#7775 = AXIS2_PLACEMENT_3D ( 'NONE', #3714, #71826, #44281 ) ;
#7776 = CARTESIAN_POINT ( 'NONE',  ( 7.099999999999928590, 2.500000000000000000, 4.430127018922196847 ) ) ;
#7777 = DIRECTION ( 'NONE',  ( 0.000000000000000000, -0.9999939076577903929, 0.003490651415223739937 ) ) ;
#7778 = VECTOR ( 'NONE', #96864, 1000.000000000000000 ) ;
#7779 = APPLICATION_PROTOCOL_DEFINITION ( 'draft international standard', 'automotive_design', 1998, #2834 ) ;
#7780 = FACE_OUTER_BOUND ( 'NONE', #125377, .T. ) ;
#7781 = PLANE ( 'NONE',  #75263 ) ;
#7782 = DIRECTION ( 'NONE',  ( 0.000000000000000000, 0.000000000000000000, 1.000000000000000000 ) ) ;
#7783 = CARTESIAN_POINT ( 'NONE',  ( 8.749999999999918288, 2.500000000000000000, -1.472243186433550122 ) ) ;
#7784 = CARTESIAN_POINT ( 'NONE',  ( -6.850000000000013856, 2.500000000000000000, 6.841600689897072485 ) ) ;
#7785 = AXIS2_PLACEMENT_3D ( 'NONE', #89559, #58816, #88921 ) ;
#7786 = DIRECTION ( 'NONE',  ( -0.000000000000000000, 1.000000000000000000, -0.000000000000000000 ) ) ;
#7787 = VERTEX_POINT ( 'NONE', #38812 ) ;
#7788 = VERTEX_POINT ( 'NONE', #78054 ) ;
#7789 = EDGE_CURVE ( 'NONE', #74230, #125138, #116466, .T. ) ;
#7791 = CIRCLE ( 'NONE', #18261, 0.06509327318403745899 ) ;
#7790 = VECTOR ( 'NONE', #127889, 1000.000000000000000 ) ;
#7792 = ADVANCED_FACE ( 'NONE', ( #98327 ), #37074, .T. ) ;
#7793 = DIRECTION ( 'NONE',  ( 0.000000000000000000, -0.000000000000000000, 1.000000000000000000 ) ) ;
#7794 = VERTEX_POINT ( 'NONE', #26395 ) ;
#7795 = ORIENTED_EDGE ( 'NONE', *, *, #2117, .T. ) ;
#7796 = DIRECTION ( 'NONE',  ( 0.000000000000000000, 0.000000000000000000, -1.000000000000000000 ) ) ;
#7797 = DIRECTION ( 'NONE',  ( -0.000000000000000000, 1.000000000000000000, -0.000000000000000000 ) ) ;
#7798 = CARTESIAN_POINT ( 'NONE',  ( 2.500000000000002220, 1.761799387799148686, -9.999999999999998224 ) ) ;
#7799 = EDGE_CURVE ( 'NONE', #99110, #89337, #110223, .T. ) ;
#7800 = DIRECTION ( 'NONE',  ( -0.000000000000000000, 1.000000000000000000, -0.000000000000000000 ) ) ;
#7801 = LINE ( 'NONE', #70437, #17261 ) ;
#7802 = DIRECTION ( 'NONE',  ( -0.000000000000000000, -1.000000000000000000, -0.000000000000000000 ) ) ;
#7803 = DIRECTION ( 'NONE',  ( 0.000000000000000000, -0.9999939076577903929, 0.003490651415223739937 ) ) ;
#7804 = ORIENTED_EDGE ( 'NONE', *, *, #85529, .T. ) ;
#7805 = DIRECTION ( 'NONE',  ( -0.000000000000000000, -1.000000000000000000, -0.000000000000000000 ) ) ;
#7806 = VECTOR ( 'NONE', #28971, 1000.000000000000000 ) ;
#7807 = CARTESIAN_POINT ( 'NONE',  ( -4.600000000000028066, 2.500000000000000000, -5.022947341949754119 ) ) ;
#7808 = ORIENTED_EDGE ( 'NONE', *, *, #52772, .T. ) ;
#7809 = VERTEX_POINT ( 'NONE', #108153 ) ;
#7810 = VERTEX_POINT ( 'NONE', #76777 ) ;
#7811 = ORIENTED_EDGE ( 'NONE', *, *, #5263, .F. ) ;
#7812 = CARTESIAN_POINT ( 'NONE',  ( 9.149999999999916866, 2.500000000000000000, 5.802370205355744659 ) ) ;
#7813 = FACE_OUTER_BOUND ( 'NONE', #107584, .T. ) ;
#7814 = ORIENTED_EDGE ( 'NONE', *, *, #73509, .T. ) ;
#7815 = CIRCLE ( 'NONE', #93599, 0.1000000000000002554 ) ;
#7816 = DIRECTION ( 'NONE',  ( 0.000000000000000000, 1.000000000000000000, 0.000000000000000000 ) ) ;
#7818 = DIRECTION ( 'NONE',  ( 0.000000000000000000, 0.000000000000000000, 1.000000000000000000 ) ) ;
#7817 = AXIS2_PLACEMENT_3D ( 'NONE', #106836, #17143, #76108 ) ;
#7819 = DIRECTION ( 'NONE',  ( 0.000000000000000000, 0.000000000000000000, -1.000000000000000000 ) ) ;
#7820 = ORIENTED_EDGE ( 'NONE', *, *, #112991, .T. ) ;
#7821 = CARTESIAN_POINT ( 'NONE',  ( 11.64999999999990798, 2.500000000000000000, 7.288010851410849256 ) ) ;
#7823 = VECTOR ( 'NONE', #64661, 1000.000000000000000 ) ;
#7822 = CONICAL_SURFACE ( 'NONE', #32901, 0.09999999999999982514, 0.003490658503988666988 ) ;
#7824 = DIRECTION ( 'NONE',  ( 0.000000000000000000, 1.000000000000000000, 0.000000000000000000 ) ) ;
#7825 = EDGE_CURVE ( 'NONE', #60531, #96053, #60067, .T. ) ;
#7826 = ORIENTED_EDGE ( 'NONE', *, *, #51694, .T. ) ;
#7827 = AXIS2_PLACEMENT_3D ( 'NONE', #30993, #121280, #61736 ) ;
#7828 = EDGE_LOOP ( 'NONE', ( #112303, #117127, #76563, #58560 ) ) ;
#7829 = VERTEX_POINT ( 'NONE', #66300 ) ;
#7830 = DIRECTION ( 'NONE',  ( -0.000000000000000000, 1.000000000000000000, -0.000000000000000000 ) ) ;
#7831 = EDGE_CURVE ( 'NONE', #78396, #39804, #87219, .T. ) ;
#7832 = AXIS2_PLACEMENT_3D ( 'NONE', #64497, #54039, #74324 ) ;
#7833 = CARTESIAN_POINT ( 'NONE',  ( -9.150000000000009237, 12.50000000000000000, -6.495190528383297135 ) ) ;
#7834 = CIRCLE ( 'NONE', #22453, 0.06509327318403745899 ) ;
#7836 = ORIENTED_EDGE ( 'NONE', *, *, #64113, .T. ) ;
#7835 = ADVANCED_FACE ( 'NONE', ( #87220 ), #17165, .T. ) ;
#7837 = FACE_OUTER_BOUND ( 'NONE', #25609, .T. ) ;
#7838 = CARTESIAN_POINT ( 'NONE',  ( -5.000000000000023093, 2.500000000000000000, 5.122947341949749323 ) ) ;
#7839 = FACE_OUTER_BOUND ( 'NONE', #42762, .T. ) ;
#7840 = CARTESIAN_POINT ( 'NONE',  ( 6.899999999999928413, 2.500000000000000000, -4.676537180435977881 ) ) ;
#7841 = ORIENTED_EDGE ( 'NONE', *, *, #104007, .F. ) ;
#7842 = AXIS2_PLACEMENT_3D ( 'NONE', #49905, #19789, #101567 ) ;
#7843 = DIRECTION ( 'NONE',  ( 0.000000000000000000, 1.000000000000000000, 0.000000000000000000 ) ) ;
#7844 = AXIS2_PLACEMENT_3D ( 'NONE', #57198, #46095, #7440 ) ;
#7845 = VERTEX_POINT ( 'NONE', #127176 ) ;
#7846 = ORIENTED_EDGE ( 'NONE', *, *, #34039, .T. ) ;
#7847 = FACE_OUTER_BOUND ( 'NONE', #27124, .T. ) ;
#7848 = ADVANCED_FACE ( 'NONE', ( #58433 ), #77413, .T. ) ;
#7849 = LINE ( 'NONE', #96225, #96125 ) ;
#7850 = FACE_BOUND ( 'NONE', #70360, .T. ) ;
#7851 = CIRCLE ( 'NONE', #108209, 0.1000000000000002554 ) ;
#7852 = CARTESIAN_POINT ( 'NONE',  ( 186.1562500006828031, 8.891194145520236347, 5.444286225454521982E-16 ) ) ;
#7853 = DIRECTION ( 'NONE',  ( 1.000000000000000000, -0.000000000000000000, -0.000000000000000000 ) ) ;
#7854 = CONICAL_SURFACE ( 'NONE', #41340, 0.1000000000000000472, 0.003490658503988666988 ) ;
#7855 = CARTESIAN_POINT ( 'NONE',  ( 2.499999999999983569, 2.500000000000000000, -4.330127018922201643 ) ) ;
#7856 = AXIS2_PLACEMENT_3D ( 'NONE', #55339, #63869, #14103 ) ;
#7857 = ORIENTED_EDGE ( 'NONE', *, *, #70093, .F. ) ;
#7858 = DIRECTION ( 'NONE',  ( 0.000000000000000000, 0.000000000000000000, -1.000000000000000000 ) ) ;
#7859 = CARTESIAN_POINT ( 'NONE',  ( 11.44999999999990870, 12.50000000000000000, -1.818653347947326138 ) ) ;
#7861 = DIRECTION ( 'NONE',  ( -0.000000000000000000, 1.000000000000000000, -0.000000000000000000 ) ) ;
#7860 = AXIS2_PLACEMENT_3D ( 'NONE', #123200, #53171, #62348 ) ;
#7863 = FACE_OUTER_BOUND ( 'NONE', #105953, .T. ) ;
#7862 = CONICAL_SURFACE ( 'NONE', #49756, 0.09999999999999982514, 0.003490658503988666988 ) ;
#7864 = ORIENTED_EDGE ( 'NONE', *, *, #100783, .T. ) ;
#7865 = CARTESIAN_POINT ( 'NONE',  ( 14.59999999999989484, 12.50000000000000000, 0.6928203230275494784 ) ) ;
#7866 = VECTOR ( 'NONE', #56770, 1000.000000000000000 ) ;
#7867 = CARTESIAN_POINT ( 'NONE',  ( -6.050000000000022027, 2.500000000000000000, -6.248780366869526759 ) ) ;
#7868 = ORIENTED_EDGE ( 'NONE', *, *, #48861, .F. ) ;
#7869 = ORIENTED_EDGE ( 'NONE', *, *, #56966, .T. ) ;
#7870 = CARTESIAN_POINT ( 'NONE',  ( 5.599999999999931255, 2.500000000000000000, 4.083716857408420609 ) ) ;
#7871 = AXIS2_PLACEMENT_3D ( 'NONE', #5029, #25309, #125460 ) ;
#7872 = CARTESIAN_POINT ( 'NONE',  ( -11.44999999999999929, 12.50000000000000000, -1.753560074763284682 ) ) ;
#7873 = FACE_BOUND ( 'NONE', #28917, .T. ) ;
#7874 = FACE_OUTER_BOUND ( 'NONE', #93186, .T. ) ;
#7875 = ADVANCED_FACE ( 'NONE', ( #56468 ), #95640, .T. ) ;
#7877 = VECTOR ( 'NONE', #127162, 1000.000000000000000 ) ;
#7876 = CIRCLE ( 'NONE', #58077, 0.09999999999999999167 ) ;
#7878 = EDGE_LOOP ( 'NONE', ( #119565, #32451, #13461, #49508 ) ) ;
#7879 = DIRECTION ( 'NONE',  ( 0.000000000000000000, 0.000000000000000000, -1.000000000000000000 ) ) ;
#7880 = ORIENTED_EDGE ( 'NONE', *, *, #71614, .T. ) ;
#7881 = VERTEX_POINT ( 'NONE', #106854 ) ;
#7882 = CARTESIAN_POINT ( 'NONE',  ( 17.37282530749029874, 0.4689596142739324014, -5.357821376857557105 ) ) ;
#7883 = EDGE_CURVE ( 'NONE', #60096, #67339, #3609, .T. ) ;
#7884 = CARTESIAN_POINT ( 'NONE',  ( 184.0468750003414300, -8.734944146203032389, -1.604583208406768146E-15 ) ) ;
#7885 = EDGE_CURVE ( 'NONE', #68909, #45780, #78721, .T. ) ;
#7886 = EDGE_LOOP ( 'NONE', ( #35639, #22532 ) ) ;
#7887 = DIRECTION ( 'NONE',  ( 0.000000000000000000, -0.9999939076577903929, 0.003490651415223739937 ) ) ;
#7888 = CARTESIAN_POINT ( 'NONE',  ( -14.14999999999998614, 12.50000000000000000, 1.472243186433549456 ) ) ;
#7889 = EDGE_CURVE ( 'NONE', #93617, #102522, #43437, .T. ) ;
#7890 = ADVANCED_FACE ( 'NONE', ( #19111 ), #39242, .T. ) ;
#7891 = CARTESIAN_POINT ( 'NONE',  ( 8.349999999999919709, 12.50000000000000000, -2.165063509461101710 ) ) ;
#7892 = EDGE_CURVE ( 'NONE', #53227, #2985, #60161, .T. ) ;
#7893 = DIRECTION ( 'NONE',  ( 0.000000000000000000, 0.000000000000000000, -1.000000000000000000 ) ) ;
#7894 = VERTEX_POINT ( 'NONE', #8017 ) ;
#7895 = EDGE_CURVE ( 'NONE', #43342, #125999, #127800, .T. ) ;
#7896 = DIRECTION ( 'NONE',  ( 0.000000000000000000, 0.000000000000000000, -1.000000000000000000 ) ) ;
#7897 = DIRECTION ( 'NONE',  ( -0.000000000000000000, 1.000000000000000000, -0.000000000000000000 ) ) ;
#7898 = LINE ( 'NONE', #129004, #67890 ) ;
#7899 = VERTEX_POINT ( 'NONE', #46667 ) ;
#7900 = CARTESIAN_POINT ( 'NONE',  ( -8.550000000000013145, 2.500000000000000000, 2.611473670974873151 ) ) ;
#7901 = VERTEX_POINT ( 'NONE', #85924 ) ;
#7902 = CARTESIAN_POINT ( 'NONE',  ( 7.099999999999925926, 2.500000000000000000, 0.6928203230275494784 ) ) ;
#7903 = ADVANCED_FACE ( 'NONE', ( #86580 ), #126520, .T. ) ;
#7904 = EDGE_LOOP ( 'NONE', ( #64232, #66812, #57160, #91312 ) ) ;
#7905 = LINE ( 'NONE', #118506, #44866 ) ;
#7906 = CARTESIAN_POINT ( 'NONE',  ( 2.899999999999944844, 2.500000000000000000, 5.022947341949748790 ) ) ;
#7907 = AXIS2_PLACEMENT_3D ( 'NONE', #106151, #104215, #85217 ) ;
#7908 = DIRECTION ( 'NONE',  ( 0.000000000000000000, -0.000000000000000000, 1.000000000000000000 ) ) ;
#7909 = DIRECTION ( 'NONE',  ( -0.000000000000000000, 1.000000000000000000, -0.000000000000000000 ) ) ;
#7910 = VERTEX_POINT ( 'NONE', #125575 ) ;
#7911 = CARTESIAN_POINT ( 'NONE',  ( 1.899999999999951283, 2.500000000000000000, -3.983716857408426293 ) ) ;
#7912 = CARTESIAN_POINT ( 'NONE',  ( -9.350000000000006750, 2.500000000000000000, 1.718653347947321386 ) ) ;
#7913 = CARTESIAN_POINT ( 'NONE',  ( 184.9427083336747160, -6.551208109652278289, 3.782341765624995134 ) ) ;
#7914 = DIRECTION ( 'NONE',  ( 0.000000000000000000, 0.000000000000000000, -1.000000000000000000 ) ) ;
#7915 = FACE_OUTER_BOUND ( 'NONE', #17874, .T. ) ;
#7916 = CIRCLE ( 'NONE', #47648, 0.06509327318403745899 ) ;
#7917 = ORIENTED_EDGE ( 'NONE', *, *, #4298, .F. ) ;
#7918 = CONICAL_SURFACE ( 'NONE', #81105, 0.1000000000000002554, 0.003490658503988666988 ) ;
#7920 = VERTEX_POINT ( 'NONE', #26746 ) ;
#7919 = AXIS2_PLACEMENT_3D ( 'NONE', #40799, #2126, #121267 ) ;
#7921 = PLANE ( 'NONE',  #49163 ) ;
#7922 = VERTEX_POINT ( 'NONE', #45749 ) ;
#7923 = CARTESIAN_POINT ( 'NONE',  ( 8.149999999999923972, 2.500000000000000000, -6.048780366869526581 ) ) ;
#7925 = VERTEX_POINT ( 'NONE', #6422 ) ;
#7924 = EDGE_LOOP ( 'NONE', ( #31434, #85745, #18389, #46290 ) ) ;
#7926 = VERTEX_POINT ( 'NONE', #37224 ) ;
#7927 = DIRECTION ( 'NONE',  ( 0.000000000000000000, 0.000000000000000000, 1.000000000000000000 ) ) ;
#7929 = PLANE ( 'NONE',  #44298 ) ;
#7928 = CONICAL_SURFACE ( 'NONE', #60189, 0.1000000000000002554, 0.003490658503988666988 ) ;
#7930 = CARTESIAN_POINT ( 'NONE',  ( 15.59999999999988951, 12.50000000000000000, 0.4115034346978109769 ) ) ;
#7931 = FILL_AREA_STYLE ('',( #98896 ) ) ;
#7932 = DIRECTION ( 'NONE',  ( 0.000000000000000000, 1.000000000000000000, 0.000000000000000000 ) ) ;
#7933 = DIRECTION ( 'NONE',  ( 0.000000000000000000, -0.000000000000000000, 1.000000000000000000 ) ) ;
#7934 = FACE_OUTER_BOUND ( 'NONE', #61648, .T. ) ;
#7935 = AXIS2_PLACEMENT_3D ( 'NONE', #125341, #124702, #46789 ) ;
#7936 = DIRECTION ( 'NONE',  ( 0.000000000000000000, 0.000000000000000000, -1.000000000000000000 ) ) ;
#7937 = ORIENTED_EDGE ( 'NONE', *, *, #119189, .F. ) ;
#7938 = CARTESIAN_POINT ( 'NONE',  ( -2.300000000000033573, 2.500000000000000000, 0.4464101615137735513 ) ) ;
#7939 = VERTEX_POINT ( 'NONE', #46370 ) ;
#7940 = VECTOR ( 'NONE', #18817, 1000.000000000000000 ) ;
#7941 = ORIENTED_EDGE ( 'NONE', *, *, #90504, .F. ) ;
#7942 = ORIENTED_EDGE ( 'NONE', *, *, #102735, .T. ) ;
#7943 = EDGE_CURVE ( 'NONE', #67339, #114052, #45109, .T. ) ;
#7944 = ORIENTED_EDGE ( 'NONE', *, *, #113565, .T. ) ;
#7945 =( GEOMETRIC_REPRESENTATION_CONTEXT ( 3 ) GLOBAL_UNCERTAINTY_ASSIGNED_CONTEXT ( ( #105561 ) ) GLOBAL_UNIT_ASSIGNED_CONTEXT ( ( #92451, #81986, #121922 ) ) REPRESENTATION_CONTEXT ( 'NONE', 'WORKASPACE' ) );
#7946 = DIRECTION ( 'NONE',  ( 0.000000000000000000, 0.000000000000000000, -1.000000000000000000 ) ) ;
#7947 = ORIENTED_EDGE ( 'NONE', *, *, #74553, .F. ) ;
#7948 = VERTEX_POINT ( 'NONE', #113845 ) ;
#7949 = AXIS2_PLACEMENT_3D ( 'NONE', #111442, #30342, #91174 ) ;
#7950 = AXIS2_PLACEMENT_3D ( 'NONE', #38051, #129036, #119187 ) ;
#7951 = ADVANCED_FACE ( 'NONE', ( #66653 ), #89389, .T. ) ;
#7952 = DIRECTION ( 'NONE',  ( 0.000000000000000000, 0.000000000000000000, 1.000000000000000000 ) ) ;
#7954 = CONICAL_SURFACE ( 'NONE', #122897, 0.1000000000000000472, 0.003490658503988666988 ) ;
#7953 = CARTESIAN_POINT ( 'NONE',  ( 5.649999999999936406, 2.500000000000000000, -6.741600689897077281 ) ) ;
#7955 = DIRECTION ( 'NONE',  ( 0.000000000000000000, 1.000000000000000000, 0.000000000000000000 ) ) ;
#7956 = FACE_OUTER_BOUND ( 'NONE', #91363, .T. ) ;
#7957 = FACE_OUTER_BOUND ( 'NONE', #21278, .T. ) ;
#7958 = VERTEX_POINT ( 'NONE', #54275 ) ;
#7959 = AXIS2_PLACEMENT_3D ( 'NONE', #15797, #38025, #88395 ) ;
#7960 = DIRECTION ( 'NONE',  ( 0.000000000000000000, 0.000000000000000000, -1.000000000000000000 ) ) ;
#7961 = ORIENTED_EDGE ( 'NONE', *, *, #125765, .T. ) ;
#7962 = DIRECTION ( 'NONE',  ( -0.000000000000000000, -1.000000000000000000, -0.000000000000000000 ) ) ;
#7963 = EDGE_LOOP ( 'NONE', ( #116081, #45606 ) ) ;
#7964 = CARTESIAN_POINT ( 'NONE',  ( -0.4500000000000397571, 12.50000000000000000, -2.165063509461101710 ) ) ;
#7965 = ORIENTED_EDGE ( 'NONE', *, *, #32189, .F. ) ;
#7966 = CIRCLE ( 'NONE', #91600, 0.1000000000000000472 ) ;
#7967 = VERTEX_POINT ( 'NONE', #34659 ) ;
#7968 = DIRECTION ( 'NONE',  ( 0.000000000000000000, -0.9999939076577903929, 0.003490651415223739937 ) ) ;
#7969 = CARTESIAN_POINT ( 'NONE',  ( -4.400000000000025224, 12.50000000000000000, -0.4115034346978157509 ) ) ;
#7971 = VECTOR ( 'NONE', #121828, 1000.000000000000000 ) ;
#7970 = AXIS2_PLACEMENT_3D ( 'NONE', #15178, #55133, #95063 ) ;
#7972 = CARTESIAN_POINT ( 'NONE',  ( 11.44999999999990692, 2.500000000000000000, 1.818653347947321475 ) ) ;
#7973 = PLANE ( 'NONE',  #34013 ) ;
#7974 = DIRECTION ( 'NONE',  ( -0.000000000000000000, -1.000000000000000000, -0.000000000000000000 ) ) ;
#7975 = VERTEX_POINT ( 'NONE', #74555 ) ;
#7976 = CARTESIAN_POINT ( 'NONE',  ( 2.049999999999950084, 2.500000000000000000, -2.065063509461102065 ) ) ;
#7977 = LINE ( 'NONE', #18452, #120439 ) ;
#7978 = DIRECTION ( 'NONE',  ( -0.000000000000000000, -1.000000000000000000, -0.000000000000000000 ) ) ;
#7979 = CARTESIAN_POINT ( 'NONE',  ( -1.900000000000034550, 12.50000000000000000, 4.611443907251934426 ) ) ;
#7980 = DIRECTION ( 'NONE',  ( 0.000000000000000000, 0.000000000000000000, 1.000000000000000000 ) ) ;
#7981 = EDGE_CURVE ( 'NONE', #11241, #13143, #86291, .T. ) ;
#7982 = ORIENTED_EDGE ( 'NONE', *, *, #75871, .T. ) ;
#7983 = EDGE_LOOP ( 'NONE', ( #88318, #66219, #111288, #91720 ) ) ;
#7984 = DIRECTION ( 'NONE',  ( -4.274815082592931898E-19, -0.9999939076577903929, -0.003490651415223739937 ) ) ;
#7985 = ORIENTED_EDGE ( 'NONE', *, *, #68365, .F. ) ;
#7986 = FACE_OUTER_BOUND ( 'NONE', #46504, .T. ) ;
#7988 = ADVANCED_FACE ( 'NONE', ( #114474 ), #24814, .T. ) ;
#7987 = CARTESIAN_POINT ( 'NONE',  ( -3.750000000000027534, 2.500000000000000000, 2.957883832488649389 ) ) ;
#7989 = VECTOR ( 'NONE', #111250, 1000.000000000000000 ) ;
#7990 = CONICAL_SURFACE ( 'NONE', #81166, 0.1000000000000000472, 0.003490658503988666988 ) ;
#7993 = VERTEX_POINT ( 'NONE', #84377 ) ;
#7992 = EDGE_CURVE ( 'NONE', #73675, #58654, #129118, .T. ) ;
#7991 = AXIS2_PLACEMENT_3D ( 'NONE', #95335, #84863, #105799 ) ;
#7994 = CARTESIAN_POINT ( 'NONE',  ( 186.3333333333333144, 6.668395609140177704, -3.849999999999998312 ) ) ;
#7995 = CARTESIAN_POINT ( 'NONE',  ( -7.300000000000016698, 2.500000000000000000, -0.4464101615137783252 ) ) ;
#7996 = LINE ( 'NONE', #125836, #102603 ) ;
#7997 = EDGE_CURVE ( 'NONE', #24371, #60396, #56820, .T. ) ;
#7998 = DIRECTION ( 'NONE',  ( 0.000000000000000000, 1.000000000000000000, 0.000000000000000000 ) ) ;
#7999 = ORIENTED_EDGE ( 'NONE', *, *, #24766, .T. ) ;
#8000 = VECTOR ( 'NONE', #91026, 1000.000000000000000 ) ;
#8001 = CIRCLE ( 'NONE', #66588, 0.06509327318403745899 ) ;
#8002 = CARTESIAN_POINT ( 'NONE',  ( 9.999999999999952038, 2.500000000000000000, -0.1000000000000022815 ) ) ;
#8003 = LINE ( 'NONE', #28958, #22559 ) ;
#8004 = EDGE_CURVE ( 'NONE', #98964, #89242, #26109, .T. ) ;
#8005 = ORIENTED_EDGE ( 'NONE', *, *, #38630, .T. ) ;
#8006 = ADVANCED_FACE ( 'NONE', ( #96757 ), #12011, .T. ) ;
#8007 = CARTESIAN_POINT ( 'NONE',  ( -9.150000000000009237, 2.500000000000000000, -7.188010851410848723 ) ) ;
#8008 = PLANE ( 'NONE',  #95727 ) ;
#8009 = CIRCLE ( 'NONE', #83247, 0.06509327318403745899 ) ;
#8010 = CARTESIAN_POINT ( 'NONE',  ( -9.200000000000009948, 12.50000000000000000, -4.330127018922197202 ) ) ;
#8011 = VECTOR ( 'NONE', #1901, 1000.000000000000000 ) ;
#8012 = ORIENTED_EDGE ( 'NONE', *, *, #66031, .T. ) ;
#8013 = DIRECTION ( 'NONE',  ( 0.000000000000000000, 1.000000000000000000, 0.000000000000000000 ) ) ;
#8014 = ORIENTED_EDGE ( 'NONE', *, *, #1251, .T. ) ;
#8015 = DIRECTION ( 'NONE',  ( 0.000000000000000000, 0.000000000000000000, -1.000000000000000000 ) ) ;
#8016 = DIRECTION ( 'NONE',  ( 0.000000000000000000, 0.000000000000000000, -1.000000000000000000 ) ) ;
#8017 = CARTESIAN_POINT ( 'NONE',  ( 0.8499999999999553468, 12.50000000000000000, 2.230156782645134950 ) ) ;
#8018 = VERTEX_POINT ( 'NONE', #47042 ) ;
#8019 = CARTESIAN_POINT ( 'NONE',  ( 10.19999999999991580, 2.500000000000000000, -0.4464101615137783252 ) ) ;
#8020 = FACE_OUTER_BOUND ( 'NONE', #54727, .T. ) ;
#8021 = AXIS2_PLACEMENT_3D ( 'NONE', #64961, #93160, #113430 ) ;
#8022 = ORIENTED_EDGE ( 'NONE', *, *, #50790, .T. ) ;
#8023 = DIRECTION ( 'NONE',  ( 0.000000000000000000, 0.000000000000000000, -1.000000000000000000 ) ) ;
#8024 = ORIENTED_EDGE ( 'NONE', *, *, #6841, .F. ) ;
#8025 = DIRECTION ( 'NONE',  ( 0.000000000000000000, 0.000000000000000000, 1.000000000000000000 ) ) ;
#8026 = CONICAL_SURFACE ( 'NONE', #116692, 0.09999999999999982514, 0.003490658503988666988 ) ;
#8027 = ADVANCED_FACE ( 'NONE', ( #24171 ), #58001, .T. ) ;
#8028 = ORIENTED_EDGE ( 'NONE', *, *, #50513, .F. ) ;
#8029 = CARTESIAN_POINT ( 'NONE',  ( -11.44999999999999751, 2.500000000000000000, -2.411473670974874306 ) ) ;
#8030 = CARTESIAN_POINT ( 'NONE',  ( 8.149999999999923972, 2.500000000000000000, 2.411473670974873862 ) ) ;
#8031 = VERTEX_POINT ( 'NONE', #104646 ) ;
#8032 = ORIENTED_EDGE ( 'NONE', *, *, #43403, .F. ) ;
#8033 = CARTESIAN_POINT ( 'NONE',  ( 3.749999999999938716, 12.50000000000000000, 7.122917578226811486 ) ) ;
#8034 = DIRECTION ( 'NONE',  ( 0.000000000000000000, 0.000000000000000000, -1.000000000000000000 ) ) ;
#8035 = VECTOR ( 'NONE', #57540, 1000.000000000000000 ) ;
#8036 = VERTEX_POINT ( 'NONE', #94843 ) ;
#8037 = EDGE_CURVE ( 'NONE', #77053, #99802, #75202, .T. ) ;
#8038 = DIRECTION ( 'NONE',  ( -0.000000000000000000, -1.000000000000000000, -0.000000000000000000 ) ) ;
#8039 = CARTESIAN_POINT ( 'NONE',  ( 187.3177083336747160, 4.367472073101515306, 7.564683531250000925 ) ) ;
#8040 = AXIS2_PLACEMENT_3D ( 'NONE', #121821, #11221, #51818 ) ;
#8041 = DIRECTION ( 'NONE',  ( 0.000000000000000000, 0.000000000000000000, -1.000000000000000000 ) ) ;
#8042 = CARTESIAN_POINT ( 'NONE',  ( 10.19999999999991047, 12.50000000000000000, 4.676537180435972552 ) ) ;
#8043 = EDGE_CURVE ( 'NONE', #41325, #1525, #85170, .T. ) ;
#8044 = CARTESIAN_POINT ( 'NONE',  ( 11.24999999999994316, 2.500000000000000000, -6.495190528383302464 ) ) ;
#8045 = CARTESIAN_POINT ( 'NONE',  ( 0.3999999999999563904, 12.50000000000000000, 3.572213422710607489 ) ) ;
#8046 = CIRCLE ( 'NONE', #29000, 0.06509327318403743123 ) ;
#8047 = EDGE_CURVE ( 'NONE', #108686, #74379, #65369, .T. ) ;
#8048 = EDGE_CURVE ( 'NONE', #22803, #84610, #95483, .T. ) ;
#8049 = ORIENTED_EDGE ( 'NONE', *, *, #16182, .T. ) ;
#8050 = ORIENTED_EDGE ( 'NONE', *, *, #11237, .T. ) ;
#8052 = ORIENTED_EDGE ( 'NONE', *, *, #94040, .F. ) ;
#8051 = EDGE_CURVE ( 'NONE', #78443, #34708, #28758, .T. ) ;
#8053 = EDGE_LOOP ( 'NONE', ( #60486, #54273 ) ) ;
#8054 = FACE_OUTER_BOUND ( 'NONE', #33823, .T. ) ;
#8055 = DIRECTION ( 'NONE',  ( -0.000000000000000000, -1.000000000000000000, -0.000000000000000000 ) ) ;
#8056 = DIRECTION ( 'NONE',  ( 0.000000000000000000, 0.000000000000000000, -1.000000000000000000 ) ) ;
#8057 = VECTOR ( 'NONE', #33197, 1000.000000000000000 ) ;
#8058 = ORIENTED_EDGE ( 'NONE', *, *, #41673, .F. ) ;
#8059 = FACE_BOUND ( 'NONE', #75040, .T. ) ;
#8060 = ORIENTED_EDGE ( 'NONE', *, *, #85232, .T. ) ;
#8061 = DIRECTION ( 'NONE',  ( 0.000000000000000000, 0.000000000000000000, 1.000000000000000000 ) ) ;
#8062 = CARTESIAN_POINT ( 'NONE',  ( 7.899999999999924860, 2.500000000000000000, -4.230127018922201998 ) ) ;
#8063 = EDGE_CURVE ( 'NONE', #96874, #128968, #26686, .T. ) ;
#8064 = DIRECTION ( 'NONE',  ( 0.000000000000000000, 1.000000000000000000, 0.000000000000000000 ) ) ;
#8066 = EDGE_CURVE ( 'NONE', #4289, #75709, #30908, .T. ) ;
#8065 = VECTOR ( 'NONE', #97995, 1000.000000000000000 ) ;
#8067 = CARTESIAN_POINT ( 'NONE',  ( 5.599999999999931255, 2.500000000000000000, 3.983716857408420076 ) ) ;
#8068 = CARTESIAN_POINT ( 'NONE',  ( 15.83209681635537258, -2.500000000000000000, 5.404881881984332281 ) ) ;
#8069 = DIRECTION ( 'NONE',  ( 0.000000000000000000, -0.000000000000000000, 1.000000000000000000 ) ) ;
#8070 = DIRECTION ( 'NONE',  ( 0.000000000000000000, 0.000000000000000000, 1.000000000000000000 ) ) ;
#8071 = DIRECTION ( 'NONE',  ( 0.000000000000000000, 1.000000000000000000, 0.000000000000000000 ) ) ;
#8072 = DIRECTION ( 'NONE',  ( 0.000000000000000000, 0.000000000000000000, -1.000000000000000000 ) ) ;
#8073 = DIRECTION ( 'NONE',  ( 0.000000000000000000, 0.000000000000000000, -1.000000000000000000 ) ) ;
#8074 = ORIENTED_EDGE ( 'NONE', *, *, #94948, .T. ) ;
#8075 = EDGE_LOOP ( 'NONE', ( #101310, #102742 ) ) ;
#8076 = EDGE_LOOP ( 'NONE', ( #112757, #84910, #66942, #128629 ) ) ;
#8077 = VERTEX_POINT ( 'NONE', #118344 ) ;
#8078 = DIRECTION ( 'NONE',  ( 0.000000000000000000, -0.000000000000000000, 1.000000000000000000 ) ) ;
#8079 = AXIS2_PLACEMENT_3D ( 'NONE', #1291, #100764, #111901 ) ;
#8080 = DIRECTION ( 'NONE',  ( 0.000000000000000000, -0.000000000000000000, 1.000000000000000000 ) ) ;
#8082 = ORIENTED_EDGE ( 'NONE', *, *, #80366, .F. ) ;
#8081 = EDGE_LOOP ( 'NONE', ( #8058, #70587 ) ) ;
#8083 = ORIENTED_EDGE ( 'NONE', *, *, #110786, .T. ) ;
#8084 = DIRECTION ( 'NONE',  ( 0.000000000000000000, -0.000000000000000000, 1.000000000000000000 ) ) ;
#8085 = VECTOR ( 'NONE', #35374, 1000.000000000000000 ) ;
#8086 = CIRCLE ( 'NONE', #129405, 0.06509327318403743123 ) ;
#8087 = FACE_OUTER_BOUND ( 'NONE', #95560, .T. ) ;
#8089 = DIRECTION ( 'NONE',  ( 0.000000000000000000, -0.9999939076577903929, 0.003490651415223739937 ) ) ;
#8088 = VECTOR ( 'NONE', #75084, 1000.000000000000000 ) ;
#8090 = DIRECTION ( 'NONE',  ( -0.000000000000000000, 1.000000000000000000, -0.000000000000000000 ) ) ;
#8091 = DIRECTION ( 'NONE',  ( 0.000000000000000000, 0.000000000000000000, -1.000000000000000000 ) ) ;
#8092 = DIRECTION ( 'NONE',  ( -0.000000000000000000, -1.000000000000000000, -0.000000000000000000 ) ) ;
#8093 = EDGE_LOOP ( 'NONE', ( #111404, #111701, #122203, #56377 ) ) ;
#8094 = AXIS2_PLACEMENT_3D ( 'NONE', #45297, #85203, #26296 ) ;
#8096 = CARTESIAN_POINT ( 'NONE',  ( 3.549999999999940314, 2.500000000000000000, 6.841600689897072485 ) ) ;
#8095 = VECTOR ( 'NONE', #93445, 1000.000000000000000 ) ;
#8097 = ORIENTED_EDGE ( 'NONE', *, *, #95572, .T. ) ;
#8098 = AXIS2_PLACEMENT_3D ( 'NONE', #124505, #6610, #125755 ) ;
#8099 = ORIENTED_EDGE ( 'NONE', *, *, #73288, .T. ) ;
#8100 = EDGE_LOOP ( 'NONE', ( #123635, #78273 ) ) ;
#8101 = VECTOR ( 'NONE', #87271, 1000.000000000000000 ) ;
#8102 = DIRECTION ( 'NONE',  ( 0.000000000000000000, 1.000000000000000000, 0.000000000000000000 ) ) ;
#8103 = ORIENTED_EDGE ( 'NONE', *, *, #62044, .F. ) ;
#8104 = ORIENTED_EDGE ( 'NONE', *, *, #74264, .F. ) ;
#8105 = AXIS2_PLACEMENT_3D ( 'NONE', #112996, #103827, #63250 ) ;
#8106 = CARTESIAN_POINT ( 'NONE',  ( -4.150000000000025224, 2.500000000000000000, -1.572243186433550211 ) ) ;
#8107 = EDGE_CURVE ( 'NONE', #93340, #6835, #18202, .T. ) ;
#8108 = AXIS2_PLACEMENT_3D ( 'NONE', #4568, #85730, #54985 ) ;
#8109 = FACE_OUTER_BOUND ( 'NONE', #15207, .T. ) ;
#8110 = CARTESIAN_POINT ( 'NONE',  ( -8.750000000000010658, 12.50000000000000000, -7.188010851410848723 ) ) ;
#8111 = LINE ( 'NONE', #116773, #21127 ) ;
#8112 = DIRECTION ( 'NONE',  ( 0.000000000000000000, -0.000000000000000000, 1.000000000000000000 ) ) ;
#8113 = ORIENTED_EDGE ( 'NONE', *, *, #22845, .F. ) ;
#8114 = DIRECTION ( 'NONE',  ( 0.000000000000000000, 1.000000000000000000, 0.000000000000000000 ) ) ;
#8115 = AXIS2_PLACEMENT_3D ( 'NONE', #1785, #41750, #59464 ) ;
#8116 = ORIENTED_EDGE ( 'NONE', *, *, #31590, .F. ) ;
#8117 = DIRECTION ( 'NONE',  ( 0.000000000000000000, 0.000000000000000000, 1.000000000000000000 ) ) ;
#8118 = VERTEX_POINT ( 'NONE', #27368 ) ;
#8119 = DIRECTION ( 'NONE',  ( 0.000000000000000000, 0.000000000000000000, 1.000000000000000000 ) ) ;
#8120 = CARTESIAN_POINT ( 'NONE',  ( 21.25101261094845384, -0.2446824650187628403, -4.189229355218849982 ) ) ;
#8121 = CIRCLE ( 'NONE', #68756, 0.1000000000000002554 ) ;
#8122 = ORIENTED_EDGE ( 'NONE', *, *, #97382, .T. ) ;
#8123 = DIRECTION ( 'NONE',  ( 0.000000000000000000, -0.9999939076577903929, 0.003490651415223739937 ) ) ;
#8124 = CARTESIAN_POINT ( 'NONE',  ( 8.349999999999919709, 2.500000000000000000, -2.265063509461101798 ) ) ;
#8125 = ORIENTED_EDGE ( 'NONE', *, *, #61431, .T. ) ;
#8126 = AXIS2_PLACEMENT_3D ( 'NONE', #25853, #54646, #86701 ) ;
#8127 = CARTESIAN_POINT ( 'NONE',  ( 6.249999999999932498, 12.50000000000000000, -5.737276932171712751 ) ) ;
#8128 = ORIENTED_EDGE ( 'NONE', *, *, #13503, .F. ) ;
#8129 = ORIENTED_EDGE ( 'NONE', *, *, #69329, .F. ) ;
#8130 = CARTESIAN_POINT ( 'NONE',  ( -11.64999999999999680, 2.500000000000000000, -6.595190528383298556 ) ) ;
#8131 = CARTESIAN_POINT ( 'NONE',  ( -13.34999999999999076, 2.500000000000000000, -2.165063509461099489 ) ) ;
#8132 = CARTESIAN_POINT ( 'NONE',  ( 186.0885416670080872, -6.551208109652273848, -3.782341765625003571 ) ) ;
#8133 = DIRECTION ( 'NONE',  ( -0.000000000000000000, -1.000000000000000000, -0.000000000000000000 ) ) ;
#8134 = AXIS2_PLACEMENT_3D ( 'NONE', #47790, #27473, #98161 ) ;
#8135 = CARTESIAN_POINT ( 'NONE',  ( 10.39999999999991154, 12.50000000000000000, 5.022947341949748790 ) ) ;
#8136 = DIRECTION ( 'NONE',  ( -0.000000000000000000, 1.000000000000000000, -0.000000000000000000 ) ) ;
#8137 = AXIS2_PLACEMENT_3D ( 'NONE', #32436, #50759, #40302 ) ;
#8138 = VERTEX_POINT ( 'NONE', #77136 ) ;
#8139 = CARTESIAN_POINT ( 'NONE',  ( 8.299999999999922551, 2.500000000000000000, -2.385244779468109755E-15 ) ) ;
#8141 = EDGE_CURVE ( 'NONE', #103702, #33924, #3694, .T. ) ;
#8140 = CARTESIAN_POINT ( 'NONE',  ( 11.04999999999991012, 2.500000000000000000, 6.841600689897072485 ) ) ;
#8142 = ORIENTED_EDGE ( 'NONE', *, *, #128917, .F. ) ;
#8143 = CIRCLE ( 'NONE', #79278, 0.1000000000000002554 ) ;
#8144 = VECTOR ( 'NONE', #101120, 1000.000000000000000 ) ;
#8145 = EDGE_CURVE ( 'NONE', #83259, #86941, #87586, .T. ) ;
#8146 = FACE_OUTER_BOUND ( 'NONE', #8303, .T. ) ;
#8147 = CARTESIAN_POINT ( 'NONE',  ( 0.3999999999999563904, 12.50000000000000000, 4.957854068765711553 ) ) ;
#8148 = CARTESIAN_POINT ( 'NONE',  ( 10.79999999999991012, 2.500000000000000000, 4.430127018922196847 ) ) ;
#8149 = CARTESIAN_POINT ( 'NONE',  ( 9.999999999999948486, 2.500000000000000000, 4.330127018922196314 ) ) ;
#8150 = EDGE_CURVE ( 'NONE', #2148, #54782, #127046, .T. ) ;
#8151 = DIRECTION ( 'NONE',  ( 0.000000000000000000, 1.000000000000000000, 0.000000000000000000 ) ) ;
#8152 = ORIENTED_EDGE ( 'NONE', *, *, #88891, .F. ) ;
#8154 = VECTOR ( 'NONE', #73687, 1000.000000000000000 ) ;
#8153 = AXIS2_PLACEMENT_3D ( 'NONE', #35197, #83645, #63996 ) ;
#8155 = FACE_OUTER_BOUND ( 'NONE', #58815, .T. ) ;
#8156 = DIRECTION ( 'NONE',  ( 0.000000000000000000, 1.000000000000000000, 0.000000000000000000 ) ) ;
#8157 = ADVANCED_FACE ( 'NONE', ( #119624 ), #58790, .T. ) ;
#8158 = EDGE_CURVE ( 'NONE', #60755, #25630, #110315, .T. ) ;
#8159 = EDGE_CURVE ( 'NONE', #79874, #74365, #18850, .T. ) ;
#8160 = ADVANCED_FACE ( 'NONE', ( #48320 ), #98058, .T. ) ;
#8161 = EDGE_LOOP ( 'NONE', ( #118595, #112092 ) ) ;
#8162 = CARTESIAN_POINT ( 'NONE',  ( 3.099999999999945466, 2.500000000000000000, 0.2464101615137735679 ) ) ;
#8163 = ORIENTED_EDGE ( 'NONE', *, *, #35843, .F. ) ;
#8164 = ORIENTED_EDGE ( 'NONE', *, *, #95668, .F. ) ;
#8165 = DIRECTION ( 'NONE',  ( 0.000000000000000000, 0.000000000000000000, 1.000000000000000000 ) ) ;
#8166 = AXIS2_PLACEMENT_3D ( 'NONE', #115751, #26102, #78440 ) ;
#8167 = EDGE_LOOP ( 'NONE', ( #57481, #50678 ) ) ;
#8168 = DIRECTION ( 'NONE',  ( 0.000000000000000000, 0.000000000000000000, 1.000000000000000000 ) ) ;
#8169 = DIRECTION ( 'NONE',  ( -0.000000000000000000, 1.000000000000000000, -0.000000000000000000 ) ) ;
#8170 = CARTESIAN_POINT ( 'NONE',  ( -6.650000000000015454, 12.50000000000000000, 7.188010851410848723 ) ) ;
#8171 = ORIENTED_EDGE ( 'NONE', *, *, #39690, .T. ) ;
#8172 = AXIS2_PLACEMENT_3D ( 'NONE', #32664, #102652, #13623 ) ;
#8173 = CARTESIAN_POINT ( 'NONE',  ( 10.64999999999991331, 2.500000000000000000, -1.918653347947325782 ) ) ;
#8174 = AXIS2_PLACEMENT_3D ( 'NONE', #51621, #10390, #69969 ) ;
#8176 = EDGE_LOOP ( 'NONE', ( #72264, #68849 ) ) ;
#8175 = DIRECTION ( 'NONE',  ( -0.000000000000000000, 1.000000000000000000, -0.000000000000000000 ) ) ;
#8177 = DIRECTION ( 'NONE',  ( 1.000000000000000000, 0.000000000000000000, 0.000000000000000000 ) ) ;
#8178 = CARTESIAN_POINT ( 'NONE',  ( 7.699999999999922018, 12.50000000000000000, 0.3464101615137735735 ) ) ;
#8179 = CONICAL_SURFACE ( 'NONE', #14432, 0.1000000000000002554, 0.003490658503988666988 ) ;
#8180 = ORIENTED_EDGE ( 'NONE', *, *, #1074, .F. ) ;
#8181 = CIRCLE ( 'NONE', #106488, 0.1000000000000002554 ) ;
#8182 = CIRCLE ( 'NONE', #127337, 0.09999999999999982514 ) ;
#8183 = EDGE_LOOP ( 'NONE', ( #66123, #22818, #23073, #113032 ) ) ;
#8184 = EDGE_LOOP ( 'NONE', ( #92947, #50308 ) ) ;
#8185 = FACE_OUTER_BOUND ( 'NONE', #112716, .T. ) ;
#8186 = DIRECTION ( 'NONE',  ( 0.000000000000000000, 0.000000000000000000, 1.000000000000000000 ) ) ;
#8187 = DIRECTION ( 'NONE',  ( 0.000000000000000000, 0.000000000000000000, 1.000000000000000000 ) ) ;
#8188 = EDGE_CURVE ( 'NONE', #59250, #125502, #67270, .T. ) ;
#8189 = FACE_BOUND ( 'NONE', #90233, .T. ) ;
#8190 = ORIENTED_EDGE ( 'NONE', *, *, #92889, .F. ) ;
#8191 = AXIS2_PLACEMENT_3D ( 'NONE', #93849, #104312, #104933 ) ;
#8192 = DIRECTION ( 'NONE',  ( -0.000000000000000000, 1.000000000000000000, -0.000000000000000000 ) ) ;
#8193 = CARTESIAN_POINT ( 'NONE',  ( -3.749999999999991118, 12.50000000000000000, -2.165063509461101710 ) ) ;
#8194 = ORIENTED_EDGE ( 'NONE', *, *, #124342, .T. ) ;
#8195 = AXIS2_PLACEMENT_3D ( 'NONE', #83027, #41182, #120368 ) ;
#8196 = CARTESIAN_POINT ( 'NONE',  ( 184.8750000000000000, 8.891194145520236347, 5.444286225454521982E-16 ) ) ;
#8198 = EDGE_CURVE ( 'NONE', #28988, #67778, #72757, .T. ) ;
#8197 = DIRECTION ( 'NONE',  ( 0.000000000000000000, -0.000000000000000000, 1.000000000000000000 ) ) ;
#8199 = CARTESIAN_POINT ( 'NONE',  ( -5.200000000000025935, 2.500000000000000000, -3.983716857408426293 ) ) ;
#8200 = EDGE_CURVE ( 'NONE', #12706, #69185, #43535, .T. ) ;
#8201 = FACE_OUTER_BOUND ( 'NONE', #108824, .T. ) ;
#8202 = DIRECTION ( 'NONE',  ( -4.274815082592931898E-19, -0.9999939076577903929, -0.003490651415223739937 ) ) ;
#8203 = EDGE_CURVE ( 'NONE', #11332, #36386, #95744, .T. ) ;
#8204 = ORIENTED_EDGE ( 'NONE', *, *, #121688, .F. ) ;
#8205 = EDGE_LOOP ( 'NONE', ( #22487, #79167, #42391, #31033 ) ) ;
#8206 = EDGE_LOOP ( 'NONE', ( #88608, #23893, #872, #8050 ) ) ;
#8207 = ORIENTED_EDGE ( 'NONE', *, *, #17664, .T. ) ;
#8208 = EDGE_LOOP ( 'NONE', ( #115295, #1477, #129275, #55833 ) ) ;
#8209 = CARTESIAN_POINT ( 'NONE',  ( -0.2000000000000412836, 12.50000000000000000, 4.741630453620009789 ) ) ;
#8210 = ADVANCED_FACE ( 'NONE', ( #79085 ), #79032, .T. ) ;
#8211 = DIRECTION ( 'NONE',  ( -0.000000000000000000, -1.000000000000000000, -0.000000000000000000 ) ) ;
#8213 = EDGE_CURVE ( 'NONE', #87323, #88035, #81083, .T. ) ;
#8212 = EDGE_LOOP ( 'NONE', ( #97842, #123261, #110199, #95599 ) ) ;
#8214 = FACE_BOUND ( 'NONE', #127139, .T. ) ;
#8215 = DIRECTION ( 'NONE',  ( 0.000000000000000000, 0.000000000000000000, 1.000000000000000000 ) ) ;
#8216 = EDGE_CURVE ( 'NONE', #25321, #42231, #1642, .T. ) ;
#8217 = ADVANCED_FACE ( 'NONE', ( #67950 ), #38526, .T. ) ;
#8218 = EDGE_CURVE ( 'NONE', #121663, #54095, #122867, .T. ) ;
#8219 = CARTESIAN_POINT ( 'NONE',  ( -15.39999999999997904, 2.500000000000000000, 0.1000000000000000056 ) ) ;
#8220 = DIRECTION ( 'NONE',  ( 0.000000000000000000, -0.000000000000000000, 1.000000000000000000 ) ) ;
#8221 = CARTESIAN_POINT ( 'NONE',  ( 3.949999999999938893, 2.500000000000000000, 6.148780366869520009 ) ) ;
#8222 = DIRECTION ( 'NONE',  ( 0.000000000000000000, 0.000000000000000000, 1.000000000000000000 ) ) ;
#8223 = ORIENTED_EDGE ( 'NONE', *, *, #44518, .F. ) ;
#8224 = AXIS2_PLACEMENT_3D ( 'NONE', #95708, #47258, #26326 ) ;
#8225 = CARTESIAN_POINT ( 'NONE',  ( 17.46754094667539903, -1.506946019336847575, 5.249106724335615759 ) ) ;
#8226 = EDGE_CURVE ( 'NONE', #60337, #124886, #11611, .T. ) ;
#8227 = ORIENTED_EDGE ( 'NONE', *, *, #18375, .T. ) ;
#8228 = ORIENTED_EDGE ( 'NONE', *, *, #104525, .T. ) ;
#8229 = VERTEX_POINT ( 'NONE', #103223 ) ;
#8230 = DIRECTION ( 'NONE',  ( -4.274815082592931898E-19, -0.9999939076577903929, -0.003490651415223739937 ) ) ;
#8231 = CARTESIAN_POINT ( 'NONE',  ( -4.600000000000024514, 2.500000000000000000, -0.6928203230275542523 ) ) ;
#8232 = DIRECTION ( 'NONE',  ( -0.000000000000000000, -1.000000000000000000, -0.000000000000000000 ) ) ;
#8233 = VERTEX_POINT ( 'NONE', #1779 ) ;
#8234 = LINE ( 'NONE', #39667, #22587 ) ;
#8235 = DIRECTION ( 'NONE',  ( 0.000000000000000000, 1.000000000000000000, 0.000000000000000000 ) ) ;
#8238 = VECTOR ( 'NONE', #111043, 1000.000000000000000 ) ;
#8237 = DIRECTION ( 'NONE',  ( 0.000000000000000000, 0.000000000000000000, 1.000000000000000000 ) ) ;
#8236 = CONICAL_SURFACE ( 'NONE', #91876, 0.1000000000000002554, 0.003490658503988666988 ) ;
#8239 = FACE_OUTER_BOUND ( 'NONE', #55589, .T. ) ;
#8240 = CARTESIAN_POINT ( 'NONE',  ( 15.79999999999989058, 12.50000000000000000, -2.385244779468109755E-15 ) ) ;
#8241 = DIRECTION ( 'NONE',  ( 0.000000000000000000, 1.000000000000000000, 0.000000000000000000 ) ) ;
#8242 = AXIS2_PLACEMENT_3D ( 'NONE', #80692, #40117, #70864 ) ;
#8243 = DIRECTION ( 'NONE',  ( -0.000000000000000000, 1.000000000000000000, -0.000000000000000000 ) ) ;
#8244 = ORIENTED_EDGE ( 'NONE', *, *, #90504, .T. ) ;
#8245 = DIRECTION ( 'NONE',  ( -0.000000000000000000, -1.000000000000000000, -0.000000000000000000 ) ) ;
#8247 = AXIS2_PLACEMENT_3D ( 'NONE', #65802, #26538, #17331 ) ;
#8246 = AXIS2_PLACEMENT_3D ( 'NONE', #9589, #120194, #41011 ) ;
#8248 = ORIENTED_EDGE ( 'NONE', *, *, #124723, .F. ) ;
#8249 = ORIENTED_EDGE ( 'NONE', *, *, #81780, .F. ) ;
#8250 = FACE_OUTER_BOUND ( 'NONE', #25595, .T. ) ;
#8251 = DIRECTION ( 'NONE',  ( -0.000000000000000000, 1.000000000000000000, -0.000000000000000000 ) ) ;
#8252 = CARTESIAN_POINT ( 'NONE',  ( 5.649999999999934630, 2.500000000000000000, 6.841600689897072485 ) ) ;
#8253 = ORIENTED_EDGE ( 'NONE', *, *, #14810, .T. ) ;
#8254 = VERTEX_POINT ( 'NONE', #33212 ) ;
#8255 = DIRECTION ( 'NONE',  ( -4.274815082592931898E-19, -0.9999939076577903929, -0.003490651415223739937 ) ) ;
#8256 = ADVANCED_FACE ( 'NONE', ( #62665 ), #82304, .T. ) ;
#8257 = CARTESIAN_POINT ( 'NONE',  ( -1.850000000000033840, 12.50000000000000000, 6.776507416713035248 ) ) ;
#8258 = CARTESIAN_POINT ( 'NONE',  ( 87.50000000000001421, 0.000000000000000000, 0.000000000000000000 ) ) ;
#8260 = ORIENTED_EDGE ( 'NONE', *, *, #57897, .T. ) ;
#8259 = AXIS2_PLACEMENT_3D ( 'NONE', #63781, #103704, #14007 ) ;
#8261 = ORIENTED_EDGE ( 'NONE', *, *, #43099, .F. ) ;
#8262 = FACE_OUTER_BOUND ( 'NONE', #126531, .T. ) ;
#8263 = EDGE_LOOP ( 'NONE', ( #20523, #109086, #72410, #10810 ) ) ;
#8264 = DIRECTION ( 'NONE',  ( -4.274815082592931898E-19, -0.9999939076577903929, -0.003490651415223739937 ) ) ;
#8265 = CIRCLE ( 'NONE', #4139, 0.06509327318403745899 ) ;
#8267 = DIRECTION ( 'NONE',  ( 0.000000000000000000, 1.000000000000000000, 0.000000000000000000 ) ) ;
#8266 = AXIS2_PLACEMENT_3D ( 'NONE', #94110, #64647, #34570 ) ;
#8268 = EDGE_LOOP ( 'NONE', ( #110623, #121270 ) ) ;
#8269 = CARTESIAN_POINT ( 'NONE',  ( 11.24999999999990763, 12.50000000000000000, -7.253104124594891289 ) ) ;
#8270 = DIRECTION ( 'NONE',  ( 0.000000000000000000, 0.000000000000000000, -1.000000000000000000 ) ) ;
#8271 = DIRECTION ( 'NONE',  ( 0.000000000000000000, 0.000000000000000000, -1.000000000000000000 ) ) ;
#8272 = EDGE_CURVE ( 'NONE', #52442, #19417, #85270, .T. ) ;
#8273 = DIRECTION ( 'NONE',  ( 0.000000000000000000, 0.000000000000000000, 1.000000000000000000 ) ) ;
#8274 = ORIENTED_EDGE ( 'NONE', *, *, #119874, .T. ) ;
#8276 = VECTOR ( 'NONE', #86497, 1000.000000000000000 ) ;
#8275 = AXIS2_PLACEMENT_3D ( 'NONE', #109719, #10835, #99260 ) ;
#8278 = DIRECTION ( 'NONE',  ( -4.274815082592931898E-19, -0.9999939076577903929, -0.003490651415223739937 ) ) ;
#8277 = AXIS2_PLACEMENT_3D ( 'NONE', #84406, #75231, #65405 ) ;
#8279 = VERTEX_POINT ( 'NONE', #111079 ) ;
#8280 = EDGE_LOOP ( 'NONE', ( #26470, #65135, #103696, #120723 ) ) ;
#8281 = DIRECTION ( 'NONE',  ( 0.000000000000000000, -0.000000000000000000, 1.000000000000000000 ) ) ;
#8282 = DIRECTION ( 'NONE',  ( -0.000000000000000000, 1.000000000000000000, -0.000000000000000000 ) ) ;
#8283 = DIRECTION ( 'NONE',  ( -0.000000000000000000, 1.000000000000000000, -0.000000000000000000 ) ) ;
#8284 = DIRECTION ( 'NONE',  ( 0.000000000000000000, 1.000000000000000000, 0.000000000000000000 ) ) ;
#8285 = AXIS2_PLACEMENT_3D ( 'NONE', #49276, #21738, #99001 ) ;
#8286 = DIRECTION ( 'NONE',  ( 0.000000000000000000, 0.000000000000000000, 1.000000000000000000 ) ) ;
#8287 = CARTESIAN_POINT ( 'NONE',  ( -9.600000000000008527, 12.50000000000000000, -5.022947341949749678 ) ) ;
#8288 = CONICAL_SURFACE ( 'NONE', #104439, 0.09999999999999982514, 0.003490658503988666988 ) ;
#8289 = DIRECTION ( 'NONE',  ( -0.000000000000000000, 1.000000000000000000, -0.000000000000000000 ) ) ;
#8290 = LINE ( 'NONE', #48227, #72069 ) ;
#8291 = CARTESIAN_POINT ( 'NONE',  ( 12.09999999999990550, 2.500000000000000000, -4.230127018922201998 ) ) ;
#8292 = DIRECTION ( 'NONE',  ( 0.000000000000000000, 0.000000000000000000, -1.000000000000000000 ) ) ;
#8293 = AXIS2_PLACEMENT_3D ( 'NONE', #81895, #41992, #2048 ) ;
#8294 = EDGE_CURVE ( 'NONE', #43428, #95183, #106209, .T. ) ;
#8295 = ORIENTED_EDGE ( 'NONE', *, *, #22020, .T. ) ;
#8296 = AXIS2_PLACEMENT_3D ( 'NONE', #31610, #22451, #53191 ) ;
#8297 = CARTESIAN_POINT ( 'NONE',  ( 12.29999999999990479, 2.500000000000000000, -3.883716857408426648 ) ) ;
#8298 = DIRECTION ( 'NONE',  ( 0.000000000000000000, 0.000000000000000000, 1.000000000000000000 ) ) ;
#8299 = PLANE ( 'NONE',  #110168 ) ;
#8300 = DIRECTION ( 'NONE',  ( 0.000000000000000000, 1.000000000000000000, 0.000000000000000000 ) ) ;
#8301 = DIRECTION ( 'NONE',  ( 0.000000000000000000, 1.000000000000000000, 0.000000000000000000 ) ) ;
#8302 = ADVANCED_FACE ( 'NONE', ( #52188 ), #122940, .T. ) ;
#8303 = EDGE_LOOP ( 'NONE', ( #61559, #77245, #24599, #38359 ) ) ;
#8304 = DIRECTION ( 'NONE',  ( 0.000000000000000000, 0.000000000000000000, 1.000000000000000000 ) ) ;
#8305 = DIRECTION ( 'NONE',  ( 0.000000000000000000, -0.9999939076577903929, 0.003490651415223739937 ) ) ;
#8307 = EDGE_LOOP ( 'NONE', ( #112891, #64953, #69843, #96364 ) ) ;
#8306 = CARTESIAN_POINT ( 'NONE',  ( 2.949999999999945111, 2.500000000000000000, 2.265063509461097357 ) ) ;
#8308 = EDGE_CURVE ( 'NONE', #101949, #97882, #66486, .T. ) ;
#8309 = EDGE_CURVE ( 'NONE', #52226, #108554, #70531, .T. ) ;
#8310 = EDGE_CURVE ( 'NONE', #81253, #64554, #83230, .T. ) ;
#8311 = ADVANCED_FACE ( 'NONE', ( #52828 ), #92767, .T. ) ;
#8312 = EDGE_CURVE ( 'NONE', #121486, #89530, #53981, .T. ) ;
#8313 = EDGE_LOOP ( 'NONE', ( #105959, #45330 ) ) ;
#8314 = CARTESIAN_POINT ( 'NONE',  ( -3.350000000000028955, 2.500000000000000000, 7.088010851410848190 ) ) ;
#8315 = VERTEX_POINT ( 'NONE', #42374 ) ;
#8316 = EDGE_LOOP ( 'NONE', ( #85206, #62823 ) ) ;
#8317 = EDGE_LOOP ( 'NONE', ( #121951, #45089 ) ) ;
#8318 = DIRECTION ( 'NONE',  ( -0.000000000000000000, 1.000000000000000000, -0.000000000000000000 ) ) ;
#8319 = AXIS2_PLACEMENT_3D ( 'NONE', #76528, #124979, #75226 ) ;
#8320 = EDGE_CURVE ( 'NONE', #38693, #95740, #110401, .T. ) ;
#8321 = DIRECTION ( 'NONE',  ( -0.000000000000000000, -1.000000000000000000, -0.000000000000000000 ) ) ;
#8322 = LINE ( 'NONE', #69168, #16939 ) ;
#8323 = ADVANCED_FACE ( 'NONE', ( #61371 ), #90821, .T. ) ;
#8324 = DIRECTION ( 'NONE',  ( -4.274815082592931898E-19, -0.9999939076577903929, -0.003490651415223739937 ) ) ;
#8326 = ORIENTED_EDGE ( 'NONE', *, *, #98644, .T. ) ;
#8325 = EDGE_CURVE ( 'NONE', #103611, #81046, #99950, .T. ) ;
#8328 = AXIS2_PLACEMENT_3D ( 'NONE', #11422, #1591, #30445 ) ;
#8327 = CIRCLE ( 'NONE', #123267, 0.06509327318403745899 ) ;
#8329 = CARTESIAN_POINT ( 'NONE',  ( -10.60000000000000320, 2.500000000000000000, -3.983716857408421852 ) ) ;
#8330 = VERTEX_POINT ( 'NONE', #41103 ) ;
#8331 = DIRECTION ( 'NONE',  ( 0.000000000000000000, 0.000000000000000000, -1.000000000000000000 ) ) ;
#8332 = CARTESIAN_POINT ( 'NONE',  ( 15.50772381900100605, -2.500000000000000444, -6.996973298636910421 ) ) ;
#8333 = CARTESIAN_POINT ( 'NONE',  ( 21.23528140090950700, 2.699413673072311504, 2.293764360948888914 ) ) ;
#8334 = FACE_OUTER_BOUND ( 'NONE', #98945, .T. ) ;
#8335 = DIRECTION ( 'NONE',  ( 0.000000000000000000, -0.9999939076577903929, 0.003490651415223739937 ) ) ;
#8336 = VERTEX_POINT ( 'NONE', #10940 ) ;
#8338 = AXIS2_PLACEMENT_3D ( 'NONE', #53743, #5907, #93671 ) ;
#8337 = AXIS2_PLACEMENT_3D ( 'NONE', #124553, #93802, #74160 ) ;
#8339 = VERTEX_POINT ( 'NONE', #23351 ) ;
#8340 = VERTEX_POINT ( 'NONE', #120290 ) ;
#8341 = ORIENTED_EDGE ( 'NONE', *, *, #59366, .F. ) ;
#8342 = VERTEX_POINT ( 'NONE', #30631 ) ;
#8343 = LINE ( 'NONE', #118304, #108904 ) ;
#8344 = CARTESIAN_POINT ( 'NONE',  ( -3.150000000000030553, 12.50000000000000000, 6.148780366869520009 ) ) ;
#8345 = DIRECTION ( 'NONE',  ( -0.000000000000000000, 1.000000000000000000, -0.000000000000000000 ) ) ;
#8346 = FACE_BOUND ( 'NONE', #28529, .T. ) ;
#8347 = PLANE ( 'NONE',  #22211 ) ;
#8348 = CARTESIAN_POINT ( 'NONE',  ( 0.8499999999999557909, 2.500000000000000000, -6.595190528383302109 ) ) ;
#8349 = DIRECTION ( 'NONE',  ( 0.000000000000000000, -0.000000000000000000, 1.000000000000000000 ) ) ;
#8350 = LINE ( 'NONE', #101900, #39672 ) ;
#8351 = CARTESIAN_POINT ( 'NONE',  ( 186.3385416670080872, 6.551208109652274736, 3.782341765625001351 ) ) ;
#8352 = PLANE ( 'NONE',  #76107 ) ;
#8353 = CARTESIAN_POINT ( 'NONE',  ( 9.799999999999915445, 2.500000000000000000, 3.883716857408421319 ) ) ;
#8354 = AXIS2_PLACEMENT_3D ( 'NONE', #101490, #11805, #79281 ) ;
#8355 = AXIS2_PLACEMENT_3D ( 'NONE', #4840, #104351, #64420 ) ;
#8356 = DIRECTION ( 'NONE',  ( -0.000000000000000000, -1.000000000000000000, -0.000000000000000000 ) ) ;
#8357 = EDGE_LOOP ( 'NONE', ( #16666, #25741, #103613, #79520 ) ) ;
#8358 = ORIENTED_EDGE ( 'NONE', *, *, #48435, .F. ) ;
#8359 = VERTEX_POINT ( 'NONE', #110456 ) ;
#8360 = ORIENTED_EDGE ( 'NONE', *, *, #69936, .F. ) ;
#8361 = FACE_OUTER_BOUND ( 'NONE', #109469, .T. ) ;
#8362 = EDGE_CURVE ( 'NONE', #5223, #118122, #51835, .T. ) ;
#8363 = FACE_BOUND ( 'NONE', #116783, .T. ) ;
#8364 = DIRECTION ( 'NONE',  ( 0.000000000000000000, 0.000000000000000000, -1.000000000000000000 ) ) ;
#8365 = EDGE_CURVE ( 'NONE', #72840, #62761, #71176, .T. ) ;
#8366 = EDGE_CURVE ( 'NONE', #23090, #16470, #127147, .T. ) ;
#8367 = ORIENTED_EDGE ( 'NONE', *, *, #23260, .T. ) ;
#8368 = DIRECTION ( 'NONE',  ( -0.000000000000000000, -1.000000000000000000, -0.000000000000000000 ) ) ;
#8369 = FACE_OUTER_BOUND ( 'NONE', #12876, .T. ) ;
#8370 = CARTESIAN_POINT ( 'NONE',  ( 10.64999999999990976, 2.500000000000000000, -6.841600689897077814 ) ) ;
#8371 = CARTESIAN_POINT ( 'NONE',  ( 0.6499999999999561684, 2.500000000000000000, 2.611473670974873151 ) ) ;
#8372 = CIRCLE ( 'NONE', #102479, 0.06509327318403745899 ) ;
#8373 = ORIENTED_EDGE ( 'NONE', *, *, #31174, .T. ) ;
#8374 = CARTESIAN_POINT ( 'NONE',  ( 16.55874544816229132, -0.4845305829427751232, 6.091953208798936537 ) ) ;
#8375 = DIRECTION ( 'NONE',  ( 0.000000000000000000, 0.000000000000000000, -1.000000000000000000 ) ) ;
#8376 = EDGE_CURVE ( 'NONE', #42757, #107800, #114955, .T. ) ;
#8377 = CIRCLE ( 'NONE', #52221, 0.1000000000000002554 ) ;
#8378 = AXIS2_PLACEMENT_3D ( 'NONE', #66138, #106073, #107999 ) ;
#8379 = ORIENTED_EDGE ( 'NONE', *, *, #4257, .T. ) ;
#8380 = ORIENTED_EDGE ( 'NONE', *, *, #112845, .T. ) ;
#8381 = CARTESIAN_POINT ( 'NONE',  ( -2.900000000000029665, 12.50000000000000000, 3.572213422710607489 ) ) ;
#8382 = CARTESIAN_POINT ( 'NONE',  ( -12.89999999999999147, 12.50000000000000000, -0.6928203230275500335 ) ) ;
#8383 = AXIS2_PLACEMENT_3D ( 'NONE', #114579, #24928, #64838 ) ;
#8384 = FACE_OUTER_BOUND ( 'NONE', #67960, .T. ) ;
#8385 = DIRECTION ( 'NONE',  ( 0.000000000000000000, 0.000000000000000000, -1.000000000000000000 ) ) ;
#8386 = EDGE_LOOP ( 'NONE', ( #21515, #31620, #80877, #68622 ) ) ;
#8387 = DIRECTION ( 'NONE',  ( -0.000000000000000000, 1.000000000000000000, -0.000000000000000000 ) ) ;
#8388 = EDGE_LOOP ( 'NONE', ( #95082, #27655, #121407, #89385 ) ) ;
#8389 = ORIENTED_EDGE ( 'NONE', *, *, #12472, .T. ) ;
#8390 = DIRECTION ( 'NONE',  ( 0.000000000000000000, -0.000000000000000000, 1.000000000000000000 ) ) ;
#8391 = ADVANCED_FACE ( 'NONE', ( #66505 ), #113691, .T. ) ;
#8392 = ORIENTED_EDGE ( 'NONE', *, *, #3207, .T. ) ;
#8393 = FACE_OUTER_BOUND ( 'NONE', #22035, .T. ) ;
#8394 = FACE_BOUND ( 'NONE', #80469, .T. ) ;
#8395 = ORIENTED_EDGE ( 'NONE', *, *, #79469, .T. ) ;
#8396 = CARTESIAN_POINT ( 'NONE',  ( 113.0003993415903523, 7.700259312267349721, 0.1577655332996449056 ) ) ;
#8397 = VERTEX_POINT ( 'NONE', #5004 ) ;
#8398 = DIRECTION ( 'NONE',  ( 0.000000000000000000, 1.000000000000000000, 0.000000000000000000 ) ) ;
#8399 = CARTESIAN_POINT ( 'NONE',  ( 8.149999999999920419, 2.500000000000000000, 6.841600689897072485 ) ) ;
#8400 = DIRECTION ( 'NONE',  ( 0.000000000000000000, -0.000000000000000000, 1.000000000000000000 ) ) ;
#8401 = CARTESIAN_POINT ( 'NONE',  ( 1.899999999999949507, 2.500000000000000000, 4.576537180435972019 ) ) ;
#8402 = DIRECTION ( 'NONE',  ( 0.000000000000000000, 1.000000000000000000, 0.000000000000000000 ) ) ;
#8403 = ORIENTED_EDGE ( 'NONE', *, *, #41940, .T. ) ;
#8404 = ORIENTED_EDGE ( 'NONE', *, *, #40841, .T. ) ;
#8405 = EDGE_LOOP ( 'NONE', ( #84692, #36281 ) ) ;
#8406 = DIRECTION ( 'NONE',  ( 0.000000000000000000, 0.000000000000000000, -1.000000000000000000 ) ) ;
#8407 = ADVANCED_FACE ( 'NONE', ( #54747 ), #25955, .T. ) ;
#8408 = DIRECTION ( 'NONE',  ( -4.274815082592931898E-19, -0.9999939076577903929, -0.003490651415223739937 ) ) ;
#8410 = DIRECTION ( 'NONE',  ( 0.000000000000000000, 0.000000000000000000, -1.000000000000000000 ) ) ;
#8409 = AXIS2_PLACEMENT_3D ( 'NONE', #97939, #88772, #77645 ) ;
#8412 = ORIENTED_EDGE ( 'NONE', *, *, #91001, .T. ) ;
#8411 = ORIENTED_EDGE ( 'NONE', *, *, #79012, .T. ) ;
#8413 = ORIENTED_EDGE ( 'NONE', *, *, #36580, .F. ) ;
#8414 = AXIS2_PLACEMENT_3D ( 'NONE', #84893, #54155, #114352 ) ;
#8415 = CARTESIAN_POINT ( 'NONE',  ( 7.499999999999923617, 12.50000000000000000, 0.6928203230275494784 ) ) ;
#8416 = DIRECTION ( 'NONE',  ( 0.000000000000000000, 0.000000000000000000, 1.000000000000000000 ) ) ;
#8417 = SHAPE_DEFINITION_REPRESENTATION ( #77351, #18450 ) ;
#8418 = AXIS2_PLACEMENT_3D ( 'NONE', #123308, #23830, #122664 ) ;
#8419 = DIRECTION ( 'NONE',  ( 0.000000000000000000, 0.000000000000000000, 1.000000000000000000 ) ) ;
#8420 = DIRECTION ( 'NONE',  ( -0.000000000000000000, 1.000000000000000000, -0.000000000000000000 ) ) ;
#8421 = CARTESIAN_POINT ( 'NONE',  ( 2.299999999999949640, 12.50000000000000000, -4.741630453620015118 ) ) ;
#8422 = DIRECTION ( 'NONE',  ( 0.000000000000000000, 1.000000000000000000, 0.000000000000000000 ) ) ;
#8423 = DIRECTION ( 'NONE',  ( 0.000000000000000000, 1.000000000000000000, 0.000000000000000000 ) ) ;
#8424 = ADVANCED_FACE ( 'NONE', ( #14176 ), #22609, .T. ) ;
#8425 = CYLINDRICAL_SURFACE ( 'NONE', #64526, 7.699999999999999289 ) ;
#8426 = ORIENTED_EDGE ( 'NONE', *, *, #87344, .F. ) ;
#8427 = EDGE_LOOP ( 'NONE', ( #87769, #7196 ) ) ;
#8428 = CARTESIAN_POINT ( 'NONE',  ( -5.450000000000023270, 2.500000000000000000, -2.165063509461101710 ) ) ;
#8429 = LINE ( 'NONE', #96813, #40361 ) ;
#8430 = EDGE_LOOP ( 'NONE', ( #61417, #110873, #79793, #20748 ) ) ;
#8431 = ORIENTED_EDGE ( 'NONE', *, *, #127741, .T. ) ;
#8432 = CARTESIAN_POINT ( 'NONE',  ( 186.5677083336747160, -4.367472073101514418, -7.564683531250002702 ) ) ;
#8433 = CARTESIAN_POINT ( 'NONE',  ( -6.450000000000016165, 2.500000000000000000, 2.611473670974873151 ) ) ;
#8434 = DIRECTION ( 'NONE',  ( -0.000000000000000000, 1.000000000000000000, -0.000000000000000000 ) ) ;
#8435 = DIRECTION ( 'NONE',  ( 0.000000000000000000, 1.000000000000000000, 0.000000000000000000 ) ) ;
#8436 = DIRECTION ( 'NONE',  ( -0.000000000000000000, 1.000000000000000000, -0.000000000000000000 ) ) ;
#8437 = DIRECTION ( 'NONE',  ( 0.000000000000000000, -0.9999939076577903929, 0.003490651415223739937 ) ) ;
#8438 = DIRECTION ( 'NONE',  ( -0.000000000000000000, 1.000000000000000000, -0.000000000000000000 ) ) ;
#8439 = DIRECTION ( 'NONE',  ( 0.000000000000000000, 1.000000000000000000, 0.000000000000000000 ) ) ;
#8440 = AXIS2_PLACEMENT_3D ( 'NONE', #14369, #45154, #62847 ) ;
#8442 = ORIENTED_EDGE ( 'NONE', *, *, #115310, .F. ) ;
#8441 = AXIS2_PLACEMENT_3D ( 'NONE', #10367, #81055, #128885 ) ;
#8443 = EDGE_CURVE ( 'NONE', #37002, #26544, #56672, .T. ) ;
#8444 = VERTEX_POINT ( 'NONE', #55414 ) ;
#8445 = EDGE_LOOP ( 'NONE', ( #41303, #47119, #35176, #39534 ) ) ;
#8446 = ORIENTED_EDGE ( 'NONE', *, *, #39849, .T. ) ;
#8447 = DIRECTION ( 'NONE',  ( -0.000000000000000000, 1.000000000000000000, -0.000000000000000000 ) ) ;
#8448 = DIRECTION ( 'NONE',  ( -0.000000000000000000, -1.000000000000000000, -0.000000000000000000 ) ) ;
#8449 = CIRCLE ( 'NONE', #75356, 0.06509327318403745899 ) ;
#8450 = ADVANCED_FACE ( 'NONE', ( #65868 ), #18367, .T. ) ;
#8451 = ORIENTED_EDGE ( 'NONE', *, *, #93414, .F. ) ;
#8452 = DIRECTION ( 'NONE',  ( -4.274815082592931898E-19, -0.9999939076577903929, -0.003490651415223739937 ) ) ;
#8453 = FACE_OUTER_BOUND ( 'NONE', #27917, .T. ) ;
#8454 = CARTESIAN_POINT ( 'NONE',  ( 1.649999999999951950, 12.50000000000000000, -7.253104124594891289 ) ) ;
#8456 = ORIENTED_EDGE ( 'NONE', *, *, #35563, .T. ) ;
#8455 = CARTESIAN_POINT ( 'NONE',  ( -0.6000000000000323963, 2.500000000000000000, -0.2464101615137759549 ) ) ;
#8457 = EDGE_CURVE ( 'NONE', #117477, #115271, #46228, .T. ) ;
#8458 = EDGE_CURVE ( 'NONE', #75790, #82453, #82949, .T. ) ;
#8459 = ADVANCED_FACE ( 'NONE', ( #24665 ), #58098, .T. ) ;
#8460 = FACE_OUTER_BOUND ( 'NONE', #85640, .T. ) ;
#8461 = ADVANCED_FACE ( 'NONE', ( #3724 ), #99633, .T. ) ;
#8462 = CARTESIAN_POINT ( 'NONE',  ( 9.199999999999915801, 2.500000000000000000, -4.330127018922201643 ) ) ;
#8463 = VECTOR ( 'NONE', #122478, 1000.000000000000000 ) ;
#8464 = ORIENTED_EDGE ( 'NONE', *, *, #129123, .F. ) ;
#8465 = CIRCLE ( 'NONE', #69115, 0.06509327318403745899 ) ;
#8466 = ORIENTED_EDGE ( 'NONE', *, *, #118135, .F. ) ;
#8468 = ORIENTED_EDGE ( 'NONE', *, *, #125947, .T. ) ;
#8467 = EDGE_CURVE ( 'NONE', #121109, #98383, #16100, .T. ) ;
#8469 = CARTESIAN_POINT ( 'NONE',  ( 6.849999999999929479, 2.500000000000000000, 6.841600689897072485 ) ) ;
#8470 = EDGE_CURVE ( 'NONE', #111058, #89282, #44302, .T. ) ;
#8471 = EDGE_CURVE ( 'NONE', #62189, #7899, #92326, .T. ) ;
#8472 = CIRCLE ( 'NONE', #2135, 0.09999999999999982514 ) ;
#8473 = CARTESIAN_POINT ( 'NONE',  ( -10.80000000000000071, 2.500000000000000000, 4.430127018922196847 ) ) ;
#8474 = ADVANCED_FACE ( 'NONE', ( #43679 ), #25415, .T. ) ;
#8475 = EDGE_CURVE ( 'NONE', #30036, #72978, #94044, .T. ) ;
#8476 = VERTEX_POINT ( 'NONE', #84211 ) ;
#8477 = CARTESIAN_POINT ( 'NONE',  ( -10.60000000000000320, 2.500000000000000000, -4.676537180435973440 ) ) ;
#8478 = DIRECTION ( 'NONE',  ( 0.000000000000000000, -0.9999939076577903929, 0.003490651415223739937 ) ) ;
#8479 = CARTESIAN_POINT ( 'NONE',  ( -14.59999999999998366, 2.500000000000000000, -1.084202172485504434E-16 ) ) ;
#8480 = CARTESIAN_POINT ( 'NONE',  ( 10.59999999999990905, 2.500000000000000000, -4.676537180435978769 ) ) ;
#8481 = ADVANCED_FACE ( 'NONE', ( #34503 ), #35903, .T. ) ;
#8482 = VERTEX_POINT ( 'NONE', #39026 ) ;
#8483 = PLANE ( 'NONE',  #85506 ) ;
#8484 = ORIENTED_EDGE ( 'NONE', *, *, #48218, .T. ) ;
#8485 = EDGE_LOOP ( 'NONE', ( #127037, #97002, #22676, #33810 ) ) ;
#8486 = PLANE ( 'NONE',  #106133 ) ;
#8487 = DIRECTION ( 'NONE',  ( 0.000000000000000000, 1.000000000000000000, 0.000000000000000000 ) ) ;
#8488 = FACE_BOUND ( 'NONE', #94727, .T. ) ;
#8489 = DIRECTION ( 'NONE',  ( -4.274815082592931898E-19, -0.9999939076577903929, -0.003490651415223739937 ) ) ;
#8490 = DIRECTION ( 'NONE',  ( 0.000000000000000000, 1.000000000000000000, 0.000000000000000000 ) ) ;
#8491 = CARTESIAN_POINT ( 'NONE',  ( -7.499999999999980460, 12.50000000000000000, 0.06509327318403515528 ) ) ;
#8492 = AXIS2_PLACEMENT_3D ( 'NONE', #34380, #63827, #125315 ) ;
#8494 = EDGE_LOOP ( 'NONE', ( #55014, #66803 ) ) ;
#8493 = AXIS2_PLACEMENT_3D ( 'NONE', #32315, #11991, #12629 ) ;
#8496 = AXIS2_PLACEMENT_3D ( 'NONE', #112916, #101169, #71702 ) ;
#8495 = DIRECTION ( 'NONE',  ( 0.000000000000000000, -0.000000000000000000, 1.000000000000000000 ) ) ;
#8497 = CARTESIAN_POINT ( 'NONE',  ( -5.600000000000020073, 2.500000000000000000, 3.883716857408421319 ) ) ;
#8498 = DIRECTION ( 'NONE',  ( -0.000000000000000000, -1.000000000000000000, -0.000000000000000000 ) ) ;
#8499 = CARTESIAN_POINT ( 'NONE',  ( 6.249999999999930722, 12.50000000000000000, -1.472243186433550122 ) ) ;
#8500 = EDGE_LOOP ( 'NONE', ( #71227, #12603 ) ) ;
#8501 = DIRECTION ( 'NONE',  ( 0.000000000000000000, 0.000000000000000000, 1.000000000000000000 ) ) ;
#8502 = AXIS2_PLACEMENT_3D ( 'NONE', #111338, #89143, #118600 ) ;
#8503 = DIRECTION ( 'NONE',  ( -0.000000000000000000, -1.000000000000000000, -0.000000000000000000 ) ) ;
#8504 = EDGE_LOOP ( 'NONE', ( #92715, #32131 ) ) ;
#8505 = ORIENTED_EDGE ( 'NONE', *, *, #106734, .F. ) ;
#8506 = AXIS2_PLACEMENT_3D ( 'NONE', #67149, #107092, #17416 ) ;
#8507 = FACE_OUTER_BOUND ( 'NONE', #15720, .T. ) ;
#8508 = DIRECTION ( 'NONE',  ( 0.000000000000000000, 0.000000000000000000, 1.000000000000000000 ) ) ;
#8509 = FACE_BOUND ( 'NONE', #49345, .T. ) ;
#8510 = LINE ( 'NONE', #96903, #82840 ) ;
#8511 = EDGE_CURVE ( 'NONE', #13812, #109878, #17393, .T. ) ;
#8512 = ORIENTED_EDGE ( 'NONE', *, *, #103601, .F. ) ;
#8513 = CARTESIAN_POINT ( 'NONE',  ( 162.5000000000000000, -0.5000000000000000000, -7.500000000000005329 ) ) ;
#8514 = EDGE_CURVE ( 'NONE', #93080, #40679, #63087, .T. ) ;
#8515 = ORIENTED_EDGE ( 'NONE', *, *, #14249, .F. ) ;
#8516 = EDGE_LOOP ( 'NONE', ( #120678, #30350, #50604, #102740 ) ) ;
#8517 = DIRECTION ( 'NONE',  ( 0.000000000000000000, 1.000000000000000000, 0.000000000000000000 ) ) ;
#8518 = CARTESIAN_POINT ( 'NONE',  ( 184.1302083336747160, -4.367472073101514418, -7.564683531250002702 ) ) ;
#8519 = ORIENTED_EDGE ( 'NONE', *, *, #40992, .F. ) ;
#8520 = LINE ( 'NONE', #48466, #13452 ) ;
#8521 = DIRECTION ( 'NONE',  ( 0.000000000000000000, 0.000000000000000000, -1.000000000000000000 ) ) ;
#8522 = EDGE_CURVE ( 'NONE', #106872, #41830, #78934, .T. ) ;
#8523 = EDGE_CURVE ( 'NONE', #71810, #88786, #18047, .T. ) ;
#8524 = CARTESIAN_POINT ( 'NONE',  ( 4.399999999999940847, 12.50000000000000000, -3.918623584224389056 ) ) ;
#8525 = CARTESIAN_POINT ( 'NONE',  ( 8.149999999999923972, 2.500000000000000000, -6.941600689897077459 ) ) ;
#8526 = ORIENTED_EDGE ( 'NONE', *, *, #2569, .F. ) ;
#8527 = FACE_OUTER_BOUND ( 'NONE', #42387, .T. ) ;
#8528 = DIRECTION ( 'NONE',  ( 0.000000000000000000, 1.000000000000000000, 0.000000000000000000 ) ) ;
#8529 = DIRECTION ( 'NONE',  ( 0.000000000000000000, -0.9999939076577903929, 0.003490651415223739937 ) ) ;
#8530 = DIRECTION ( 'NONE',  ( 0.000000000000000000, -1.000000000000000000, 0.000000000000000000 ) ) ;
#8531 = ORIENTED_EDGE ( 'NONE', *, *, #49281, .F. ) ;
#8532 = CARTESIAN_POINT ( 'NONE',  ( -8.350000000000013856, 2.500000000000000000, -7.088010851410848190 ) ) ;
#8533 = VERTEX_POINT ( 'NONE', #119470 ) ;
#8534 = CARTESIAN_POINT ( 'NONE',  ( 10.59999999999991260, 2.500000000000000000, 0.4464101615137735513 ) ) ;
#8535 = AXIS2_PLACEMENT_3D ( 'NONE', #4946, #122808, #73063 ) ;
#8536 = ORIENTED_EDGE ( 'NONE', *, *, #18656, .T. ) ;
#8537 = DIRECTION ( 'NONE',  ( -0.000000000000000000, 1.000000000000000000, -0.000000000000000000 ) ) ;
#8538 = AXIS2_PLACEMENT_3D ( 'NONE', #42600, #92979, #72052 ) ;
#8539 = FACE_OUTER_BOUND ( 'NONE', #65931, .T. ) ;
#8540 = DIRECTION ( 'NONE',  ( 0.000000000000000000, 0.000000000000000000, -1.000000000000000000 ) ) ;
#8541 = DIRECTION ( 'NONE',  ( -4.274815082592931898E-19, -0.9999939076577903929, -0.003490651415223739937 ) ) ;
#8542 = EDGE_LOOP ( 'NONE', ( #84074, #5186 ) ) ;
#8543 = CARTESIAN_POINT ( 'NONE',  ( 9.149999999999920419, 2.500000000000000000, 1.472243186433545459 ) ) ;
#8544 = LINE ( 'NONE', #7912, #83625 ) ;
#8545 = CARTESIAN_POINT ( 'NONE',  ( -9.350000000000004974, 2.500000000000000000, 6.048780366869521252 ) ) ;
#8546 = CARTESIAN_POINT ( 'NONE',  ( 184.5260416670080588, -6.551208109652273848, -3.782341765625003571 ) ) ;
#8547 = DIRECTION ( 'NONE',  ( 0.000000000000000000, 0.000000000000000000, -1.000000000000000000 ) ) ;
#8548 = FACE_OUTER_BOUND ( 'NONE', #117629, .T. ) ;
#8550 = EDGE_CURVE ( 'NONE', #76648, #112463, #119517, .T. ) ;
#8549 = CIRCLE ( 'NONE', #85916, 0.06509327318403745899 ) ;
#8551 = VERTEX_POINT ( 'NONE', #48169 ) ;
#8552 = AXIS2_PLACEMENT_3D ( 'NONE', #123448, #115547, #35099 ) ;
#8553 = ORIENTED_EDGE ( 'NONE', *, *, #72074, .F. ) ;
#8554 = DIRECTION ( 'NONE',  ( -0.000000000000000000, -1.000000000000000000, -0.000000000000000000 ) ) ;
#8555 = ORIENTED_EDGE ( 'NONE', *, *, #106937, .F. ) ;
#8556 = CARTESIAN_POINT ( 'NONE',  ( -9.150000000000009237, 2.500000000000000000, 2.165063509461097713 ) ) ;
#8558 = ORIENTED_EDGE ( 'NONE', *, *, #35848, .F. ) ;
#8557 = ORIENTED_EDGE ( 'NONE', *, *, #23867, .F. ) ;
#8559 = EDGE_LOOP ( 'NONE', ( #52526, #97411 ) ) ;
#8560 = CARTESIAN_POINT ( 'NONE',  ( 12.04999999999990479, 12.50000000000000000, 2.099970236277060032 ) ) ;
#8561 = CARTESIAN_POINT ( 'NONE',  ( 6.649999999999929301, 2.500000000000000000, -2.165063509461101710 ) ) ;
#8562 = DIRECTION ( 'NONE',  ( -4.274815082592931898E-19, -0.9999939076577903929, -0.003490651415223739937 ) ) ;
#8563 =( NAMED_UNIT ( * ) SI_UNIT ( $, .STERADIAN. ) SOLID_ANGLE_UNIT ( ) );
#8564 = DIRECTION ( 'NONE',  ( 0.000000000000000000, 1.000000000000000000, 0.000000000000000000 ) ) ;
#8565 = VECTOR ( 'NONE', #122044, 1000.000000000000000 ) ;
#8566 = CARTESIAN_POINT ( 'NONE',  ( 185.8750000000000000, 8.891194145520236347, 5.444286225454521982E-16 ) ) ;
#8567 = ADVANCED_FACE ( 'NONE', ( #6919 ), #97901, .T. ) ;
#8568 = PLANE ( 'NONE',  #91557 ) ;
#8569 = DIRECTION ( 'NONE',  ( -0.000000000000000000, 1.000000000000000000, -0.000000000000000000 ) ) ;
#8570 = EDGE_CURVE ( 'NONE', #114031, #5343, #65123, .T. ) ;
#8571 = CARTESIAN_POINT ( 'NONE',  ( 2.299999999999949640, 12.50000000000000000, -0.4115034346978156399 ) ) ;
#8572 = ORIENTED_EDGE ( 'NONE', *, *, #43928, .T. ) ;
#8573 = ORIENTED_EDGE ( 'NONE', *, *, #77296, .F. ) ;
#8574 = ORIENTED_EDGE ( 'NONE', *, *, #14693, .F. ) ;
#8575 = CARTESIAN_POINT ( 'NONE',  ( -11.89999999999999680, 2.500000000000000000, 0.3464101615137776813 ) ) ;
#8576 = ORIENTED_EDGE ( 'NONE', *, *, #26237, .T. ) ;
#8577 = EDGE_CURVE ( 'NONE', #28877, #108367, #88192, .T. ) ;
#8578 = ORIENTED_EDGE ( 'NONE', *, *, #82982, .T. ) ;
#8579 = CARTESIAN_POINT ( 'NONE',  ( -12.29999999999999361, 12.50000000000000000, 4.048810130592458201 ) ) ;
#8580 = DIRECTION ( 'NONE',  ( 0.000000000000000000, 1.000000000000000000, 0.000000000000000000 ) ) ;
#8581 = CARTESIAN_POINT ( 'NONE',  ( -10.20000000000000462, 12.50000000000000000, 4.676537180435972552 ) ) ;
#8582 = DIRECTION ( 'NONE',  ( 0.000000000000000000, 0.000000000000000000, 1.000000000000000000 ) ) ;
#8583 = CARTESIAN_POINT ( 'NONE',  ( 13.14999999999989733, 2.500000000000000000, -2.511473670974877948 ) ) ;
#8584 = AXIS2_PLACEMENT_3D ( 'NONE', #111970, #32783, #62861 ) ;
#8585 = CARTESIAN_POINT ( 'NONE',  ( 0.3999999999999555023, 2.500000000000000000, 4.430127018922196847 ) ) ;
#8586 = VERTEX_POINT ( 'NONE', #97263 ) ;
#8587 = CONICAL_SURFACE ( 'NONE', #31605, 0.09999999999999999167, 0.003490658503988666988 ) ;
#8588 = DIRECTION ( 'NONE',  ( -4.274815082592931898E-19, -0.9999939076577903929, -0.003490651415223739937 ) ) ;
#8589 = VERTEX_POINT ( 'NONE', #88057 ) ;
#8590 = CARTESIAN_POINT ( 'NONE',  ( 14.39999999999989555, 2.500000000000000000, 0.2464101615137736789 ) ) ;
#8591 = AXIS2_PLACEMENT_3D ( 'NONE', #123120, #113945, #102811 ) ;
#8592 = ORIENTED_EDGE ( 'NONE', *, *, #8047, .T. ) ;
#8593 = CARTESIAN_POINT ( 'NONE',  ( -10.40000000000000213, 12.50000000000000000, -4.265033745738159965 ) ) ;
#8594 = ORIENTED_EDGE ( 'NONE', *, *, #46619, .T. ) ;
#8595 = AXIS2_PLACEMENT_3D ( 'NONE', #15975, #94545, #4226 ) ;
#8596 = ORIENTED_EDGE ( 'NONE', *, *, #110889, .T. ) ;
#8597 = CARTESIAN_POINT ( 'NONE',  ( 11.44999999999990692, 12.50000000000000000, -6.776507416713040577 ) ) ;
#8598 = CARTESIAN_POINT ( 'NONE',  ( -8.150000000000009237, 12.50000000000000000, 6.148780366869520009 ) ) ;
#8599 = EDGE_CURVE ( 'NONE', #113919, #18774, #99408, .T. ) ;
#8600 = DIRECTION ( 'NONE',  ( -4.274815082592931898E-19, -0.9999939076577903929, -0.003490651415223739937 ) ) ;
#8601 = CARTESIAN_POINT ( 'NONE',  ( -10.80000000000000071, 12.50000000000000000, -2.276824562219559311E-15 ) ) ;
#8602 = LINE ( 'NONE', #78676, #93180 ) ;
#8603 = VERTEX_POINT ( 'NONE', #28532 ) ;
#8604 = CARTESIAN_POINT ( 'NONE',  ( 6.049999999999930544, 2.500000000000000000, 2.411473670974873862 ) ) ;
#8605 = CARTESIAN_POINT ( 'NONE',  ( -2.100000000000033396, 2.500000000000000000, 0.6928203230275494784 ) ) ;
#8606 = EDGE_CURVE ( 'NONE', #120306, #85725, #75592, .T. ) ;
#8607 = CARTESIAN_POINT ( 'NONE',  ( -5.200000000000024158, 2.500000000000000000, -4.576537180435977348 ) ) ;
#8608 = EDGE_CURVE ( 'NONE', #38064, #55936, #125762, .T. ) ;
#8609 = LINE ( 'NONE', #129084, #34762 ) ;
#8610 = EDGE_CURVE ( 'NONE', #23183, #62091, #71488, .T. ) ;
#8611 = DIRECTION ( 'NONE',  ( 0.000000000000000000, 1.000000000000000000, 0.000000000000000000 ) ) ;
#8612 = ORIENTED_EDGE ( 'NONE', *, *, #64801, .T. ) ;
#8613 = EDGE_LOOP ( 'NONE', ( #2891, #61345, #125870, #11666 ) ) ;
#8614 = EDGE_CURVE ( 'NONE', #96017, #127371, #69330, .T. ) ;
#8615 = ADVANCED_FACE ( 'NONE', ( #112252 ), #58891, .T. ) ;
#8616 = DIRECTION ( 'NONE',  ( 0.000000000000000000, 0.000000000000000000, 1.000000000000000000 ) ) ;
#8617 = EDGE_CURVE ( 'NONE', #128383, #96759, #110311, .T. ) ;
#8618 = VERTEX_POINT ( 'NONE', #22602 ) ;
#8619 = DIRECTION ( 'NONE',  ( -4.274815082592931898E-19, -0.9999939076577903929, -0.003490651415223739937 ) ) ;
#8620 = AXIS2_PLACEMENT_3D ( 'NONE', #79163, #16329, #126314 ) ;
#8621 = DIRECTION ( 'NONE',  ( 1.000000000000000000, -0.000000000000000000, -0.000000000000000000 ) ) ;
#8622 = AXIS2_PLACEMENT_3D ( 'NONE', #39557, #21161, #19216 ) ;
#8623 = EDGE_CURVE ( 'NONE', #119894, #23306, #120776, .T. ) ;
#8624 = ORIENTED_EDGE ( 'NONE', *, *, #57574, .T. ) ;
#8625 = CARTESIAN_POINT ( 'NONE',  ( 184.5416666666666572, -4.445597072760122614, 7.699999999999998401 ) ) ;
#8626 = CARTESIAN_POINT ( 'NONE',  ( -7.300000000000018474, 12.50000000000000000, -3.918623584224389056 ) ) ;
#8627 = EDGE_CURVE ( 'NONE', #98294, #95448, #113259, .T. ) ;
#8628 = PRESENTATION_STYLE_ASSIGNMENT (( #46012 ) ) ;
#8629 = CARTESIAN_POINT ( 'NONE',  ( -13.29999999999998828, 2.500000000000000000, 4.230127018922196669 ) ) ;
#8630 = EDGE_LOOP ( 'NONE', ( #91027, #77369, #3674, #80074 ) ) ;
#8631 = EDGE_CURVE ( 'NONE', #105260, #8138, #90007, .T. ) ;
#8632 = CONICAL_SURFACE ( 'NONE', #50504, 0.09999999999999982514, 0.003490658503988666988 ) ;
#8633 = FACE_OUTER_BOUND ( 'NONE', #47665, .T. ) ;
#8634 = ORIENTED_EDGE ( 'NONE', *, *, #9047, .T. ) ;
#8635 = PLANE ( 'NONE',  #17159 ) ;
#8636 = CARTESIAN_POINT ( 'NONE',  ( -6.850000000000017408, 2.500000000000000000, -6.841600689897077814 ) ) ;
#8637 = DIRECTION ( 'NONE',  ( 0.000000000000000000, 0.000000000000000000, 1.000000000000000000 ) ) ;
#8638 = AXIS2_PLACEMENT_3D ( 'NONE', #87526, #427, #127469 ) ;
#8639 = CIRCLE ( 'NONE', #81814, 0.1000000000000000472 ) ;
#8640 = ORIENTED_EDGE ( 'NONE', *, *, #85471, .T. ) ;
#8641 = DIRECTION ( 'NONE',  ( 0.000000000000000000, 0.000000000000000000, 1.000000000000000000 ) ) ;
#8642 = VECTOR ( 'NONE', #111006, 1000.000000000000000 ) ;
#8643 = EDGE_LOOP ( 'NONE', ( #55002, #87651, #59079, #66352 ) ) ;
#8644 = DIRECTION ( 'NONE',  ( 0.000000000000000000, 0.000000000000000000, 1.000000000000000000 ) ) ;
#8645 = DIRECTION ( 'NONE',  ( 0.000000000000000000, 0.000000000000000000, 1.000000000000000000 ) ) ;
#8646 = AXIS2_PLACEMENT_3D ( 'NONE', #114278, #95934, #54699 ) ;
#8647 = CARTESIAN_POINT ( 'NONE',  ( -12.09999999999999609, 12.50000000000000000, -4.330127018922198978 ) ) ;
#8648 = ORIENTED_EDGE ( 'NONE', *, *, #41160, .T. ) ;
#8649 = DIRECTION ( 'NONE',  ( 0.000000000000000000, -0.000000000000000000, 1.000000000000000000 ) ) ;
#8650 = DIRECTION ( 'NONE',  ( -0.000000000000000000, -1.000000000000000000, -0.000000000000000000 ) ) ;
#8651 = AXIS2_PLACEMENT_3D ( 'NONE', #6962, #65905, #107110 ) ;
#8652 = ORIENTED_EDGE ( 'NONE', *, *, #36983, .T. ) ;
#8653 = DIRECTION ( 'NONE',  ( -0.000000000000000000, -1.000000000000000000, -0.000000000000000000 ) ) ;
#8654 = VERTEX_POINT ( 'NONE', #21952 ) ;
#8655 = DIRECTION ( 'NONE',  ( 0.000000000000000000, 1.000000000000000000, 0.000000000000000000 ) ) ;
#8656 = EDGE_CURVE ( 'NONE', #47134, #93656, #6617, .T. ) ;
#8657 = ORIENTED_EDGE ( 'NONE', *, *, #48864, .T. ) ;
#8658 = CARTESIAN_POINT ( 'NONE',  ( 12.89999999999990088, 2.500000000000000000, 4.430127018922196847 ) ) ;
#8659 = CARTESIAN_POINT ( 'NONE',  ( -6.050000000000017586, 12.50000000000000000, 1.753560074763284016 ) ) ;
#8660 = ADVANCED_FACE ( 'NONE', ( #42229 ), #62520, .T. ) ;
#8661 = VERTEX_POINT ( 'NONE', #11462 ) ;
#8662 = EDGE_LOOP ( 'NONE', ( #79028, #23814, #108464, #32036 ) ) ;
#8663 = LINE ( 'NONE', #127194, #128283 ) ;
#8664 = DIRECTION ( 'NONE',  ( 0.000000000000000000, 1.000000000000000000, 0.000000000000000000 ) ) ;
#8665 = ORIENTED_EDGE ( 'NONE', *, *, #66679, .F. ) ;
#8666 = CARTESIAN_POINT ( 'NONE',  ( -12.69999999999999396, 2.500000000000000000, 0.3464101615137776813 ) ) ;
#8667 = CARTESIAN_POINT ( 'NONE',  ( -7.700000000000010836, 2.500000000000000000, 3.983716857408420964 ) ) ;
#8668 = DIRECTION ( 'NONE',  ( -0.000000000000000000, 1.000000000000000000, -0.000000000000000000 ) ) ;
#8669 = VECTOR ( 'NONE', #128143, 1000.000000000000000 ) ;
#8670 = CARTESIAN_POINT ( 'NONE',  ( 107.3283734746308227, 7.144069872249539266, 4.965747202897751400 ) ) ;
#8671 = LINE ( 'NONE', #17192, #78165 ) ;
#8672 = AXIS2_PLACEMENT_3D ( 'NONE', #46285, #87489, #17460 ) ;
#8673 = VECTOR ( 'NONE', #20528, 1000.000000000000000 ) ;
#8674 = CARTESIAN_POINT ( 'NONE',  ( 4.399999999999940847, 2.500000000000000000, -4.776537180435977525 ) ) ;
#8675 = DIRECTION ( 'NONE',  ( 0.000000000000000000, 0.000000000000000000, -1.000000000000000000 ) ) ;
#8676 = CONICAL_SURFACE ( 'NONE', #2423, 0.1000000000000002554, 0.003490658503988666988 ) ;
#8677 = ORIENTED_EDGE ( 'NONE', *, *, #93318, .F. ) ;
#8679 = EDGE_LOOP ( 'NONE', ( #96736, #79112, #68934, #100287 ) ) ;
#8678 = CIRCLE ( 'NONE', #102691, 0.06509327318403745899 ) ;
#8680 = EDGE_LOOP ( 'NONE', ( #89388, #37217 ) ) ;
#8681 = ORIENTED_EDGE ( 'NONE', *, *, #128325, .T. ) ;
#8682 = LINE ( 'NONE', #78102, #39177 ) ;
#8683 = DIRECTION ( 'NONE',  ( 0.000000000000000000, 1.000000000000000000, 0.000000000000000000 ) ) ;
#8684 = VECTOR ( 'NONE', #86795, 1000.000000000000000 ) ;
#8685 = LINE ( 'NONE', #48639, #42703 ) ;
#8686 = ORIENTED_EDGE ( 'NONE', *, *, #118244, .F. ) ;
#8687 = FACE_BOUND ( 'NONE', #107867, .T. ) ;
#8688 = ORIENTED_EDGE ( 'NONE', *, *, #108689, .T. ) ;
#8689 = CARTESIAN_POINT ( 'NONE',  ( -6.850000000000013856, 12.50000000000000000, 6.213873640053559022 ) ) ;
#8690 = FACE_OUTER_BOUND ( 'NONE', #17826, .T. ) ;
#8691 = AXIS2_PLACEMENT_3D ( 'NONE', #57975, #48805, #97883 ) ;
#8692 = DIRECTION ( 'NONE',  ( 0.000000000000000000, -0.9999939076577903929, 0.003490651415223739937 ) ) ;
#8693 = DIRECTION ( 'NONE',  ( -0.000000000000000000, 1.000000000000000000, -0.000000000000000000 ) ) ;
#8694 = LINE ( 'NONE', #86629, #51400 ) ;
#8695 = CARTESIAN_POINT ( 'NONE',  ( -13.34999999999999076, 2.500000000000000000, 2.065063509461101621 ) ) ;
#8696 = CARTESIAN_POINT ( 'NONE',  ( 2.099999999999948574, 2.500000000000000000, 4.230127018922196669 ) ) ;
#8697 = CARTESIAN_POINT ( 'NONE',  ( -0.4500000000000402012, 2.500000000000000000, 6.595190528383296780 ) ) ;
#8698 = DIRECTION ( 'NONE',  ( 0.000000000000000000, 0.000000000000000000, 1.000000000000000000 ) ) ;
#8699 = FACE_OUTER_BOUND ( 'NONE', #67664, .T. ) ;
#8700 = EDGE_CURVE ( 'NONE', #74521, #80440, #30486, .T. ) ;
#8701 = EDGE_LOOP ( 'NONE', ( #59558, #62667 ) ) ;
#8702 = ORIENTED_EDGE ( 'NONE', *, *, #53412, .F. ) ;
#8703 = ORIENTED_EDGE ( 'NONE', *, *, #27520, .T. ) ;
#8704 = EDGE_LOOP ( 'NONE', ( #70978, #52290 ) ) ;
#8705 = DIRECTION ( 'NONE',  ( -0.000000000000000000, -1.000000000000000000, -0.000000000000000000 ) ) ;
#8706 = B_SPLINE_CURVE_WITH_KNOTS ( 'NONE', 3,
 ( #104825, #15149, #30494, #40961, #80867, #31135, #71040, #21284, #61221, #101148, #11468, #36115 ),
 .UNSPECIFIED., .F., .F.,
 ( 4, 2, 2, 2, 2, 4 ),
 ( 0.000000000000000000, 0.001300228439403514720, 0.002600456878807029439, 0.003900685318210543942, 0.004550799537912301844, 0.005200913757614058879 ),
 .UNSPECIFIED. ) ;
#8707 = CARTESIAN_POINT ( 'NONE',  ( 15.59999999999988951, 2.500000000000000000, -0.3464101615137783474 ) ) ;
#8709 = EDGE_LOOP ( 'NONE', ( #68552, #21572 ) ) ;
#8708 = ORIENTED_EDGE ( 'NONE', *, *, #75077, .F. ) ;
#8710 = ORIENTED_EDGE ( 'NONE', *, *, #61674, .T. ) ;
#8711 = DIRECTION ( 'NONE',  ( 0.000000000000000000, 1.000000000000000000, 0.000000000000000000 ) ) ;
#8712 = AXIS2_PLACEMENT_3D ( 'NONE', #60795, #29409, #100703 ) ;
#8713 = EDGE_CURVE ( 'NONE', #64779, #121936, #106982, .T. ) ;
#8714 = PLANE ( 'NONE',  #128221 ) ;
#8715 = FACE_OUTER_BOUND ( 'NONE', #121087, .T. ) ;
#8716 = DIRECTION ( 'NONE',  ( 0.000000000000000000, 1.000000000000000000, 0.000000000000000000 ) ) ;
#8717 = CARTESIAN_POINT ( 'NONE',  ( -5.400000000000019895, 2.500000000000000000, -0.6928203230275541413 ) ) ;
#8718 = CARTESIAN_POINT ( 'NONE',  ( 0.3999999999999628852, 2.500000000000000000, 0.5928203230275517210 ) ) ;
#8719 = ADVANCED_FACE ( 'NONE', ( #92608 ), #23362, .T. ) ;
#8720 = DIRECTION ( 'NONE',  ( 0.000000000000000000, 1.000000000000000000, 0.000000000000000000 ) ) ;
#8721 = ADVANCED_FACE ( 'NONE', ( #1002 ), #102781, .T. ) ;
#8722 = EDGE_LOOP ( 'NONE', ( #24846, #16195 ) ) ;
#8723 = AXIS2_PLACEMENT_3D ( 'NONE', #94957, #5894, #45209 ) ;
#8724 = AXIS2_PLACEMENT_3D ( 'NONE', #90033, #120797, #41619 ) ;
#8725 = DIRECTION ( 'NONE',  ( 0.000000000000000000, -0.9999939076577903929, 0.003490651415223739937 ) ) ;
#8726 = ORIENTED_EDGE ( 'NONE', *, *, #118709, .F. ) ;
#8727 = VERTEX_POINT ( 'NONE', #12104 ) ;
#8728 = CONICAL_SURFACE ( 'NONE', #37990, 0.09999999999999999167, 0.003490658503988666988 ) ;
#8729 = ORIENTED_EDGE ( 'NONE', *, *, #5321, .T. ) ;
#8730 = AXIS2_PLACEMENT_3D ( 'NONE', #65553, #73431, #36105 ) ;
#8731 = DIRECTION ( 'NONE',  ( 0.000000000000000000, 0.000000000000000000, 1.000000000000000000 ) ) ;
#8732 = VERTEX_POINT ( 'NONE', #31763 ) ;
#8733 = EDGE_CURVE ( 'NONE', #4409, #71397, #12734, .T. ) ;
#8734 = EDGE_LOOP ( 'NONE', ( #123850, #4764 ) ) ;
#8735 = AXIS2_PLACEMENT_3D ( 'NONE', #15402, #105074, #94616 ) ;
#8736 = DIRECTION ( 'NONE',  ( 0.000000000000000000, 0.000000000000000000, -1.000000000000000000 ) ) ;
#8737 = AXIS2_PLACEMENT_3D ( 'NONE', #94474, #55846, #72918 ) ;
#8738 = DIRECTION ( 'NONE',  ( 0.000000000000000000, 0.000000000000000000, -1.000000000000000000 ) ) ;
#8739 = DIRECTION ( 'NONE',  ( 0.000000000000000000, 0.000000000000000000, 1.000000000000000000 ) ) ;
#8740 = FACE_OUTER_BOUND ( 'NONE', #118935, .T. ) ;
#8741 = VECTOR ( 'NONE', #75485, 1000.000000000000000 ) ;
#8742 = AXIS2_PLACEMENT_3D ( 'NONE', #62382, #102301, #60461 ) ;
#8743 = DIRECTION ( 'NONE',  ( 0.000000000000000000, 1.000000000000000000, 0.000000000000000000 ) ) ;
#8744 = VECTOR ( 'NONE', #82759, 1000.000000000000000 ) ;
#8745 = EDGE_LOOP ( 'NONE', ( #103824, #55372 ) ) ;
#8746 = CARTESIAN_POINT ( 'NONE',  ( -11.64999999999999680, 2.500000000000000000, -2.165063509461097713 ) ) ;
#8747 = VERTEX_POINT ( 'NONE', #91315 ) ;
#8748 = DIRECTION ( 'NONE',  ( -0.000000000000000000, -1.000000000000000000, -0.000000000000000000 ) ) ;
#8749 = ORIENTED_EDGE ( 'NONE', *, *, #13825, .F. ) ;
#8750 = CARTESIAN_POINT ( 'NONE',  ( 111.3045913714602477, 7.846616099438112890, 3.765819408771217347 ) ) ;
#8751 = CIRCLE ( 'NONE', #60993, 0.1000000000000002554 ) ;
#8752 = DIRECTION ( 'NONE',  ( -0.000000000000000000, -1.000000000000000000, -0.000000000000000000 ) ) ;
#8753 = B_SPLINE_CURVE_WITH_KNOTS ( 'NONE', 3,
 ( #126159, #96050, #65289, #46298, #16815, #115684, #74485, #85586 ),
 .UNSPECIFIED., .F., .F.,
 ( 4, 2, 2, 4 ),
 ( 0.002994103107820000886, 0.003957537843903918655, 0.004920972579987836423, 0.006847842052155671960 ),
 .UNSPECIFIED. ) ;
#8754 = ORIENTED_EDGE ( 'NONE', *, *, #57411, .F. ) ;
#8755 = CARTESIAN_POINT ( 'NONE',  ( 8.749999999999920064, 2.500000000000000000, -2.757883832488654097 ) ) ;
#8756 = CARTESIAN_POINT ( 'NONE',  ( 9.599999999999914380, 2.500000000000000000, 5.122947341949749323 ) ) ;
#8757 = VERTEX_POINT ( 'NONE', #10789 ) ;
#8758 = ADVANCED_FACE ( 'NONE', ( #52679 ), #46353, .T. ) ;
#8759 = CARTESIAN_POINT ( 'NONE',  ( -15.39999999999998082, 2.500000000000000000, 0.5928203230275517210 ) ) ;
#8760 = ORIENTED_EDGE ( 'NONE', *, *, #51701, .F. ) ;
#8761 = EDGE_LOOP ( 'NONE', ( #40648, #78146, #111751, #45036 ) ) ;
#8762 = DIRECTION ( 'NONE',  ( 0.000000000000000000, 0.000000000000000000, 1.000000000000000000 ) ) ;
#8763 = DIRECTION ( 'NONE',  ( 0.000000000000000000, 0.000000000000000000, 1.000000000000000000 ) ) ;
#8764 = EDGE_CURVE ( 'NONE', #55169, #87449, #96512, .T. ) ;
#8765 = CARTESIAN_POINT ( 'NONE',  ( 185.7135416670080588, 4.367472073101518859, -7.564683531249999149 ) ) ;
#8766 = CARTESIAN_POINT ( 'NONE',  ( 9.149999999999920419, 12.50000000000000000, 1.472243186433545459 ) ) ;
#8767 = ADVANCED_FACE ( 'NONE', ( #90665 ), #88102, .T. ) ;
#8768 = CARTESIAN_POINT ( 'NONE',  ( 1.849999999999949685, 12.50000000000000000, 1.818653347947321475 ) ) ;
#8769 = ORIENTED_EDGE ( 'NONE', *, *, #103114, .F. ) ;
#8770 = LINE ( 'NONE', #10086, #36290 ) ;
#8771 = CIRCLE ( 'NONE', #15019, 0.1000000000000002554 ) ;
#8772 = CIRCLE ( 'NONE', #27638, 0.1000000000000002554 ) ;
#8773 = ADVANCED_FACE ( 'NONE', ( #110937 ), #25510, .T. ) ;
#8774 = VECTOR ( 'NONE', #70115, 1000.000000000000000 ) ;
#8775 = EDGE_CURVE ( 'NONE', #43807, #53996, #104842, .T. ) ;
#8776 = ADVANCED_FACE ( 'NONE', ( #14027 ), #74259, .T. ) ;
#8777 = EDGE_CURVE ( 'NONE', #109700, #81402, #27651, .T. ) ;
#8778 = VERTEX_POINT ( 'NONE', #63144 ) ;
#8779 = CARTESIAN_POINT ( 'NONE',  ( 0.6499999999999561684, 2.500000000000000000, 2.511473670974873507 ) ) ;
#8780 = DIRECTION ( 'NONE',  ( -0.000000000000000000, 1.000000000000000000, -0.000000000000000000 ) ) ;
#8781 = AXIS2_PLACEMENT_3D ( 'NONE', #127480, #75157, #26697 ) ;
#8782 = AXIS2_PLACEMENT_3D ( 'NONE', #72075, #83178, #32153 ) ;
#8783 = VECTOR ( 'NONE', #82813, 1000.000000000000000 ) ;
#8784 = ORIENTED_EDGE ( 'NONE', *, *, #13776, .T. ) ;
#8785 = ADVANCED_FACE ( 'NONE', ( #63801 ), #96610, .T. ) ;
#8786 = AXIS2_PLACEMENT_3D ( 'NONE', #25144, #115440, #6143 ) ;
#8787 = CIRCLE ( 'NONE', #121666, 0.06509327318403745899 ) ;
#8788 = CARTESIAN_POINT ( 'NONE',  ( 7.699999999999923794, 2.500000000000000000, -0.4464101615137783252 ) ) ;
#8789 = CARTESIAN_POINT ( 'NONE',  ( 8.549999999999922551, 2.500000000000000000, 2.511473670974873507 ) ) ;
#8790 = DIRECTION ( 'NONE',  ( 0.000000000000000000, 0.000000000000000000, 1.000000000000000000 ) ) ;
#8791 = CARTESIAN_POINT ( 'NONE',  ( -11.64999999999999680, 12.50000000000000000, -2.922977105672687426 ) ) ;
#8792 = PLANE ( 'NONE',  #70436 ) ;
#8793 = ORIENTED_EDGE ( 'NONE', *, *, #58941, .T. ) ;
#8794 = EDGE_CURVE ( 'NONE', #103548, #76584, #92419, .T. ) ;
#8795 = VECTOR ( 'NONE', #83647, 1000.000000000000000 ) ;
#8796 = FACE_OUTER_BOUND ( 'NONE', #3440, .T. ) ;
#8797 = DIRECTION ( 'NONE',  ( 0.000000000000000000, 0.000000000000000000, 1.000000000000000000 ) ) ;
#8798 = ORIENTED_EDGE ( 'NONE', *, *, #120900, .F. ) ;
#8799 = CARTESIAN_POINT ( 'NONE',  ( -8.950000000000008171, 2.500000000000000000, -2.511473670974877948 ) ) ;
#8800 = ORIENTED_EDGE ( 'NONE', *, *, #6353, .T. ) ;
#8801 = ORIENTED_EDGE ( 'NONE', *, *, #63503, .F. ) ;
#8802 = CARTESIAN_POINT ( 'NONE',  ( 127.5000000000000000, -5.000000000000000000, -1.999999999999998224 ) ) ;
#8803 = ORIENTED_EDGE ( 'NONE', *, *, #63561, .T. ) ;
#8804 = CARTESIAN_POINT ( 'NONE',  ( 187.5000000000000000, 0.000000000000000000, 0.000000000000000000 ) ) ;
#8805 = CARTESIAN_POINT ( 'NONE',  ( -6.050000000000017586, 2.500000000000000000, 1.718653347947321386 ) ) ;
#8806 = CIRCLE ( 'NONE', #17104, 0.06509327318403745899 ) ;
#8807 = EDGE_LOOP ( 'NONE', ( #72916, #792, #68472, #109596 ) ) ;
#8808 = DIRECTION ( 'NONE',  ( 0.000000000000000000, 0.000000000000000000, -1.000000000000000000 ) ) ;
#8810 = ORIENTED_EDGE ( 'NONE', *, *, #95497, .T. ) ;
#8809 = DIRECTION ( 'NONE',  ( -0.000000000000000000, -1.000000000000000000, -0.000000000000000000 ) ) ;
#8811 = CARTESIAN_POINT ( 'NONE',  ( 175.5000000000000000, 0.000000000000000000, 0.000000000000000000 ) ) ;
#8812 = FACE_OUTER_BOUND ( 'NONE', #43255, .T. ) ;
#8813 = AXIS2_PLACEMENT_3D ( 'NONE', #31222, #91410, #122175 ) ;
#8814 = ORIENTED_EDGE ( 'NONE', *, *, #20669, .T. ) ;
#8815 = CIRCLE ( 'NONE', #48557, 0.1000000000000002554 ) ;
#8816 = AXIS2_PLACEMENT_3D ( 'NONE', #125800, #106810, #17114 ) ;
#8817 = AXIS2_PLACEMENT_3D ( 'NONE', #73030, #23942, #66267 ) ;
#8819 = VERTEX_POINT ( 'NONE', #113532 ) ;
#8818 = EDGE_CURVE ( 'NONE', #4150, #7088, #4852, .T. ) ;
#8820 = EDGE_LOOP ( 'NONE', ( #117894, #46706 ) ) ;
#8821 = CARTESIAN_POINT ( 'NONE',  ( -4.600000000000024514, 2.500000000000000000, -0.6928203230275542523 ) ) ;
#8822 = DIRECTION ( 'NONE',  ( 0.000000000000000000, -0.9999939076577903929, 0.003490651415223739937 ) ) ;
#8823 = DIRECTION ( 'NONE',  ( 0.000000000000000000, -0.000000000000000000, 1.000000000000000000 ) ) ;
#8824 = FACE_BOUND ( 'NONE', #57735, .T. ) ;
#8825 = ORIENTED_EDGE ( 'NONE', *, *, #5774, .F. ) ;
#8826 = CARTESIAN_POINT ( 'NONE',  ( 5.849999999999932143, 2.500000000000000000, 2.065063509461097624 ) ) ;
#8827 = CARTESIAN_POINT ( 'NONE',  ( -0.6000000000000383915, 2.500000000000000000, -4.676537180435977881 ) ) ;
#8828 = AXIS2_PLACEMENT_3D ( 'NONE', #66133, #7853, #56309 ) ;
#8829 = ORIENTED_EDGE ( 'NONE', *, *, #59469, .T. ) ;
#8830 = CIRCLE ( 'NONE', #6758, 0.1000000000000002554 ) ;
#8831 = ADVANCED_FACE ( 'NONE', ( #85360 ), #56894, .T. ) ;
#8832 = LINE ( 'NONE', #48785, #117620 ) ;
#8833 = PLANE ( 'NONE',  #11542 ) ;
#8834 = AXIS2_PLACEMENT_3D ( 'NONE', #91028, #111967, #58 ) ;
#8835 = VECTOR ( 'NONE', #24354, 1000.000000000000000 ) ;
#8836 = FACE_OUTER_BOUND ( 'NONE', #78661, .T. ) ;
#8837 = CARTESIAN_POINT ( 'NONE',  ( 8.349999999999919709, 12.50000000000000000, -1.537336459617587581 ) ) ;
#8838 = FACE_OUTER_BOUND ( 'NONE', #87394, .T. ) ;
#8839 = DIRECTION ( 'NONE',  ( 0.000000000000000000, 1.000000000000000000, 0.000000000000000000 ) ) ;
#8840 = AXIS2_PLACEMENT_3D ( 'NONE', #88355, #128323, #51690 ) ;
#8841 = DIRECTION ( 'NONE',  ( -0.000000000000000000, 1.000000000000000000, -0.000000000000000000 ) ) ;
#8842 = VERTEX_POINT ( 'NONE', #125916 ) ;
#8843 = CIRCLE ( 'NONE', #46503, 0.1000000000000002554 ) ;
#8844 = VERTEX_POINT ( 'NONE', #55894 ) ;
#8845 = EDGE_LOOP ( 'NONE', ( #96616, #61863, #98127, #52050 ) ) ;
#8846 = ORIENTED_EDGE ( 'NONE', *, *, #116653, .T. ) ;
#8847 = ORIENTED_EDGE ( 'NONE', *, *, #69404, .F. ) ;
#8848 = CARTESIAN_POINT ( 'NONE',  ( -8.150000000000012790, 12.50000000000000000, -1.818653347947326138 ) ) ;
#8849 = DIRECTION ( 'NONE',  ( -0.000000000000000000, 1.000000000000000000, -0.000000000000000000 ) ) ;
#8850 = ORIENTED_EDGE ( 'NONE', *, *, #2427, .T. ) ;
#8851 = FACE_BOUND ( 'NONE', #69460, .T. ) ;
#8852 = FACE_OUTER_BOUND ( 'NONE', #46664, .T. ) ;
#8853 = CARTESIAN_POINT ( 'NONE',  ( -8.550000000000011369, 12.50000000000000000, 1.883746621131358934 ) ) ;
#8854 = DIRECTION ( 'NONE',  ( 0.000000000000000000, 0.000000000000000000, 1.000000000000000000 ) ) ;
#8855 = FACE_OUTER_BOUND ( 'NONE', #62365, .T. ) ;
#8856 = DIRECTION ( 'NONE',  ( 0.000000000000000000, 0.000000000000000000, 1.000000000000000000 ) ) ;
#8857 = ORIENTED_EDGE ( 'NONE', *, *, #87078, .T. ) ;
#8858 = EDGE_LOOP ( 'NONE', ( #113677, #10481 ) ) ;
#8859 = EDGE_LOOP ( 'NONE', ( #64817, #71563 ) ) ;
#8860 = AXIS2_PLACEMENT_3D ( 'NONE', #15428, #29157, #101099 ) ;
#8861 = EDGE_LOOP ( 'NONE', ( #33621, #107525, #11255, #65914 ) ) ;
#8862 = CIRCLE ( 'NONE', #2606, 0.06509327318403745899 ) ;
#8863 = CARTESIAN_POINT ( 'NONE',  ( -1.650000000000034772, 12.50000000000000000, 6.560283801567334372 ) ) ;
#8864 = CIRCLE ( 'NONE', #557, 0.06509327318403745899 ) ;
#8865 = CARTESIAN_POINT ( 'NONE',  ( 4.999999999999938716, 12.50000000000000000, -5.022947341949754119 ) ) ;
#8866 = CARTESIAN_POINT ( 'NONE',  ( -5.400000000000024336, 2.500000000000000000, -3.637306695894650055 ) ) ;
#8867 = ORIENTED_EDGE ( 'NONE', *, *, #121327, .F. ) ;
#8868 = DIRECTION ( 'NONE',  ( 0.000000000000000000, 0.000000000000000000, -1.000000000000000000 ) ) ;
#8869 = EDGE_CURVE ( 'NONE', #122246, #46899, #4655, .T. ) ;
#8870 = LINE ( 'NONE', #39032, #36546 ) ;
#8871 = CONICAL_SURFACE ( 'NONE', #25591, 0.09999999999999982514, 0.003490658503988666988 ) ;
#8872 = AXIS2_PLACEMENT_3D ( 'NONE', #95415, #105228, #97340 ) ;
#8873 = CIRCLE ( 'NONE', #25594, 0.1000000000000002554 ) ;
#8874 = DIRECTION ( 'NONE',  ( 0.000000000000000000, -0.9999939076577903929, 0.003490651415223739937 ) ) ;
#8875 = CARTESIAN_POINT ( 'NONE',  ( 185.1510416670080872, 4.367472073101518859, -7.564683531249999149 ) ) ;
#8876 = DIRECTION ( 'NONE',  ( -0.000000000000000000, -1.000000000000000000, -0.000000000000000000 ) ) ;
#8877 = CARTESIAN_POINT ( 'NONE',  ( 11.24999999999994493, 2.500000000000000000, 6.495190528383297135 ) ) ;
#8878 = AXIS2_PLACEMENT_3D ( 'NONE', #91165, #22447, #59803 ) ;
#8879 = ADVANCED_FACE ( 'NONE', ( #94531 ), #93903, .T. ) ;
#8880 = CIRCLE ( 'NONE', #59077, 0.1000000000000002554 ) ;
#8881 = EDGE_CURVE ( 'NONE', #88669, #128715, #7356, .T. ) ;
#8882 = DIRECTION ( 'NONE',  ( 0.000000000000000000, -0.000000000000000000, 1.000000000000000000 ) ) ;
#8883 = ADVANCED_FACE ( 'NONE', ( #124650 ), #86141, .T. ) ;
#8884 = ORIENTED_EDGE ( 'NONE', *, *, #83856, .T. ) ;
#8885 = CARTESIAN_POINT ( 'NONE',  ( 14.14999999999989377, 12.50000000000000000, -2.922977105672691422 ) ) ;
#8886 = AXIS2_PLACEMENT_3D ( 'NONE', #48225, #50178, #57407 ) ;
#8887 = ORIENTED_EDGE ( 'NONE', *, *, #13023, .F. ) ;
#8888 = ORIENTED_EDGE ( 'NONE', *, *, #115363, .F. ) ;
#8889 = DIRECTION ( 'NONE',  ( 0.000000000000000000, 1.000000000000000000, 0.000000000000000000 ) ) ;
#8890 = EDGE_CURVE ( 'NONE', #7809, #65690, #107081, .T. ) ;
#8891 = DIRECTION ( 'NONE',  ( -0.000000000000000000, 1.000000000000000000, -0.000000000000000000 ) ) ;
#8892 = DIRECTION ( 'NONE',  ( 0.000000000000000000, -0.000000000000000000, 1.000000000000000000 ) ) ;
#8893 = EDGE_CURVE ( 'NONE', #67022, #69080, #73635, .T. ) ;
#8894 = ORIENTED_EDGE ( 'NONE', *, *, #114161, .T. ) ;
#8895 = EDGE_LOOP ( 'NONE', ( #31628, #102122, #108395, #118547 ) ) ;
#8896 = AXIS2_PLACEMENT_3D ( 'NONE', #126007, #116189, #26533 ) ;
#8897 = CARTESIAN_POINT ( 'NONE',  ( 5.399999999999936406, 2.500000000000000000, -3.537306695894649966 ) ) ;
#8898 = FACE_OUTER_BOUND ( 'NONE', #28262, .T. ) ;
#8899 = EDGE_LOOP ( 'NONE', ( #77896, #127489 ) ) ;
#8900 = EDGE_LOOP ( 'NONE', ( #55225, #38942 ) ) ;
#8901 = CARTESIAN_POINT ( 'NONE',  ( 0.8499999999999557909, 2.500000000000000000, -7.288010851410854585 ) ) ;
#8903 = EDGE_LOOP ( 'NONE', ( #44443, #62662 ) ) ;
#8902 = CIRCLE ( 'NONE', #79928, 0.06509327318403745899 ) ;
#8904 = DIRECTION ( 'NONE',  ( 0.000000000000000000, 0.000000000000000000, 1.000000000000000000 ) ) ;
#8905 = AXIS2_PLACEMENT_3D ( 'NONE', #46857, #86760, #75021 ) ;
#8906 = AXIS2_PLACEMENT_3D ( 'NONE', #122533, #70850, #93710 ) ;
#8907 = ORIENTED_EDGE ( 'NONE', *, *, #61142, .T. ) ;
#8908 = DIRECTION ( 'NONE',  ( 0.000000000000000000, 0.000000000000000000, 1.000000000000000000 ) ) ;
#8909 = DIRECTION ( 'NONE',  ( -0.000000000000000000, -1.000000000000000000, -0.000000000000000000 ) ) ;
#8910 = CARTESIAN_POINT ( 'NONE',  ( 1.649999999999950617, 2.500000000000000000, 2.165063509461097713 ) ) ;
#8911 = CARTESIAN_POINT ( 'NONE',  ( 1.649999999999950617, 12.50000000000000000, 2.230156782645134950 ) ) ;
#8912 = ORIENTED_EDGE ( 'NONE', *, *, #55033, .F. ) ;
#8913 = CONICAL_SURFACE ( 'NONE', #98801, 0.1000000000000000472, 0.003490658503988666988 ) ;
#8914 = AXIS2_PLACEMENT_3D ( 'NONE', #120611, #61706, #30318 ) ;
#8915 = DIRECTION ( 'NONE',  ( 0.000000000000000000, 0.000000000000000000, 1.000000000000000000 ) ) ;
#8916 = AXIS2_PLACEMENT_3D ( 'NONE', #4114, #74811, #42805 ) ;
#8917 = ORIENTED_EDGE ( 'NONE', *, *, #71459, .F. ) ;
#8918 = ORIENTED_EDGE ( 'NONE', *, *, #36264, .F. ) ;
#8919 = DIRECTION ( 'NONE',  ( 0.000000000000000000, 1.000000000000000000, 0.000000000000000000 ) ) ;
#8920 = LINE ( 'NONE', #96652, #67926 ) ;
#8921 = LINE ( 'NONE', #39074, #40702 ) ;
#8922 = CARTESIAN_POINT ( 'NONE',  ( -1.450000000000035483, 2.500000000000000000, 6.248780366869521430 ) ) ;
#8923 = CIRCLE ( 'NONE', #125994, 0.06509327318403745899 ) ;
#8924 = CARTESIAN_POINT ( 'NONE',  ( 8.099999999999921485, 12.50000000000000000, 0.4115034346978109769 ) ) ;
#8925 = DIRECTION ( 'NONE',  ( 0.000000000000000000, 0.000000000000000000, -1.000000000000000000 ) ) ;
#8926 = DIRECTION ( 'NONE',  ( -0.000000000000000000, -1.000000000000000000, -0.000000000000000000 ) ) ;
#8927 = CARTESIAN_POINT ( 'NONE',  ( -8.749999999999976907, 2.500000000000000000, -6.595190528383296780 ) ) ;
#8928 = AXIS2_PLACEMENT_3D ( 'NONE', #73282, #102111, #70712 ) ;
#8929 = CARTESIAN_POINT ( 'NONE',  ( 3.149999999999942624, 12.50000000000000000, 6.148780366869520897 ) ) ;
#8930 = ADVANCED_FACE ( 'NONE', ( #65716 ), #105655, .T. ) ;
#8931 = ADVANCED_FACE ( 'NONE', ( #54594 ), #44807, .T. ) ;
#8932 = AXIS2_PLACEMENT_3D ( 'NONE', #23496, #73893, #94175 ) ;
#8933 = EDGE_CURVE ( 'NONE', #81692, #44808, #17174, .T. ) ;
#8934 = CARTESIAN_POINT ( 'NONE',  ( 8.299999999999922551, 2.500000000000000000, 0.09999999999999761857 ) ) ;
#8935 = VECTOR ( 'NONE', #81638, 1000.000000000000114 ) ;
#8936 = ORIENTED_EDGE ( 'NONE', *, *, #74247, .T. ) ;
#8937 = EDGE_CURVE ( 'NONE', #78082, #33468, #63186, .T. ) ;
#8938 = DIRECTION ( 'NONE',  ( 0.000000000000000000, 0.000000000000000000, 1.000000000000000000 ) ) ;
#8939 = DIRECTION ( 'NONE',  ( -4.274815082592931898E-19, -0.9999939076577903929, -0.003490651415223739937 ) ) ;
#8940 = DIRECTION ( 'NONE',  ( 0.000000000000000000, 0.000000000000000000, 1.000000000000000000 ) ) ;
#8941 = CARTESIAN_POINT ( 'NONE',  ( -9.400000000000007461, 12.50000000000000000, 4.048810130592458201 ) ) ;
#8942 = FACE_OUTER_BOUND ( 'NONE', #8280, .T. ) ;
#8943 = ORIENTED_EDGE ( 'NONE', *, *, #49298, .F. ) ;
#8944 = EDGE_CURVE ( 'NONE', #52806, #113778, #67349, .T. ) ;
#8945 = CARTESIAN_POINT ( 'NONE',  ( -14.99999999999998401, 12.50000000000000000, 0.6277270498435143509 ) ) ;
#8946 = EDGE_CURVE ( 'NONE', #112348, #7603, #48609, .T. ) ;
#8947 = CARTESIAN_POINT ( 'NONE',  ( 1.249999999999954259, 12.50000000000000000, -7.188010851410854052 ) ) ;
#8949 = VERTEX_POINT ( 'NONE', #58503 ) ;
#8948 = CARTESIAN_POINT ( 'NONE',  ( 4.599999999999940137, 2.500000000000000000, -5.022947341949754119 ) ) ;
#8950 = VECTOR ( 'NONE', #16961, 1000.000000000000000 ) ;
#8951 = EDGE_CURVE ( 'NONE', #94541, #96192, #78131, .T. ) ;
#8952 = ORIENTED_EDGE ( 'NONE', *, *, #89643, .T. ) ;
#8953 = CARTESIAN_POINT ( 'NONE',  ( -9.800000000000006040, 12.50000000000000000, -4.741630453620011565 ) ) ;
#8954 = AXIS2_PLACEMENT_3D ( 'NONE', #36524, #76432, #77074 ) ;
#8955 = EDGE_LOOP ( 'NONE', ( #49758, #116316, #27736, #11281 ) ) ;
#8956 = ORIENTED_EDGE ( 'NONE', *, *, #19548, .T. ) ;
#8957 = VECTOR ( 'NONE', #106723, 1000.000000000000000 ) ;
#8958 = ORIENTED_EDGE ( 'NONE', *, *, #81101, .T. ) ;
#8959 = DIRECTION ( 'NONE',  ( 0.000000000000000000, 1.000000000000000000, 0.000000000000000000 ) ) ;
#8960 = CIRCLE ( 'NONE', #111468, 0.09999999999999999167 ) ;
#8961 = CIRCLE ( 'NONE', #31982, 0.09999999999999982514 ) ;
#8962 = CARTESIAN_POINT ( 'NONE',  ( 4.349999999999938360, 12.50000000000000000, 1.818653347947321475 ) ) ;
#8963 = PLANE ( 'NONE',  #27431 ) ;
#8964 = CARTESIAN_POINT ( 'NONE',  ( 7.499999999999960032, 2.500000000000000000, -0.1000000000000022815 ) ) ;
#8966 = EDGE_LOOP ( 'NONE', ( #120547, #38560, #49456, #51909 ) ) ;
#8965 = CIRCLE ( 'NONE', #128115, 0.1000000000000000472 ) ;
#8967 = AXIS2_PLACEMENT_3D ( 'NONE', #36348, #76257, #26510 ) ;
#8968 = CARTESIAN_POINT ( 'NONE',  ( 8.299999999999922551, 12.50000000000000000, -2.385244779468109755E-15 ) ) ;
#8970 = EDGE_LOOP ( 'NONE', ( #122796, #76600 ) ) ;
#8969 = AXIS2_PLACEMENT_3D ( 'NONE', #116912, #44979, #6300 ) ;
#8971 = FACE_OUTER_BOUND ( 'NONE', #112421, .T. ) ;
#8972 = CARTESIAN_POINT ( 'NONE',  ( 20.64614705759127133, -2.669560853935763589, -2.247897417623094363 ) ) ;
#8973 = CIRCLE ( 'NONE', #6809, 0.1000000000000002554 ) ;
#8974 = CARTESIAN_POINT ( 'NONE',  ( 17.29982614914977646, 2.489966891809544780, 2.989943721785365938 ) ) ;
#8975 = DIRECTION ( 'NONE',  ( 0.000000000000000000, 0.000000000000000000, -1.000000000000000000 ) ) ;
#8976 = LINE ( 'NONE', #58102, #93547 ) ;
#8977 = CIRCLE ( 'NONE', #86342, 0.09999999999999982514 ) ;
#8978 = VERTEX_POINT ( 'NONE', #98386 ) ;
#8979 = ORIENTED_EDGE ( 'NONE', *, *, #19266, .F. ) ;
#8980 = ORIENTED_EDGE ( 'NONE', *, *, #111325, .F. ) ;
#8981 = ORIENTED_EDGE ( 'NONE', *, *, #33585, .T. ) ;
#8982 = ORIENTED_EDGE ( 'NONE', *, *, #42656, .F. ) ;
#8983 = DIRECTION ( 'NONE',  ( 0.000000000000000000, 0.000000000000000000, -1.000000000000000000 ) ) ;
#8984 = CARTESIAN_POINT ( 'NONE',  ( -11.84999999999999787, 12.50000000000000000, -6.213873640053560798 ) ) ;
#8985 = PLANE ( 'NONE',  #12676 ) ;
#8986 = FACE_BOUND ( 'NONE', #40798, .T. ) ;
#8987 = DIRECTION ( 'NONE',  ( 0.000000000000000000, 0.000000000000000000, -1.000000000000000000 ) ) ;
#8988 = DIRECTION ( 'NONE',  ( 0.000000000000000000, 0.000000000000000000, 1.000000000000000000 ) ) ;
#8989 = DIRECTION ( 'NONE',  ( 0.000000000000000000, 0.000000000000000000, 1.000000000000000000 ) ) ;
#8990 = CARTESIAN_POINT ( 'NONE',  ( 11.64999999999990621, 12.50000000000000000, 6.430097255199259010 ) ) ;
#8991 = CIRCLE ( 'NONE', #29944, 0.06509327318403745899 ) ;
#8992 = EDGE_CURVE ( 'NONE', #61342, #125293, #98672, .T. ) ;
#8993 = DIRECTION ( 'NONE',  ( 0.000000000000000000, 0.000000000000000000, -1.000000000000000000 ) ) ;
#8994 = DIRECTION ( 'NONE',  ( 0.000000000000000000, -0.000000000000000000, 1.000000000000000000 ) ) ;
#8995 = CARTESIAN_POINT ( 'NONE',  ( 12.89999999999989910, 12.50000000000000000, -0.6928203230275542523 ) ) ;
#8996 = AXIS2_PLACEMENT_3D ( 'NONE', #60187, #102660, #20247 ) ;
#8997 = CIRCLE ( 'NONE', #88418, 0.06509327318403741736 ) ;
#8998 = CIRCLE ( 'NONE', #126075, 0.1000000000000000472 ) ;
#8999 = DIRECTION ( 'NONE',  ( -0.000000000000000000, -1.000000000000000000, -0.000000000000000000 ) ) ;
#9000 = VERTEX_POINT ( 'NONE', #86646 ) ;
#9001 = VERTEX_POINT ( 'NONE', #116741 ) ;
#9002 = ORIENTED_EDGE ( 'NONE', *, *, #126380, .T. ) ;
#9003 = ORIENTED_EDGE ( 'NONE', *, *, #76254, .T. ) ;
#9004 = CARTESIAN_POINT ( 'NONE',  ( -13.74999999999998757, 2.500000000000000000, 1.472243186433549456 ) ) ;
#9005 = LINE ( 'NONE', #48960, #115637 ) ;
#9006 = FACE_BOUND ( 'NONE', #96670, .T. ) ;
#9007 = CIRCLE ( 'NONE', #119731, 0.1000000000000002554 ) ;
#9008 = AXIS2_PLACEMENT_3D ( 'NONE', #113080, #41796, #122918 ) ;
#9009 = DIRECTION ( 'NONE',  ( -0.000000000000000000, 1.000000000000000000, -0.000000000000000000 ) ) ;
#9010 = CIRCLE ( 'NONE', #55089, 0.06509327318403745899 ) ;
#9011 = CIRCLE ( 'NONE', #40344, 0.06509327318403745899 ) ;
#9012 = ORIENTED_EDGE ( 'NONE', *, *, #56336, .F. ) ;
#9013 = CARTESIAN_POINT ( 'NONE',  ( 1.249999999999988454, 12.50000000000000000, 2.165063509461097713 ) ) ;
#9014 = DIRECTION ( 'NONE',  ( 0.000000000000000000, 0.000000000000000000, -1.000000000000000000 ) ) ;
#9015 = DIRECTION ( 'NONE',  ( -0.000000000000000000, -1.000000000000000000, -0.000000000000000000 ) ) ;
#9016 = EDGE_CURVE ( 'NONE', #93873, #113633, #42265, .T. ) ;
#9017 = CARTESIAN_POINT ( 'NONE',  ( -6.650000000000014566, 12.50000000000000000, 2.165063509461097713 ) ) ;
#9018 = ORIENTED_EDGE ( 'NONE', *, *, #67845, .F. ) ;
#9019 = AXIS2_PLACEMENT_3D ( 'NONE', #7048, #65329, #66623 ) ;
#9020 = PLANE ( 'NONE',  #118145 ) ;
#9021 = CIRCLE ( 'NONE', #124051, 0.1000000000000000472 ) ;
#9022 = CONICAL_SURFACE ( 'NONE', #59234, 0.09999999999999982514, 0.003490658503988666988 ) ;
#9023 = EDGE_LOOP ( 'NONE', ( #76449, #20500, #89779, #31353 ) ) ;
#9024 = ORIENTED_EDGE ( 'NONE', *, *, #104554, .F. ) ;
#9025 = DIRECTION ( 'NONE',  ( 0.000000000000000000, -0.000000000000000000, 1.000000000000000000 ) ) ;
#9026 = DIRECTION ( 'NONE',  ( -0.000000000000000000, 1.000000000000000000, -0.000000000000000000 ) ) ;
#9027 = VERTEX_POINT ( 'NONE', #77471 ) ;
#9028 = ADVANCED_FACE ( 'NONE', ( #28386 ), #75687, .T. ) ;
#9029 = PLANE ( 'NONE',  #111657 ) ;
#9030 = CIRCLE ( 'NONE', #92372, 0.1000000000000002554 ) ;
#9031 = DIRECTION ( 'NONE',  ( -0.000000000000000000, 1.000000000000000000, -0.000000000000000000 ) ) ;
#9032 = ORIENTED_EDGE ( 'NONE', *, *, #172, .T. ) ;
#9033 = DIRECTION ( 'NONE',  ( 0.000000000000000000, -0.000000000000000000, 1.000000000000000000 ) ) ;
#9034 = ORIENTED_EDGE ( 'NONE', *, *, #70418, .T. ) ;
#9035 = ADVANCED_FACE ( 'NONE', ( #16604 ), #57847, .T. ) ;
#9036 = DIRECTION ( 'NONE',  ( 0.000000000000000000, 1.000000000000000000, 0.000000000000000000 ) ) ;
#9037 = EDGE_CURVE ( 'NONE', #6696, #95907, #2519, .T. ) ;
#9038 = EDGE_LOOP ( 'NONE', ( #25672, #10330 ) ) ;
#9039 = FACE_OUTER_BOUND ( 'NONE', #112352, .T. ) ;
#9040 = FACE_BOUND ( 'NONE', #24731, .T. ) ;
#9041 = ORIENTED_EDGE ( 'NONE', *, *, #121066, .F. ) ;
#9042 = CARTESIAN_POINT ( 'NONE',  ( 111.7496660746278820, 6.950752061642088364, -3.322700296524552233 ) ) ;
#9043 = EDGE_LOOP ( 'NONE', ( #55633, #66768, #43056, #8867 ) ) ;
#9044 = CARTESIAN_POINT ( 'NONE',  ( 87.50000000000001421, 0.000000000000000000, -8.199999999999999289 ) ) ;
#9045 = CARTESIAN_POINT ( 'NONE',  ( -5.650000000000019895, 12.50000000000000000, 1.883746621131358934 ) ) ;
#9046 = ADVANCED_FACE ( 'NONE', ( #127859 ), #97755, .T. ) ;
#9047 = EDGE_CURVE ( 'NONE', #46827, #70903, #69434, .T. ) ;
#9048 = AXIS2_PLACEMENT_3D ( 'NONE', #105997, #77181, #45798 ) ;
#9049 = CARTESIAN_POINT ( 'NONE',  ( -7.500000000000001776, -1.500000000000000000, 1.734723475976807094E-15 ) ) ;
#9050 = CIRCLE ( 'NONE', #98948, 0.09999999999999982514 ) ;
#9051 = EDGE_CURVE ( 'NONE', #94980, #103724, #23468, .T. ) ;
#9052 = DIRECTION ( 'NONE',  ( -1.000000000000000000, 0.000000000000000000, 1.445602896647339656E-16 ) ) ;
#9053 = EDGE_CURVE ( 'NONE', #113165, #98051, #33940, .T. ) ;
#9054 = ADVANCED_FACE ( 'NONE', ( #59137 ), #26452, .T. ) ;
#9055 = FACE_OUTER_BOUND ( 'NONE', #51411, .T. ) ;
#9056 = EDGE_LOOP ( 'NONE', ( #27589, #112836 ) ) ;
#9057 = ORIENTED_EDGE ( 'NONE', *, *, #28914, .F. ) ;
#9058 = ORIENTED_EDGE ( 'NONE', *, *, #88592, .F. ) ;
#9059 = CARTESIAN_POINT ( 'NONE',  ( -9.150000000000009237, 2.500000000000000000, 1.472243186433545459 ) ) ;
#9060 = AXIS2_PLACEMENT_3D ( 'NONE', #123429, #44223, #73682 ) ;
#9061 = CIRCLE ( 'NONE', #126140, 0.06509327318403745899 ) ;
#9062 = FACE_OUTER_BOUND ( 'NONE', #114783, .T. ) ;
#9063 = CIRCLE ( 'NONE', #13260, 0.06509327318403745899 ) ;
#9065 = DIRECTION ( 'NONE',  ( -4.274815082592931898E-19, -0.9999939076577903929, -0.003490651415223739937 ) ) ;
#9064 = CIRCLE ( 'NONE', #73908, 0.06509327318403745899 ) ;
#9067 = ORIENTED_EDGE ( 'NONE', *, *, #36889, .T. ) ;
#9066 = ORIENTED_EDGE ( 'NONE', *, *, #15107, .F. ) ;
#9068 = VERTEX_POINT ( 'NONE', #129186 ) ;
#9069 = EDGE_CURVE ( 'NONE', #31487, #37042, #39514, .T. ) ;
#9070 = LINE ( 'NONE', #20184, #127146 ) ;
#9071 = CARTESIAN_POINT ( 'NONE',  ( -8.350000000000010303, 2.500000000000000000, 6.495190528383297135 ) ) ;
#9072 = CIRCLE ( 'NONE', #63456, 0.06509327318403741736 ) ;
#9073 = CIRCLE ( 'NONE', #4942, 0.1000000000000002554 ) ;
#9074 = AXIS2_PLACEMENT_3D ( 'NONE', #59201, #118095, #68352 ) ;
#9075 = CARTESIAN_POINT ( 'NONE',  ( -4.150000000000024336, 12.50000000000000000, -2.165063509461101710 ) ) ;
#9076 = CARTESIAN_POINT ( 'NONE',  ( 2.099999999999950351, 2.500000000000000000, -2.276824562219559311E-15 ) ) ;
#9077 = DIRECTION ( 'NONE',  ( 0.000000000000000000, 0.000000000000000000, 1.000000000000000000 ) ) ;
#9078 = DIRECTION ( 'NONE',  ( 0.000000000000000000, 0.000000000000000000, 1.000000000000000000 ) ) ;
#9079 = DIRECTION ( 'NONE',  ( -0.000000000000000000, -1.000000000000000000, -0.000000000000000000 ) ) ;
#9080 = AXIS2_PLACEMENT_3D ( 'NONE', #68817, #7304, #28253 ) ;
#9081 = LINE ( 'NONE', #56871, #22798 ) ;
#9082 = CIRCLE ( 'NONE', #82254, 0.1000000000000002554 ) ;
#9083 = ORIENTED_EDGE ( 'NONE', *, *, #127753, .T. ) ;
#9084 = ORIENTED_EDGE ( 'NONE', *, *, #80921, .T. ) ;
#9085 = DIRECTION ( 'NONE',  ( -0.000000000000000000, -1.000000000000000000, -0.000000000000000000 ) ) ;
#9086 = CARTESIAN_POINT ( 'NONE',  ( -9.400000000000009237, 12.50000000000000000, -4.676537180435974328 ) ) ;
#9087 = ORIENTED_EDGE ( 'NONE', *, *, #82659, .F. ) ;
#9088 = ORIENTED_EDGE ( 'NONE', *, *, #112002, .F. ) ;
#9089 = CARTESIAN_POINT ( 'NONE',  ( 186.1927083336747160, 6.551208109652275624, -3.782341765624998686 ) ) ;
#9090 = DIRECTION ( 'NONE',  ( 0.000000000000000000, 1.000000000000000000, 0.000000000000000000 ) ) ;
#9091 = CARTESIAN_POINT ( 'NONE',  ( 15.83209681635537258, -2.500000000000000000, 5.404881881984332281 ) ) ;
#9092 = AXIS2_PLACEMENT_3D ( 'NONE', #9314, #49259, #89164 ) ;
#9093 = CARTESIAN_POINT ( 'NONE',  ( -3.300000000000028244, 2.500000000000000000, 4.230127018922196669 ) ) ;
#9094 = CARTESIAN_POINT ( 'NONE',  ( -13.94999999999998685, 2.500000000000000000, -2.511473670974875727 ) ) ;
#9095 = DIRECTION ( 'NONE',  ( 0.000000000000000000, 1.000000000000000000, 0.000000000000000000 ) ) ;
#9096 = DIRECTION ( 'NONE',  ( 0.000000000000000000, 1.000000000000000000, 0.000000000000000000 ) ) ;
#9097 = EDGE_CURVE ( 'NONE', #127312, #24007, #119607, .T. ) ;
#9098 = CONICAL_SURFACE ( 'NONE', #88508, 0.1000000000000002554, 0.003490658503988666988 ) ;
#9099 = EDGE_CURVE ( 'NONE', #110247, #61095, #84100, .T. ) ;
#9100 = FACE_OUTER_BOUND ( 'NONE', #123829, .T. ) ;
#9101 = CIRCLE ( 'NONE', #82274, 0.06509327318403745899 ) ;
#9102 = ORIENTED_EDGE ( 'NONE', *, *, #19385, .F. ) ;
#9103 = EDGE_CURVE ( 'NONE', #49010, #20499, #21410, .T. ) ;
#9104 = ORIENTED_EDGE ( 'NONE', *, *, #68196, .T. ) ;
#9105 = VERTEX_POINT ( 'NONE', #120623 ) ;
#9106 = ADVANCED_FACE ( 'NONE', ( #2128 ), #20498, .T. ) ;
#9107 = ORIENTED_EDGE ( 'NONE', *, *, #41940, .F. ) ;
#9108 = CONICAL_SURFACE ( 'NONE', #32121, 0.1000000000000002554, 0.003490658503988666988 ) ;
#9109 = DIRECTION ( 'NONE',  ( 0.000000000000000000, 0.000000000000000000, 1.000000000000000000 ) ) ;
#9110 = DIRECTION ( 'NONE',  ( 0.000000000000000000, 0.000000000000000000, 1.000000000000000000 ) ) ;
#9111 = CONICAL_SURFACE ( 'NONE', #61457, 0.1000000000000000472, 0.003490658503988666988 ) ;
#9112 = EDGE_CURVE ( 'NONE', #51138, #104697, #42069, .T. ) ;
#9113 = CIRCLE ( 'NONE', #76010, 0.06509327318403745899 ) ;
#9114 = ORIENTED_EDGE ( 'NONE', *, *, #41042, .T. ) ;
#9115 = EDGE_CURVE ( 'NONE', #91937, #87854, #71588, .T. ) ;
#9116 = LINE ( 'NONE', #41185, #98766 ) ;
#9117 = AXIS2_PLACEMENT_3D ( 'NONE', #128773, #125035, #115859 ) ;
#9118 = CARTESIAN_POINT ( 'NONE',  ( 17.50000000000000000, -2.750000000000000444, -2.864912725862979848 ) ) ;
#9119 = EDGE_CURVE ( 'NONE', #70277, #85577, #119697, .T. ) ;
#9120 = DIRECTION ( 'NONE',  ( -0.000000000000000000, 1.000000000000000000, -0.000000000000000000 ) ) ;
#9122 = VERTEX_POINT ( 'NONE', #12588 ) ;
#9121 = DIRECTION ( 'NONE',  ( 0.000000000000000000, 0.000000000000000000, 1.000000000000000000 ) ) ;
#9123 = DIRECTION ( 'NONE',  ( -0.000000000000000000, 1.000000000000000000, -0.000000000000000000 ) ) ;
#9124 = CIRCLE ( 'NONE', #11258, 0.1000000000000002554 ) ;
#9125 = EDGE_CURVE ( 'NONE', #98405, #128034, #11309, .T. ) ;
#9126 = CARTESIAN_POINT ( 'NONE',  ( 5.399999999999935518, 12.50000000000000000, -4.395220292106239768 ) ) ;
#9127 = ORIENTED_EDGE ( 'NONE', *, *, #55767, .T. ) ;
#9128 = CONICAL_SURFACE ( 'NONE', #34186, 0.1000000000000002554, 0.003490658503988666988 ) ;
#9129 = AXIS2_PLACEMENT_3D ( 'NONE', #72224, #22490, #32317 ) ;
#9130 = CIRCLE ( 'NONE', #17524, 0.06509327318403745899 ) ;
#9131 = ORIENTED_EDGE ( 'NONE', *, *, #56503, .F. ) ;
#9132 = VERTEX_POINT ( 'NONE', #19853 ) ;
#9133 = VERTEX_POINT ( 'NONE', #112099 ) ;
#9134 = CARTESIAN_POINT ( 'NONE',  ( 6.849999999999929479, 12.50000000000000000, -2.511473670974877948 ) ) ;
#9135 = CONICAL_SURFACE ( 'NONE', #101072, 0.1000000000000002554, 0.003490658503988666988 ) ;
#9136 = CARTESIAN_POINT ( 'NONE',  ( 13.34999999999989662, 2.500000000000000000, -2.857883832488653741 ) ) ;
#9137 = AXIS2_PLACEMENT_3D ( 'NONE', #95143, #15916, #93217 ) ;
#9138 = VERTEX_POINT ( 'NONE', #52522 ) ;
#9139 = DIRECTION ( 'NONE',  ( -0.000000000000000000, -1.000000000000000000, -0.000000000000000000 ) ) ;
#9140 = CARTESIAN_POINT ( 'NONE',  ( -2.900000000000029221, 12.50000000000000000, -4.330127018922201643 ) ) ;
#9141 = DIRECTION ( 'NONE',  ( 0.000000000000000000, 0.000000000000000000, -1.000000000000000000 ) ) ;
#9142 = DIRECTION ( 'NONE',  ( 0.000000000000000000, -0.9999939076577903929, 0.003490651415223739937 ) ) ;
#9143 = EDGE_CURVE ( 'NONE', #51919, #71123, #10635, .T. ) ;
#9144 = ORIENTED_EDGE ( 'NONE', *, *, #78306, .T. ) ;
#9145 = CARTESIAN_POINT ( 'NONE',  ( 4.549999999999935874, 2.500000000000000000, 6.595190528383296780 ) ) ;
#9146 = EDGE_LOOP ( 'NONE', ( #115940, #29496 ) ) ;
#9147 = EDGE_LOOP ( 'NONE', ( #59259, #65933 ) ) ;
#9149 = CONICAL_SURFACE ( 'NONE', #53071, 0.1000000000000002554, 0.003490658503988666988 ) ;
#9148 = DIRECTION ( 'NONE',  ( -0.000000000000000000, 1.000000000000000000, -0.000000000000000000 ) ) ;
#9150 = AXIS2_PLACEMENT_3D ( 'NONE', #14330, #54277, #94199 ) ;
#9151 = CARTESIAN_POINT ( 'NONE',  ( 11.64999999999990443, 2.500000000000000000, 1.572243186433545548 ) ) ;
#9152 = FACE_BOUND ( 'NONE', #53337, .T. ) ;
#9153 = DIRECTION ( 'NONE',  ( 0.000000000000000000, 1.000000000000000000, 0.000000000000000000 ) ) ;
#9154 = DIRECTION ( 'NONE',  ( 0.000000000000000000, 0.000000000000000000, -1.000000000000000000 ) ) ;
#9155 = LINE ( 'NONE', #22224, #73195 ) ;
#9156 = CIRCLE ( 'NONE', #90728, 0.1000000000000000472 ) ;
#9157 = CIRCLE ( 'NONE', #82332, 0.06509327318403741736 ) ;
#9158 = ADVANCED_FACE ( 'NONE', ( #30979 ), #44490, .T. ) ;
#9159 = CIRCLE ( 'NONE', #28036, 0.09999999999999982514 ) ;
#9160 = AXIS2_PLACEMENT_3D ( 'NONE', #29212, #67818, #88077 ) ;
#9161 = ORIENTED_EDGE ( 'NONE', *, *, #22010, .F. ) ;
#9162 = CARTESIAN_POINT ( 'NONE',  ( 4.349999999999940137, 2.500000000000000000, -2.611473670974877592 ) ) ;
#9163 = DIRECTION ( 'NONE',  ( -0.000000000000000000, 1.000000000000000000, -0.000000000000000000 ) ) ;
#9164 = DIRECTION ( 'NONE',  ( -0.000000000000000000, -1.000000000000000000, -0.000000000000000000 ) ) ;
#9165 = DIRECTION ( 'NONE',  ( -0.000000000000000000, 1.000000000000000000, -0.000000000000000000 ) ) ;
#9166 = ORIENTED_EDGE ( 'NONE', *, *, #102502, .F. ) ;
#9167 = PLANE ( 'NONE',  #34374 ) ;
#9168 = AXIS2_PLACEMENT_3D ( 'NONE', #63654, #103579, #44014 ) ;
#9169 = VECTOR ( 'NONE', #26415, 1000.000000000000000 ) ;
#9170 = DIRECTION ( 'NONE',  ( 0.000000000000000000, 1.000000000000000000, 0.000000000000000000 ) ) ;
#9171 = ORIENTED_EDGE ( 'NONE', *, *, #89424, .T. ) ;
#9172 = ORIENTED_EDGE ( 'NONE', *, *, #69173, .F. ) ;
#9173 = AXIS2_PLACEMENT_3D ( 'NONE', #32143, #91038, #52400 ) ;
#9174 = DIRECTION ( 'NONE',  ( -0.000000000000000000, -1.000000000000000000, -0.000000000000000000 ) ) ;
#9175 = ADVANCED_FACE ( 'NONE', ( #11951 ), #80712, .T. ) ;
#9176 = DIRECTION ( 'NONE',  ( 0.000000000000000000, 1.000000000000000000, 0.000000000000000000 ) ) ;
#9177 = FACE_BOUND ( 'NONE', #25366, .T. ) ;
#9178 = DIRECTION ( 'NONE',  ( 0.000000000000000000, 0.000000000000000000, 1.000000000000000000 ) ) ;
#9179 = VERTEX_POINT ( 'NONE', #121268 ) ;
#9180 = CARTESIAN_POINT ( 'NONE',  ( -12.29999999999999538, 2.500000000000000000, 4.676537180435972552 ) ) ;
#9181 = VERTEX_POINT ( 'NONE', #70240 ) ;
#9182 = LINE ( 'NONE', #47183, #105103 ) ;
#9183 = CARTESIAN_POINT ( 'NONE',  ( 183.9218750003414016, 0.000000000000000000, 7.564683531250000925 ) ) ;
#9185 = ORIENTED_EDGE ( 'NONE', *, *, #102178, .T. ) ;
#9184 = CIRCLE ( 'NONE', #119907, 0.06509327318403745899 ) ;
#9186 = CARTESIAN_POINT ( 'NONE',  ( 5.849999999999933920, 2.500000000000000000, -2.165063509461101710 ) ) ;
#9187 = DIRECTION ( 'NONE',  ( 0.000000000000000000, 0.000000000000000000, 1.000000000000000000 ) ) ;
#9188 = DIRECTION ( 'NONE',  ( 0.000000000000000000, 0.000000000000000000, 1.000000000000000000 ) ) ;
#9189 = CARTESIAN_POINT ( 'NONE',  ( -12.89999999999999325, 12.50000000000000000, 0.6928203230275535862 ) ) ;
#9190 = VECTOR ( 'NONE', #65523, 1000.000000000000000 ) ;
#9191 = AXIS2_PLACEMENT_3D ( 'NONE', #84506, #124431, #34776 ) ;
#9192 = ORIENTED_EDGE ( 'NONE', *, *, #18573, .T. ) ;
#9193 = ADVANCED_FACE ( 'NONE', ( #31604 ), #6807, .T. ) ;
#9194 = DIRECTION ( 'NONE',  ( 0.000000000000000000, 1.000000000000000000, 0.000000000000000000 ) ) ;
#9195 = DIRECTION ( 'NONE',  ( 0.000000000000000000, -0.9999939076577903929, 0.003490651415223739937 ) ) ;
#9196 = LINE ( 'NONE', #49146, #36762 ) ;
#9197 = DIRECTION ( 'NONE',  ( 0.000000000000000000, 1.000000000000000000, 0.000000000000000000 ) ) ;
#9198 = ORIENTED_EDGE ( 'NONE', *, *, #21995, .T. ) ;
#9199 = ORIENTED_EDGE ( 'NONE', *, *, #115736, .F. ) ;
#9200 = CARTESIAN_POINT ( 'NONE',  ( 16.56576425165006938, 2.500000000000000000, 6.084390597445819893 ) ) ;
#9201 = ORIENTED_EDGE ( 'NONE', *, *, #50891, .T. ) ;
#9203 = PLANE ( 'NONE',  #84832 ) ;
#9202 = AXIS2_PLACEMENT_3D ( 'NONE', #114817, #104992, #94538 ) ;
#9204 = DIRECTION ( 'NONE',  ( -0.000000000000000000, 1.000000000000000000, -0.000000000000000000 ) ) ;
#9205 = CONICAL_SURFACE ( 'NONE', #40538, 0.09999999999999982514, 0.003490658503988666988 ) ;
#9206 = DIRECTION ( 'NONE',  ( -0.000000000000000000, -1.000000000000000000, -0.000000000000000000 ) ) ;
#9207 = DIRECTION ( 'NONE',  ( 0.000000000000000000, 0.000000000000000000, 1.000000000000000000 ) ) ;
#9208 = ORIENTED_EDGE ( 'NONE', *, *, #114771, .F. ) ;
#9209 = CARTESIAN_POINT ( 'NONE',  ( 7.899999999999924860, 2.500000000000000000, 4.430127018922196847 ) ) ;
#9210 = FACE_OUTER_BOUND ( 'NONE', #663, .T. ) ;
#9211 = CARTESIAN_POINT ( 'NONE',  ( 81.97620162060584903, 3.937821635701168166, -6.124242818032728408 ) ) ;
#9212 = EDGE_CURVE ( 'NONE', #92207, #61030, #184, .T. ) ;
#9213 = EDGE_CURVE ( 'NONE', #40443, #106006, #79993, .T. ) ;
#9214 = CARTESIAN_POINT ( 'NONE',  ( 13.34999999999989662, 2.500000000000000000, -2.165063509461101710 ) ) ;
#9215 = PLANE ( 'NONE',  #105069 ) ;
#9216 = EDGE_CURVE ( 'NONE', #126539, #108133, #125959, .T. ) ;
#9217 = EDGE_CURVE ( 'NONE', #65457, #113749, #80056, .T. ) ;
#9218 = CARTESIAN_POINT ( 'NONE',  ( -14.54999999999998472, 2.500000000000000000, 2.065063509461101621 ) ) ;
#9219 = ORIENTED_EDGE ( 'NONE', *, *, #120553, .T. ) ;
#9220 = ORIENTED_EDGE ( 'NONE', *, *, #28587, .F. ) ;
#9221 = DIRECTION ( 'NONE',  ( 0.000000000000000000, 1.000000000000000000, 0.000000000000000000 ) ) ;
#9223 = EDGE_LOOP ( 'NONE', ( #78376, #128382 ) ) ;
#9222 = CIRCLE ( 'NONE', #126203, 0.06509327318403745899 ) ;
#9224 = CONICAL_SURFACE ( 'NONE', #36430, 0.1000000000000002554, 0.003490658503988666988 ) ;
#9225 = VECTOR ( 'NONE', #42677, 1000.000000000000000 ) ;
#9226 = CARTESIAN_POINT ( 'NONE',  ( 107.9999999999992895, 5.855766388783293586, 5.000000000000080824 ) ) ;
#9228 = ORIENTED_EDGE ( 'NONE', *, *, #62204, .T. ) ;
#9227 = ORIENTED_EDGE ( 'NONE', *, *, #129400, .T. ) ;
#9229 = EDGE_LOOP ( 'NONE', ( #110914, #111984, #58646, #110071 ) ) ;
#9230 = AXIS2_PLACEMENT_3D ( 'NONE', #94501, #44125, #6739 ) ;
#9231 = EDGE_CURVE ( 'NONE', #83779, #129184, #84189, .T. ) ;
#9232 = LINE ( 'NONE', #48510, #112762 ) ;
#9233 = AXIS2_PLACEMENT_3D ( 'NONE', #120885, #42335, #121514 ) ;
#9234 = ADVANCED_FACE ( 'NONE', ( #50584 ), #62363, .T. ) ;
#9235 = CARTESIAN_POINT ( 'NONE',  ( 11.64999999999990266, 2.500000000000000000, -6.495190528383302464 ) ) ;
#9236 = EDGE_CURVE ( 'NONE', #75526, #26170, #96704, .T. ) ;
#9237 = PLANE ( 'NONE',  #24690 ) ;
#9238 = SURFACE_SIDE_STYLE ('',( #47882 ) ) ;
#9239 = DIRECTION ( 'NONE',  ( -0.000000000000000000, -1.000000000000000000, -0.000000000000000000 ) ) ;
#9240 = DIRECTION ( 'NONE',  ( -0.000000000000000000, 1.000000000000000000, -0.000000000000000000 ) ) ;
#9241 = DIRECTION ( 'NONE',  ( 0.000000000000000000, 1.000000000000000000, 0.000000000000000000 ) ) ;
#9242 = CARTESIAN_POINT ( 'NONE',  ( 5.649999999999934630, 12.50000000000000000, 6.841600689897072485 ) ) ;
#9243 = CARTESIAN_POINT ( 'NONE',  ( 0.8499999999999536815, 2.500000000000000000, 5.802370205355744659 ) ) ;
#9244 = ORIENTED_EDGE ( 'NONE', *, *, #34204, .T. ) ;
#9245 = ORIENTED_EDGE ( 'NONE', *, *, #90779, .F. ) ;
#9246 = CONICAL_SURFACE ( 'NONE', #15486, 0.09999999999999982514, 0.003490658503988666988 ) ;
#9247 = DIRECTION ( 'NONE',  ( -0.000000000000000000, -1.000000000000000000, -0.000000000000000000 ) ) ;
#9248 = CONICAL_SURFACE ( 'NONE', #97067, 0.09999999999999982514, 0.003490658503988666988 ) ;
#9249 = CIRCLE ( 'NONE', #86594, 0.06509327318403743123 ) ;
#9250 = ORIENTED_EDGE ( 'NONE', *, *, #648, .T. ) ;
#9251 = EDGE_LOOP ( 'NONE', ( #45064, #72272, #77640, #4723 ) ) ;
#9252 = FACE_OUTER_BOUND ( 'NONE', #89003, .T. ) ;
#9253 = AXIS2_PLACEMENT_3D ( 'NONE', #18482, #7364, #57778 ) ;
#9254 = CIRCLE ( 'NONE', #25986, 0.1000000000000002554 ) ;
#9255 = DIRECTION ( 'NONE',  ( -0.000000000000000000, 1.000000000000000000, -0.000000000000000000 ) ) ;
#9257 = FACE_OUTER_BOUND ( 'NONE', #52603, .T. ) ;
#9256 = VECTOR ( 'NONE', #25708, 1000.000000000000000 ) ;
#9258 = DIRECTION ( 'NONE',  ( -0.000000000000000000, 1.000000000000000000, -0.000000000000000000 ) ) ;
#9259 = LINE ( 'NONE', #12467, #124001 ) ;
#9260 = ORIENTED_EDGE ( 'NONE', *, *, #87253, .F. ) ;
#9261 = CIRCLE ( 'NONE', #19419, 0.06509327318403745899 ) ;
#9263 = ORIENTED_EDGE ( 'NONE', *, *, #74711, .T. ) ;
#9262 = AXIS2_PLACEMENT_3D ( 'NONE', #47102, #49687, #108584 ) ;
#9264 = CARTESIAN_POINT ( 'NONE',  ( 10.39999999999991154, 2.500000000000000000, -3.637306695894650055 ) ) ;
#9265 = CONICAL_SURFACE ( 'NONE', #76163, 0.09999999999999999167, 0.003490658503988666988 ) ;
#9266 = ORIENTED_EDGE ( 'NONE', *, *, #42339, .T. ) ;
#9267 = CARTESIAN_POINT ( 'NONE',  ( -9.800000000000004263, 2.500000000000000000, -0.4464101615137783252 ) ) ;
#9268 = ORIENTED_EDGE ( 'NONE', *, *, #112266, .T. ) ;
#9269 = CIRCLE ( 'NONE', #92908, 0.06509327318403745899 ) ;
#9270 = ORIENTED_EDGE ( 'NONE', *, *, #47643, .T. ) ;
#9271 = LINE ( 'NONE', #97646, #94227 ) ;
#9272 = FACE_OUTER_BOUND ( 'NONE', #71385, .T. ) ;
#9273 = EDGE_CURVE ( 'NONE', #113704, #117157, #121847, .T. ) ;
#9274 = DIRECTION ( 'NONE',  ( 0.000000000000000000, 0.000000000000000000, 1.000000000000000000 ) ) ;
#9275 = DIRECTION ( 'NONE',  ( 0.000000000000000000, 0.000000000000000000, -1.000000000000000000 ) ) ;
#9276 = EDGE_CURVE ( 'NONE', #3365, #21424, #35943, .T. ) ;
#9277 = DIRECTION ( 'NONE',  ( -0.000000000000000000, 1.000000000000000000, -0.000000000000000000 ) ) ;
#9278 = ORIENTED_EDGE ( 'NONE', *, *, #116510, .F. ) ;
#9279 = FACE_OUTER_BOUND ( 'NONE', #19632, .T. ) ;
#9280 = CARTESIAN_POINT ( 'NONE',  ( -11.89999999999999680, 2.500000000000000000, -4.576537180435975571 ) ) ;
#9281 = CARTESIAN_POINT ( 'NONE',  ( -12.09999999999999609, 12.50000000000000000, -3.572213422710609709 ) ) ;
#9282 = DIRECTION ( 'NONE',  ( 0.000000000000000000, 0.000000000000000000, 1.000000000000000000 ) ) ;
#9283 = VECTOR ( 'NONE', #95610, 1000.000000000000000 ) ;
#9284 = EDGE_CURVE ( 'NONE', #77431, #129270, #19346, .T. ) ;
#9285 = CARTESIAN_POINT ( 'NONE',  ( 13.74999999999989342, 2.500000000000000000, -1.572243186433550211 ) ) ;
#9286 = ORIENTED_EDGE ( 'NONE', *, *, #110864, .F. ) ;
#9287 = ORIENTED_EDGE ( 'NONE', *, *, #30866, .F. ) ;
#9288 = DIRECTION ( 'NONE',  ( -0.000000000000000000, 1.000000000000000000, -0.000000000000000000 ) ) ;
#9289 = ORIENTED_EDGE ( 'NONE', *, *, #62439, .F. ) ;
#9290 = AXIS2_PLACEMENT_3D ( 'NONE', #14164, #81627, #32563 ) ;
#9291 = CARTESIAN_POINT ( 'NONE',  ( 10.44999999999991402, 2.500000000000000000, 6.395190528383296602 ) ) ;
#9292 = LINE ( 'NONE', #89138, #81632 ) ;
#9293 = VECTOR ( 'NONE', #23489, 1000.000000000000000 ) ;
#9294 = EDGE_LOOP ( 'NONE', ( #61885, #121794, #22820, #124223 ) ) ;
#9295 = DIRECTION ( 'NONE',  ( 0.000000000000000000, 0.000000000000000000, -1.000000000000000000 ) ) ;
#9296 = CARTESIAN_POINT ( 'NONE',  ( -13.74999999999998757, 12.50000000000000000, -2.922977105672689202 ) ) ;
#9297 = LINE ( 'NONE', #70159, #79625 ) ;
#9298 = CARTESIAN_POINT ( 'NONE',  ( 7.499999999999961808, 2.500000000000000000, -4.230127018922201998 ) ) ;
#9299 = ORIENTED_EDGE ( 'NONE', *, *, #54776, .F. ) ;
#9300 = CONICAL_SURFACE ( 'NONE', #40630, 0.1000000000000002554, 0.003490658503988666988 ) ;
#9301 = CARTESIAN_POINT ( 'NONE',  ( 6.249999999999967137, 12.50000000000000000, 6.430097255199259010 ) ) ;
#9302 = ORIENTED_EDGE ( 'NONE', *, *, #14775, .T. ) ;
#9303 = DIRECTION ( 'NONE',  ( 0.000000000000000000, -0.000000000000000000, 1.000000000000000000 ) ) ;
#9304 = DIRECTION ( 'NONE',  ( -0.000000000000000000, -1.000000000000000000, -0.000000000000000000 ) ) ;
#9305 = CARTESIAN_POINT ( 'NONE',  ( -0.8500000000000382805, 12.50000000000000000, -7.253104124594891289 ) ) ;
#9306 = ORIENTED_EDGE ( 'NONE', *, *, #97306, .T. ) ;
#9307 = AXIS2_PLACEMENT_3D ( 'NONE', #52457, #779, #70812 ) ;
#9308 = VECTOR ( 'NONE', #32852, 1000.000000000000000 ) ;
#9309 = DIRECTION ( 'NONE',  ( -4.274815082592931898E-19, -0.9999939076577903929, -0.003490651415223739937 ) ) ;
#9310 = EDGE_CURVE ( 'NONE', #128257, #26935, #40304, .T. ) ;
#9312 = ORIENTED_EDGE ( 'NONE', *, *, #54705, .F. ) ;
#9311 = AXIS2_PLACEMENT_3D ( 'NONE', #100320, #41414, #61696 ) ;
#9313 = CARTESIAN_POINT ( 'NONE',  ( -5.850000000000022737, 2.500000000000000000, -2.265063509461101798 ) ) ;
#9314 = CARTESIAN_POINT ( 'NONE',  ( -5.800000000000018474, 2.500000000000000000, 4.330127018922196314 ) ) ;
#9315 = CARTESIAN_POINT ( 'NONE',  ( -2.050000000000033129, 12.50000000000000000, 2.165063509461097713 ) ) ;
#9316 = EDGE_LOOP ( 'NONE', ( #44407, #107328, #14188, #28135 ) ) ;
#9317 = CARTESIAN_POINT ( 'NONE',  ( 10.79999999999991012, 2.500000000000000000, -4.230127018922201998 ) ) ;
#9318 = CARTESIAN_POINT ( 'NONE',  ( -12.49999999999999467, 2.500000000000000000, -3.737306695894647035 ) ) ;
#9319 = ADVANCED_FACE ( 'NONE', ( #106608 ), #113444, .T. ) ;
#9320 = ORIENTED_EDGE ( 'NONE', *, *, #121331, .F. ) ;
#9321 = CARTESIAN_POINT ( 'NONE',  ( -11.25000000000000178, 2.500000000000000000, -5.802370205355746435 ) ) ;
#9322 = ADVANCED_FACE ( 'NONE', ( #16279 ), #66042, .T. ) ;
#9323 = ORIENTED_EDGE ( 'NONE', *, *, #60627, .F. ) ;
#9324 = CARTESIAN_POINT ( 'NONE',  ( -13.14999999999999147, 12.50000000000000000, 1.818653347947325472 ) ) ;
#9325 = CIRCLE ( 'NONE', #67907, 0.1000000000000002554 ) ;
#9326 = ORIENTED_EDGE ( 'NONE', *, *, #50753, .T. ) ;
#9327 = DIRECTION ( 'NONE',  ( 0.000000000000000000, 1.000000000000000000, 0.000000000000000000 ) ) ;
#9328 = CARTESIAN_POINT ( 'NONE',  ( -5.000000000000026645, 12.50000000000000000, -3.637306695894650055 ) ) ;
#9329 = VECTOR ( 'NONE', #78992, 1000.000000000000000 ) ;
#9330 = CONICAL_SURFACE ( 'NONE', #3085, 0.1000000000000000056, 0.003490658503988666988 ) ;
#9331 = ORIENTED_EDGE ( 'NONE', *, *, #20867, .T. ) ;
#9332 = ADVANCED_FACE ( 'NONE', ( #47064 ), #25599, .T. ) ;
#9333 = ORIENTED_EDGE ( 'NONE', *, *, #124504, .F. ) ;
#9334 = LINE ( 'NONE', #6722, #117774 ) ;
#9335 = DIRECTION ( 'NONE',  ( 0.000000000000000000, 0.000000000000000000, 1.000000000000000000 ) ) ;
#9336 = ORIENTED_EDGE ( 'NONE', *, *, #112503, .T. ) ;
#9337 = PLANE ( 'NONE',  #92809 ) ;
#9338 = CARTESIAN_POINT ( 'NONE',  ( 186.6510416670080872, 4.367472073101518859, -7.564683531249999149 ) ) ;
#9339 = AXIS2_PLACEMENT_3D ( 'NONE', #122908, #82992, #24061 ) ;
#9340 = CIRCLE ( 'NONE', #26077, 0.06509327318403741736 ) ;
#9341 = VECTOR ( 'NONE', #44721, 1000.000000000000000 ) ;
#9342 = CARTESIAN_POINT ( 'NONE',  ( -1.650000000000035216, 2.500000000000000000, -5.902370205355750521 ) ) ;
#9343 = CARTESIAN_POINT ( 'NONE',  ( 103.5197895262259493, 8.411351917275529999, -2.243970670365522224 ) ) ;
#9344 = LINE ( 'NONE', #97081, #53027 ) ;
#9345 = AXIS2_PLACEMENT_3D ( 'NONE', #69310, #109239, #100085 ) ;
#9346 = DIRECTION ( 'NONE',  ( 1.000000000000000000, 0.000000000000000000, 0.000000000000000000 ) ) ;
#9347 = CARTESIAN_POINT ( 'NONE',  ( 10.64999999999991331, 2.500000000000000000, 6.841600689897072485 ) ) ;
#9348 = CIRCLE ( 'NONE', #1034, 0.1000000000000002554 ) ;
#9349 = CIRCLE ( 'NONE', #7186, 0.06509327318403745899 ) ;
#9350 = ORIENTED_EDGE ( 'NONE', *, *, #19285, .T. ) ;
#9352 = ORIENTED_EDGE ( 'NONE', *, *, #83133, .F. ) ;
#9351 = EDGE_CURVE ( 'NONE', #9179, #91328, #63647, .T. ) ;
#9353 = VERTEX_POINT ( 'NONE', #97434 ) ;
#9354 = EDGE_LOOP ( 'NONE', ( #46928, #53020 ) ) ;
#9355 = DIRECTION ( 'NONE',  ( 0.000000000000000000, 0.000000000000000000, -1.000000000000000000 ) ) ;
#9356 = DIRECTION ( 'NONE',  ( 0.000000000000000000, 0.000000000000000000, 1.000000000000000000 ) ) ;
#9357 = VECTOR ( 'NONE', #115014, 1000.000000000000000 ) ;
#9358 = FACE_OUTER_BOUND ( 'NONE', #106855, .T. ) ;
#9359 = ORIENTED_EDGE ( 'NONE', *, *, #102783, .F. ) ;
#9360 = FACE_BOUND ( 'NONE', #125009, .T. ) ;
#9361 = ORIENTED_EDGE ( 'NONE', *, *, #47864, .F. ) ;
#9362 = DIRECTION ( 'NONE',  ( 0.000000000000000000, 1.000000000000000000, 0.000000000000000000 ) ) ;
#9363 = CARTESIAN_POINT ( 'NONE',  ( -12.29999999999999538, 12.50000000000000000, -0.3464101615137741841 ) ) ;
#9365 = ADVANCED_FACE ( 'NONE', ( #102903 ), #100909, .T. ) ;
#9364 = CARTESIAN_POINT ( 'NONE',  ( -11.64999999999999680, 2.500000000000000000, -2.265063509461097802 ) ) ;
#9366 = DIRECTION ( 'NONE',  ( 0.000000000000000000, -0.9999939076577903929, 0.003490651415223739937 ) ) ;
#9367 = DIRECTION ( 'NONE',  ( -0.000000000000000000, 1.000000000000000000, -0.000000000000000000 ) ) ;
#9368 = CARTESIAN_POINT ( 'NONE',  ( -7.700000000000010836, 2.500000000000000000, 4.083716857408421497 ) ) ;
#9369 = FACE_OUTER_BOUND ( 'NONE', #29517, .T. ) ;
#9370 = CARTESIAN_POINT ( 'NONE',  ( 13.74999999999989519, 12.50000000000000000, -2.857883832488653741 ) ) ;
#9371 = EDGE_CURVE ( 'NONE', #103567, #60985, #33548, .T. ) ;
#9372 = ADVANCED_FACE ( 'NONE', ( #17577 ), #564, .T. ) ;
#9373 = LINE ( 'NONE', #89219, #47405 ) ;
#9374 = EDGE_CURVE ( 'NONE', #10577, #125752, #50761, .T. ) ;
#9375 = EDGE_CURVE ( 'NONE', #63575, #41663, #32910, .T. ) ;
#9376 = AXIS2_PLACEMENT_3D ( 'NONE', #85876, #125181, #125799 ) ;
#9377 = CARTESIAN_POINT ( 'NONE',  ( -0.8500000000000390576, 12.50000000000000000, -2.165063509461101710 ) ) ;
#9378 = ORIENTED_EDGE ( 'NONE', *, *, #76459, .T. ) ;
#9379 = EDGE_LOOP ( 'NONE', ( #89695, #43189, #92876, #122815 ) ) ;
#9380 = ORIENTED_EDGE ( 'NONE', *, *, #111507, .F. ) ;
#9381 = ORIENTED_EDGE ( 'NONE', *, *, #74890, .T. ) ;
#9382 = CARTESIAN_POINT ( 'NONE',  ( 17.45053073489777873, -1.969617801096962495, -4.507369966543559592 ) ) ;
#9383 = EDGE_CURVE ( 'NONE', #30984, #91594, #65414, .T. ) ;
#9384 = DIRECTION ( 'NONE',  ( 0.000000000000000000, 0.000000000000000000, -1.000000000000000000 ) ) ;
#9387 = ORIENTED_EDGE ( 'NONE', *, *, #57398, .F. ) ;
#9386 = EDGE_LOOP ( 'NONE', ( #18804, #64629 ) ) ;
#9385 = EDGE_CURVE ( 'NONE', #100404, #15576, #69521, .T. ) ;
#9388 = EDGE_LOOP ( 'NONE', ( #75653, #25072, #100050, #31211 ) ) ;
#9389 = CARTESIAN_POINT ( 'NONE',  ( 185.0000000000000000, 0.000000000000000000, 7.700000000000000178 ) ) ;
#9390 = AXIS2_PLACEMENT_3D ( 'NONE', #122699, #33053, #63130 ) ;
#9391 = CONICAL_SURFACE ( 'NONE', #76281, 0.1000000000000002554, 0.003490658503988666988 ) ;
#9392 = EDGE_CURVE ( 'NONE', #2451, #10395, #65310, .T. ) ;
#9393 = ADVANCED_FACE ( 'NONE', ( #72820 ), #123901, .T. ) ;
#9394 = CARTESIAN_POINT ( 'NONE',  ( -9.150000000000009237, 2.500000000000000000, -1.372243186433550033 ) ) ;
#9395 = DIRECTION ( 'NONE',  ( 0.000000000000000000, 0.000000000000000000, -1.000000000000000000 ) ) ;
#9396 = DIRECTION ( 'NONE',  ( -0.000000000000000000, 1.000000000000000000, -0.000000000000000000 ) ) ;
#9397 = DIRECTION ( 'NONE',  ( 0.000000000000000000, 0.000000000000000000, -1.000000000000000000 ) ) ;
#9398 = CARTESIAN_POINT ( 'NONE',  ( 14.99999999999992895, 2.500000000000000000, 0.09999999999999772959 ) ) ;
#9399 = CARTESIAN_POINT ( 'NONE',  ( -3.550000000000027356, 2.500000000000000000, -2.411473670974877859 ) ) ;
#9400 = EDGE_LOOP ( 'NONE', ( #28922, #83238, #119882, #65804 ) ) ;
#9401 = EDGE_CURVE ( 'NONE', #107047, #46462, #3423, .T. ) ;
#9402 = CARTESIAN_POINT ( 'NONE',  ( 11.69999999999990870, 2.500000000000000000, 4.430127018922196847 ) ) ;
#9403 = ORIENTED_EDGE ( 'NONE', *, *, #16123, .F. ) ;
#9404 = CONICAL_SURFACE ( 'NONE', #53321, 0.1000000000000002554, 0.003490658503988666988 ) ;
#9405 = ORIENTED_EDGE ( 'NONE', *, *, #79554, .T. ) ;
#9406 = VERTEX_POINT ( 'NONE', #20170 ) ;
#9407 = AXIS2_PLACEMENT_3D ( 'NONE', #26106, #46366, #26741 ) ;
#9408 = DIRECTION ( 'NONE',  ( 0.000000000000000000, 1.000000000000000000, 0.000000000000000000 ) ) ;
#9409 = VERTEX_POINT ( 'NONE', #128866 ) ;
#9410 = VERTEX_POINT ( 'NONE', #18871 ) ;
#9411 = DIRECTION ( 'NONE',  ( -4.274815082592931898E-19, -0.9999939076577903929, -0.003490651415223739937 ) ) ;
#9412 = DIRECTION ( 'NONE',  ( 0.000000000000000000, 0.000000000000000000, 1.000000000000000000 ) ) ;
#9413 = CARTESIAN_POINT ( 'NONE',  ( 2.099999999999950351, 2.500000000000000000, -0.6928203230275541413 ) ) ;
#9414 = CONICAL_SURFACE ( 'NONE', #84627, 0.1000000000000002554, 0.003490658503988666988 ) ;
#9415 = DIRECTION ( 'NONE',  ( 0.000000000000000000, 1.000000000000000000, 0.000000000000000000 ) ) ;
#9416 = DIRECTION ( 'NONE',  ( 0.000000000000000000, 0.000000000000000000, 1.000000000000000000 ) ) ;
#9417 = EDGE_LOOP ( 'NONE', ( #9018, #124719 ) ) ;
#9418 = DIRECTION ( 'NONE',  ( 0.000000000000000000, 1.000000000000000000, 0.000000000000000000 ) ) ;
#9419 = ORIENTED_EDGE ( 'NONE', *, *, #26086, .T. ) ;
#9420 = CARTESIAN_POINT ( 'NONE',  ( 16.55712575656009733, 0.2764121571832068303, 6.093697237269479317 ) ) ;
#9421 = VERTEX_POINT ( 'NONE', #58182 ) ;
#9422 = CARTESIAN_POINT ( 'NONE',  ( 112.4803320538941875, 8.411414713183589242, 2.243816228936815538 ) ) ;
#9423 = CARTESIAN_POINT ( 'NONE',  ( -10.45000000000000462, 2.500000000000000000, -6.495190528383298911 ) ) ;
#9424 = ORIENTED_EDGE ( 'NONE', *, *, #86245, .F. ) ;
#9425 = DIRECTION ( 'NONE',  ( -0.000000000000000000, 1.000000000000000000, -0.000000000000000000 ) ) ;
#9426 = CARTESIAN_POINT ( 'NONE',  ( 12.29999999999990123, 12.50000000000000000, 0.2813168883297361700 ) ) ;
#9427 = CIRCLE ( 'NONE', #90984, 0.1000000000000002554 ) ;
#9428 = VERTEX_POINT ( 'NONE', #58811 ) ;
#9429 = EDGE_CURVE ( 'NONE', #69132, #114300, #128120, .T. ) ;
#9430 = AXIS2_PLACEMENT_3D ( 'NONE', #69729, #111586, #10774 ) ;
#9432 = CARTESIAN_POINT ( 'NONE',  ( 9.349999999999919709, 2.500000000000000000, 1.918653347947321564 ) ) ;
#9431 = AXIS2_PLACEMENT_3D ( 'NONE', #17288, #76890, #14719 ) ;
#9433 = ADVANCED_FACE ( 'NONE', ( #129511 ), #107901, .F. ) ;
#9434 = ORIENTED_EDGE ( 'NONE', *, *, #49696, .F. ) ;
#9435 = VECTOR ( 'NONE', #34842, 1000.000000000000000 ) ;
#9436 = ORIENTED_EDGE ( 'NONE', *, *, #8937, .F. ) ;
#9437 = DIRECTION ( 'NONE',  ( -0.000000000000000000, 1.000000000000000000, -0.000000000000000000 ) ) ;
#9438 = DIRECTION ( 'NONE',  ( -0.000000000000000000, 1.000000000000000000, -0.000000000000000000 ) ) ;
#9439 = DIRECTION ( 'NONE',  ( 0.000000000000000000, 1.000000000000000000, 0.000000000000000000 ) ) ;
#9440 = DIRECTION ( 'NONE',  ( 0.000000000000000000, 1.000000000000000000, 0.000000000000000000 ) ) ;
#9441 = CIRCLE ( 'NONE', #40761, 0.1000000000000002554 ) ;
#9442 = CARTESIAN_POINT ( 'NONE',  ( 9.599999999999917932, 2.500000000000000000, 0.6928203230275494784 ) ) ;
#9443 = AXIS2_PLACEMENT_3D ( 'NONE', #123036, #90986, #1311 ) ;
#9444 = ORIENTED_EDGE ( 'NONE', *, *, #44376, .F. ) ;
#9445 = AXIS2_PLACEMENT_3D ( 'NONE', #108252, #99739, #27123 ) ;
#9446 = DIRECTION ( 'NONE',  ( 0.000000000000000000, 0.000000000000000000, -1.000000000000000000 ) ) ;
#9447 = AXIS2_PLACEMENT_3D ( 'NONE', #120852, #70463, #71758 ) ;
#9448 = ORIENTED_EDGE ( 'NONE', *, *, #34066, .F. ) ;
#9449 = AXIS2_PLACEMENT_3D ( 'NONE', #93952, #25854, #122764 ) ;
#9450 = CARTESIAN_POINT ( 'NONE',  ( -4.400000000000025224, 12.50000000000000000, -0.3464101615137783474 ) ) ;
#9452 = CONICAL_SURFACE ( 'NONE', #24030, 0.1000000000000000472, 0.003490658503988666988 ) ;
#9451 = DIRECTION ( 'NONE',  ( 0.000000000000000000, 0.000000000000000000, 1.000000000000000000 ) ) ;
#9453 = AXIS2_PLACEMENT_3D ( 'NONE', #80919, #61280, #88797 ) ;
#9454 = CARTESIAN_POINT ( 'NONE',  ( 11.84999999999990727, 2.500000000000000000, -1.818653347947326138 ) ) ;
#9455 = CARTESIAN_POINT ( 'NONE',  ( -1.050000000000037348, 12.50000000000000000, -2.446380397790840266 ) ) ;
#9456 = DIRECTION ( 'NONE',  ( -4.274815082592931898E-19, -0.9999939076577903929, -0.003490651415223739937 ) ) ;
#9457 = DIRECTION ( 'NONE',  ( 0.000000000000000000, 0.000000000000000000, 1.000000000000000000 ) ) ;
#9458 = CARTESIAN_POINT ( 'NONE',  ( -4.550000000000026468, 12.50000000000000000, -6.495190528383302464 ) ) ;
#9459 = ORIENTED_EDGE ( 'NONE', *, *, #74083, .T. ) ;
#9460 = DIRECTION ( 'NONE',  ( 0.000000000000000000, 0.000000000000000000, 1.000000000000000000 ) ) ;
#9461 = CARTESIAN_POINT ( 'NONE',  ( -11.05000000000000071, 12.50000000000000000, 6.776507416713035248 ) ) ;
#9462 = PRESENTATION_STYLE_ASSIGNMENT (( #69663 ) ) ;
#9463 = CIRCLE ( 'NONE', #51254, 0.06509327318403745899 ) ;
#9464 = ORIENTED_EDGE ( 'NONE', *, *, #122283, .T. ) ;
#9465 = CARTESIAN_POINT ( 'NONE',  ( -11.25000000000000000, 2.500000000000000000, -7.088010851410849966 ) ) ;
#9466 = EDGE_CURVE ( 'NONE', #106163, #34203, #109846, .T. ) ;
#9467 = ORIENTED_EDGE ( 'NONE', *, *, #78260, .T. ) ;
#9468 = VERTEX_POINT ( 'NONE', #59484 ) ;
#9469 = FACE_OUTER_BOUND ( 'NONE', #125015, .T. ) ;
#9470 = AXIS2_PLACEMENT_3D ( 'NONE', #51873, #121249, #23050 ) ;
#9471 = ORIENTED_EDGE ( 'NONE', *, *, #62734, .T. ) ;
#9472 = DIRECTION ( 'NONE',  ( -0.000000000000000000, -1.000000000000000000, -0.000000000000000000 ) ) ;
#9473 = DIRECTION ( 'NONE',  ( 0.000000000000000000, 1.000000000000000000, 0.000000000000000000 ) ) ;
#9474 = VECTOR ( 'NONE', #22593, 1000.000000000000000 ) ;
#9475 = AXIS2_PLACEMENT_3D ( 'NONE', #62636, #82917, #50871 ) ;
#9476 = VERTEX_POINT ( 'NONE', #88916 ) ;
#9477 = DIRECTION ( 'NONE',  ( -4.274815082592931898E-19, -0.9999939076577903929, -0.003490651415223739937 ) ) ;
#9479 = ORIENTED_EDGE ( 'NONE', *, *, #25895, .T. ) ;
#9478 = CARTESIAN_POINT ( 'NONE',  ( -4.400000000000025224, 2.500000000000000000, -0.3464101615137783474 ) ) ;
#9480 = EDGE_CURVE ( 'NONE', #85840, #17226, #82044, .T. ) ;
#9481 = DIRECTION ( 'NONE',  ( 0.000000000000000000, 0.000000000000000000, 1.000000000000000000 ) ) ;
#9482 = DIRECTION ( 'NONE',  ( -0.000000000000000000, -1.000000000000000000, -0.000000000000000000 ) ) ;
#9483 = EDGE_CURVE ( 'NONE', #17558, #94655, #80100, .T. ) ;
#9484 = ORIENTED_EDGE ( 'NONE', *, *, #98562, .T. ) ;
#9485 = CIRCLE ( 'NONE', #63783, 0.06509327318403745899 ) ;
#9486 = VERTEX_POINT ( 'NONE', #118363 ) ;
#9487 = AXIS2_PLACEMENT_3D ( 'NONE', #98053, #117666, #89526 ) ;
#9488 = ORIENTED_EDGE ( 'NONE', *, *, #86360, .T. ) ;
#9489 = DIRECTION ( 'NONE',  ( 0.000000000000000000, 0.000000000000000000, 1.000000000000000000 ) ) ;
#9490 = CARTESIAN_POINT ( 'NONE',  ( 2.899999999999944844, 2.500000000000000000, 3.637306695894644726 ) ) ;
#9491 = CARTESIAN_POINT ( 'NONE',  ( -10.40000000000000213, 12.50000000000000000, -4.395220292106235327 ) ) ;
#9492 = EDGE_CURVE ( 'NONE', #60798, #24108, #19438, .T. ) ;
#9493 = FACE_BOUND ( 'NONE', #100702, .T. ) ;
#9494 = VERTEX_POINT ( 'NONE', #28062 ) ;
#9495 = CARTESIAN_POINT ( 'NONE',  ( 8.149999999999923972, 12.50000000000000000, -6.841600689897077814 ) ) ;
#9496 = CARTESIAN_POINT ( 'NONE',  ( -4.350000000000027178, 2.500000000000000000, -6.148780366869526226 ) ) ;
#9497 = ORIENTED_EDGE ( 'NONE', *, *, #61825, .F. ) ;
#9498 = DIRECTION ( 'NONE',  ( -0.6795087154616692438, 6.363550617825454546E-16, -0.7336674352945157240 ) ) ;
#9500 = LINE ( 'NONE', #118801, #80523 ) ;
#9499 = AXIS2_PLACEMENT_3D ( 'NONE', #122036, #11426, #72926 ) ;
#9501 = AXIS2_PLACEMENT_3D ( 'NONE', #831, #10624, #112732 ) ;
#9502 = DIRECTION ( 'NONE',  ( -0.000000000000000000, -1.000000000000000000, -0.000000000000000000 ) ) ;
#9503 = CARTESIAN_POINT ( 'NONE',  ( -9.550000000000006040, 2.500000000000000000, 2.165063509461097713 ) ) ;
#9504 = DIRECTION ( 'NONE',  ( 0.000000000000000000, 1.000000000000000000, 0.000000000000000000 ) ) ;
#9505 = DIRECTION ( 'NONE',  ( -0.000000000000000000, 1.000000000000000000, -0.000000000000000000 ) ) ;
#9506 = DIRECTION ( 'NONE',  ( 0.000000000000000000, 0.000000000000000000, -1.000000000000000000 ) ) ;
#9507 = VERTEX_POINT ( 'NONE', #99386 ) ;
#9508 = ORIENTED_EDGE ( 'NONE', *, *, #43455, .F. ) ;
#9509 = VERTEX_POINT ( 'NONE', #87610 ) ;
#9510 = VECTOR ( 'NONE', #31929, 1000.000000000000000 ) ;
#9511 = ORIENTED_EDGE ( 'NONE', *, *, #15275, .F. ) ;
#9512 = ORIENTED_EDGE ( 'NONE', *, *, #119176, .T. ) ;
#9513 = PLANE ( 'NONE',  #127940 ) ;
#9514 = FACE_OUTER_BOUND ( 'NONE', #123325, .T. ) ;
#9515 = VERTEX_POINT ( 'NONE', #60118 ) ;
#9516 = FACE_BOUND ( 'NONE', #83588, .T. ) ;
#9517 = VECTOR ( 'NONE', #100666, 1000.000000000000000 ) ;
#9518 = DIRECTION ( 'NONE',  ( 0.000000000000000000, 1.000000000000000000, 0.000000000000000000 ) ) ;
#9519 = EDGE_CURVE ( 'NONE', #57536, #117403, #9708, .T. ) ;
#9520 = CONICAL_SURFACE ( 'NONE', #42904, 0.1000000000000002554, 0.003490658503988666988 ) ;
#9521 = DIRECTION ( 'NONE',  ( 0.000000000000000000, 1.000000000000000000, 0.000000000000000000 ) ) ;
#9522 = CIRCLE ( 'NONE', #28404, 0.1000000000000002554 ) ;
#9523 = FACE_OUTER_BOUND ( 'NONE', #31925, .T. ) ;
#9524 = DIRECTION ( 'NONE',  ( 0.000000000000000000, 0.000000000000000000, 1.000000000000000000 ) ) ;
#9525 = FACE_OUTER_BOUND ( 'NONE', #112386, .T. ) ;
#9526 = ADVANCED_FACE ( 'NONE', ( #69919 ), #42456, .T. ) ;
#9527 = DIRECTION ( 'NONE',  ( 0.000000000000000000, 1.000000000000000000, 0.000000000000000000 ) ) ;
#9528 = ORIENTED_EDGE ( 'NONE', *, *, #18097, .F. ) ;
#9529 = ADVANCED_FACE ( 'NONE', ( #60744 ), #48803, .T. ) ;
#9530 = AXIS2_PLACEMENT_3D ( 'NONE', #16474, #77993, #67503 ) ;
#9531 = VERTEX_POINT ( 'NONE', #89553 ) ;
#9532 = ORIENTED_EDGE ( 'NONE', *, *, #97864, .T. ) ;
#9533 = EDGE_LOOP ( 'NONE', ( #14337, #32365 ) ) ;
#9534 = ADVANCED_FACE ( 'NONE', ( #90173 ), #117722, .T. ) ;
#9535 = CIRCLE ( 'NONE', #126516, 0.06509327318403745899 ) ;
#9537 = ADVANCED_FACE ( 'NONE', ( #80393 ), #101020, .T. ) ;
#9536 = CARTESIAN_POINT ( 'NONE',  ( 10.06913504599038589, 2.500000000000000444, 8.158951466667705432 ) ) ;
#9538 = DIRECTION ( 'NONE',  ( 0.000000000000000000, -0.000000000000000000, 1.000000000000000000 ) ) ;
#9540 = ORIENTED_EDGE ( 'NONE', *, *, #104981, .T. ) ;
#9539 = ADVANCED_FACE ( 'NONE', ( #49005 ), #39194, .T. ) ;
#9541 = DIRECTION ( 'NONE',  ( 0.000000000000000000, -0.000000000000000000, 1.000000000000000000 ) ) ;
#9542 = VECTOR ( 'NONE', #80111, 1000.000000000000000 ) ;
#9543 = AXIS2_PLACEMENT_3D ( 'NONE', #6748, #46711, #86627 ) ;
#9544 = DIRECTION ( 'NONE',  ( 0.000000000000000000, 0.000000000000000000, 1.000000000000000000 ) ) ;
#9545 = AXIS2_PLACEMENT_3D ( 'NONE', #19183, #101645, #29675 ) ;
#9547 = EDGE_CURVE ( 'NONE', #4520, #78724, #25706, .T. ) ;
#9546 = DIRECTION ( 'NONE',  ( 0.000000000000000000, 0.000000000000000000, 1.000000000000000000 ) ) ;
#9548 = CARTESIAN_POINT ( 'NONE',  ( 186.2760416670080588, 6.551208109652274736, 3.782341765625001351 ) ) ;
#9549 = DIRECTION ( 'NONE',  ( -0.000000000000000000, -1.000000000000000000, -0.000000000000000000 ) ) ;
#9550 = DIRECTION ( 'NONE',  ( 0.000000000000000000, 0.000000000000000000, 1.000000000000000000 ) ) ;
#9551 = DIRECTION ( 'NONE',  ( 0.000000000000000000, 0.000000000000000000, 1.000000000000000000 ) ) ;
#9552 = EDGE_LOOP ( 'NONE', ( #65835, #97726, #118168, #57625 ) ) ;
#9553 = CARTESIAN_POINT ( 'NONE',  ( 7.499999999999961808, 12.50000000000000000, 4.265033745738159077 ) ) ;
#9554 = EDGE_CURVE ( 'NONE', #72741, #106830, #98080, .T. ) ;
#9555 = EDGE_LOOP ( 'NONE', ( #7857, #107446, #48874, #51348 ) ) ;
#9556 = ORIENTED_EDGE ( 'NONE', *, *, #88559, .F. ) ;
#9557 = DIRECTION ( 'NONE',  ( 0.000000000000000000, -0.000000000000000000, 1.000000000000000000 ) ) ;
#9558 = CARTESIAN_POINT ( 'NONE',  ( -14.14999999999998614, 2.500000000000000000, -2.165063509461099489 ) ) ;
#9559 = DIRECTION ( 'NONE',  ( 0.000000000000000000, -1.000000000000000000, 0.000000000000000000 ) ) ;
#9560 = CIRCLE ( 'NONE', #53389, 0.06509327318403741736 ) ;
#9561 = ORIENTED_EDGE ( 'NONE', *, *, #70626, .F. ) ;
#9562 = EDGE_LOOP ( 'NONE', ( #126635, #7600 ) ) ;
#9563 = CARTESIAN_POINT ( 'NONE',  ( 3.949999999999942446, 2.500000000000000000, -2.511473670974877948 ) ) ;
#9564 = FACE_OUTER_BOUND ( 'NONE', #49629, .T. ) ;
#9565 = CARTESIAN_POINT ( 'NONE',  ( 14.34999999999989306, 12.50000000000000000, -2.576566944158915184 ) ) ;
#9566 = ORIENTED_EDGE ( 'NONE', *, *, #114056, .T. ) ;
#9567 = DIRECTION ( 'NONE',  ( 0.000000000000000000, 1.000000000000000000, 0.000000000000000000 ) ) ;
#9568 = AXIS2_PLACEMENT_3D ( 'NONE', #121725, #81794, #80533 ) ;
#9569 = VECTOR ( 'NONE', #109503, 1000.000000000000000 ) ;
#9570 = ORIENTED_EDGE ( 'NONE', *, *, #100064, .T. ) ;
#9572 = AXIS2_PLACEMENT_3D ( 'NONE', #70354, #42189, #21914 ) ;
#9571 = CARTESIAN_POINT ( 'NONE',  ( 11.24999999999994316, 12.50000000000000000, 2.165063509461097713 ) ) ;
#9573 = EDGE_LOOP ( 'NONE', ( #16113, #91803 ) ) ;
#9574 = AXIS2_PLACEMENT_3D ( 'NONE', #129129, #39463, #11898 ) ;
#9575 = DIRECTION ( 'NONE',  ( -0.000000000000000000, 1.000000000000000000, -0.000000000000000000 ) ) ;
#9576 = CARTESIAN_POINT ( 'NONE',  ( 142.3152275665817115, 0.5000000000000000000, 4.152444035927816302 ) ) ;
#9577 = PLANE ( 'NONE',  #19715 ) ;
#9578 = DIRECTION ( 'NONE',  ( 0.000000000000000000, -0.000000000000000000, 1.000000000000000000 ) ) ;
#9579 = VERTEX_POINT ( 'NONE', #62687 ) ;
#9580 = DIRECTION ( 'NONE',  ( -4.274815082592931898E-19, -0.9999939076577903929, -0.003490651415223739937 ) ) ;
#9581 = EDGE_CURVE ( 'NONE', #125530, #102565, #96803, .T. ) ;
#9583 = AXIS2_PLACEMENT_3D ( 'NONE', #100330, #86787, #27223 ) ;
#9582 = CONICAL_SURFACE ( 'NONE', #82754, 0.09999999999999982514, 0.003490658503988666988 ) ;
#9584 = ORIENTED_EDGE ( 'NONE', *, *, #108031, .F. ) ;
#9585 = ORIENTED_EDGE ( 'NONE', *, *, #93523, .F. ) ;
#9586 = FACE_OUTER_BOUND ( 'NONE', #20543, .T. ) ;
#9587 = CARTESIAN_POINT ( 'NONE',  ( -5.850000000000018296, 12.50000000000000000, 7.253104124594885960 ) ) ;
#9588 = CARTESIAN_POINT ( 'NONE',  ( -6.650000000000018119, 12.50000000000000000, -2.792790559304616504 ) ) ;
#9589 = CARTESIAN_POINT ( 'NONE',  ( 12.09999999999990550, 12.50000000000000000, -4.330127018922201643 ) ) ;
#9590 = CARTESIAN_POINT ( 'NONE',  ( -8.950000000000006395, 12.50000000000000000, 6.841600689897072485 ) ) ;
#9591 = DIRECTION ( 'NONE',  ( -0.000000000000000000, -1.000000000000000000, -0.000000000000000000 ) ) ;
#9592 = EDGE_CURVE ( 'NONE', #42850, #59613, #46640, .T. ) ;
#9593 = CIRCLE ( 'NONE', #34655, 0.1000000000000002554 ) ;
#9594 = CONICAL_SURFACE ( 'NONE', #30545, 0.1000000000000002554, 0.003490658503988666988 ) ;
#9595 = DIRECTION ( 'NONE',  ( 0.000000000000000000, 0.000000000000000000, -1.000000000000000000 ) ) ;
#9596 = CARTESIAN_POINT ( 'NONE',  ( -4.600000000000028955, 2.500000000000000000, -4.430127018922202176 ) ) ;
#9597 = DIRECTION ( 'NONE',  ( 0.000000000000000000, -0.9999939076577903929, 0.003490651415223739937 ) ) ;
#9598 = VERTEX_POINT ( 'NONE', #113711 ) ;
#9599 = DIRECTION ( 'NONE',  ( -1.000000000000000000, -0.000000000000000000, -0.000000000000000000 ) ) ;
#9600 = PLANE ( 'NONE',  #123148 ) ;
#9601 = CARTESIAN_POINT ( 'NONE',  ( 0.6499999999999543920, 2.500000000000000000, 6.741600689897071952 ) ) ;
#9602 = FACE_OUTER_BOUND ( 'NONE', #58722, .T. ) ;
#9603 = DIRECTION ( 'NONE',  ( 0.000000000000000000, 0.000000000000000000, 1.000000000000000000 ) ) ;
#9604 = ORIENTED_EDGE ( 'NONE', *, *, #84640, .F. ) ;
#9605 = DIRECTION ( 'NONE',  ( -0.000000000000000000, -1.000000000000000000, -0.000000000000000000 ) ) ;
#9606 = CIRCLE ( 'NONE', #40939, 0.06509327318403745899 ) ;
#9607 = AXIS2_PLACEMENT_3D ( 'NONE', #20393, #11844, #110063 ) ;
#9608 = CARTESIAN_POINT ( 'NONE',  ( 4.349999999999940137, 2.500000000000000000, -6.841600689897078702 ) ) ;
#9610 = ORIENTED_EDGE ( 'NONE', *, *, #97126, .F. ) ;
#9609 = PLANE ( 'NONE',  #88055 ) ;
#9611 = ORIENTED_EDGE ( 'NONE', *, *, #44394, .T. ) ;
#9612 = CONICAL_SURFACE ( 'NONE', #45418, 0.09999999999999982514, 0.003490658503988666988 ) ;
#9613 = DIRECTION ( 'NONE',  ( -4.274815082592931898E-19, -0.9999939076577903929, -0.003490651415223739937 ) ) ;
#9614 = ADVANCED_FACE ( 'NONE', ( #103248 ), #34130, .T. ) ;
#9615 = EDGE_LOOP ( 'NONE', ( #94078, #21722, #26798, #60605 ) ) ;
#9616 = ORIENTED_EDGE ( 'NONE', *, *, #35927, .T. ) ;
#9617 = VERTEX_POINT ( 'NONE', #82967 ) ;
#9618 = LINE ( 'NONE', #68533, #63357 ) ;
#9619 = AXIS2_PLACEMENT_3D ( 'NONE', #106993, #56600, #66434 ) ;
#9620 = DIRECTION ( 'NONE',  ( 0.000000000000000000, 0.000000000000000000, 1.000000000000000000 ) ) ;
#9621 = DIRECTION ( 'NONE',  ( -4.274815082592931898E-19, -0.9999939076577903929, -0.003490651415223739937 ) ) ;
#9622 = AXIS2_PLACEMENT_3D ( 'NONE', #116003, #26995, #66253 ) ;
#9623 = LINE ( 'NONE', #8964, #20695 ) ;
#9624 = EDGE_CURVE ( 'NONE', #95428, #62002, #23654, .T. ) ;
#9625 = ORIENTED_EDGE ( 'NONE', *, *, #3190, .F. ) ;
#9627 = AXIS2_PLACEMENT_3D ( 'NONE', #92180, #101375, #50997 ) ;
#9626 = CARTESIAN_POINT ( 'NONE',  ( -11.44999999999999929, 12.50000000000000000, -1.883746621131359600 ) ) ;
#9628 = ORIENTED_EDGE ( 'NONE', *, *, #72659, .F. ) ;
#9629 = CARTESIAN_POINT ( 'NONE',  ( -13.74999999999995381, 12.50000000000000000, 2.165063509461101265 ) ) ;
#9630 = EDGE_CURVE ( 'NONE', #27914, #66020, #109329, .T. ) ;
#9631 = CARTESIAN_POINT ( 'NONE',  ( 18.93069778776535017, 2.571126379696623943, 2.451182541064385489 ) ) ;
#9632 = CARTESIAN_POINT ( 'NONE',  ( 2.099999999999950351, 12.50000000000000000, -4.330127018922201643 ) ) ;
#9633 = DIRECTION ( 'NONE',  ( -0.000000000000000000, 1.000000000000000000, -0.000000000000000000 ) ) ;
#9634 = EDGE_CURVE ( 'NONE', #115142, #13760, #101956, .T. ) ;
#9635 = EDGE_LOOP ( 'NONE', ( #112073, #54024 ) ) ;
#9636 = EDGE_LOOP ( 'NONE', ( #33222, #99534 ) ) ;
#9638 = ORIENTED_EDGE ( 'NONE', *, *, #39541, .T. ) ;
#9637 = EDGE_CURVE ( 'NONE', #67575, #106091, #63372, .T. ) ;
#9639 = EDGE_LOOP ( 'NONE', ( #68602, #26178 ) ) ;
#9640 = ORIENTED_EDGE ( 'NONE', *, *, #3917, .T. ) ;
#9641 = DIRECTION ( 'NONE',  ( 0.000000000000000000, 0.000000000000000000, 1.000000000000000000 ) ) ;
#9642 = DIRECTION ( 'NONE',  ( -0.000000000000000000, -1.000000000000000000, -0.000000000000000000 ) ) ;
#9643 = DIRECTION ( 'NONE',  ( 0.000000000000000000, 0.000000000000000000, -1.000000000000000000 ) ) ;
#9644 = ADVANCED_FACE ( 'NONE', ( #123512 ), #51577, .T. ) ;
#9645 = FACE_BOUND ( 'NONE', #23800, .T. ) ;
#9646 = CARTESIAN_POINT ( 'NONE',  ( 1.049999999999952083, 12.50000000000000000, 6.906693963081109722 ) ) ;
#9647 = CIRCLE ( 'NONE', #124576, 0.06509327318403745899 ) ;
#9648 = DIRECTION ( 'NONE',  ( -0.000000000000000000, -1.000000000000000000, -0.000000000000000000 ) ) ;
#9649 = CARTESIAN_POINT ( 'NONE',  ( 3.949999999999938893, 12.50000000000000000, 6.148780366869520009 ) ) ;
#9650 = DIRECTION ( 'NONE',  ( 0.000000000000000000, 0.000000000000000000, 1.000000000000000000 ) ) ;
#9651 = CIRCLE ( 'NONE', #43409, 0.1000000000000002554 ) ;
#9652 = DIRECTION ( 'NONE',  ( 0.000000000000000000, 1.000000000000000000, 0.000000000000000000 ) ) ;
#9653 = CIRCLE ( 'NONE', #41072, 0.06509327318403745899 ) ;
#9654 = DIRECTION ( 'NONE',  ( 0.000000000000000000, 1.000000000000000000, 0.000000000000000000 ) ) ;
#9655 = DIRECTION ( 'NONE',  ( 0.000000000000000000, -0.9999939076577903929, 0.003490651415223739937 ) ) ;
#9656 = AXIS2_PLACEMENT_3D ( 'NONE', #66322, #47344, #54558 ) ;
#9657 = CONICAL_SURFACE ( 'NONE', #103841, 0.1000000000000000472, 0.003490658503988666988 ) ;
#9658 = DIRECTION ( 'NONE',  ( 0.000000000000000000, 0.000000000000000000, 1.000000000000000000 ) ) ;
#9659 = CIRCLE ( 'NONE', #103670, 0.09999999999999982514 ) ;
#9660 = EDGE_LOOP ( 'NONE', ( #103057, #29266 ) ) ;
#9661 = ORIENTED_EDGE ( 'NONE', *, *, #80016, .F. ) ;
#9662 = VERTEX_POINT ( 'NONE', #22771 ) ;
#9663 = ORIENTED_EDGE ( 'NONE', *, *, #16748, .F. ) ;
#9664 = CARTESIAN_POINT ( 'NONE',  ( 3.149999999999942624, 12.50000000000000000, 6.841600689897072485 ) ) ;
#9665 = DIRECTION ( 'NONE',  ( -0.000000000000000000, -1.000000000000000000, -0.000000000000000000 ) ) ;
#9666 = FACE_BOUND ( 'NONE', #70858, .T. ) ;
#9668 = DIRECTION ( 'NONE',  ( 0.000000000000000000, 0.000000000000000000, -1.000000000000000000 ) ) ;
#9667 = AXIS2_PLACEMENT_3D ( 'NONE', #34620, #17518, #114433 ) ;
#9670 = AXIS2_PLACEMENT_3D ( 'NONE', #71500, #111412, #81963 ) ;
#9669 = CIRCLE ( 'NONE', #49403, 0.06509327318403745899 ) ;
#9671 = ORIENTED_EDGE ( 'NONE', *, *, #98562, .F. ) ;
#9672 = DIRECTION ( 'NONE',  ( 0.000000000000000000, -0.9999939076577903929, 0.003490651415223739937 ) ) ;
#9673 = CARTESIAN_POINT ( 'NONE',  ( 1.249999999999952038, 2.500000000000000000, 2.857883832488649301 ) ) ;
#9674 = CARTESIAN_POINT ( 'NONE',  ( 9.149999999999916866, 2.500000000000000000, 7.188010851410848723 ) ) ;
#9675 = DIRECTION ( 'NONE',  ( -0.000000000000000000, -1.000000000000000000, -0.000000000000000000 ) ) ;
#9676 = ORIENTED_EDGE ( 'NONE', *, *, #112270, .F. ) ;
#9677 = DIRECTION ( 'NONE',  ( 0.000000000000000000, 0.000000000000000000, 1.000000000000000000 ) ) ;
#9678 = ADVANCED_FACE ( 'NONE', ( #43065 ), #50933, .T. ) ;
#9679 = VERTEX_POINT ( 'NONE', #82325 ) ;
#9680 = EDGE_CURVE ( 'NONE', #41032, #60331, #73140, .T. ) ;
#9681 = ORIENTED_EDGE ( 'NONE', *, *, #63486, .T. ) ;
#9682 = EDGE_CURVE ( 'NONE', #76788, #1255, #52909, .T. ) ;
#9683 = DIRECTION ( 'NONE',  ( 0.000000000000000000, 0.000000000000000000, 1.000000000000000000 ) ) ;
#9684 = DIRECTION ( 'NONE',  ( -0.000000000000000000, 1.000000000000000000, -0.000000000000000000 ) ) ;
#9686 = ORIENTED_EDGE ( 'NONE', *, *, #33016, .T. ) ;
#9685 = EDGE_CURVE ( 'NONE', #3071, #74230, #12900, .T. ) ;
#9687 = ADVANCED_FACE ( 'NONE', ( #52855 ), #121956, .T. ) ;
#9688 = LINE ( 'NONE', #56824, #101190 ) ;
#9689 = CARTESIAN_POINT ( 'NONE',  ( -11.05000000000000249, 2.500000000000000000, -6.048780366869523029 ) ) ;
#9690 = ORIENTED_EDGE ( 'NONE', *, *, #125934, .F. ) ;
#9692 = EDGE_CURVE ( 'NONE', #1314, #102047, #50849, .T. ) ;
#9691 = CARTESIAN_POINT ( 'NONE',  ( 3.149999999999946176, 12.50000000000000000, -1.818653347947325916 ) ) ;
#9693 = ORIENTED_EDGE ( 'NONE', *, *, #122072, .T. ) ;
#9694 = DIRECTION ( 'NONE',  ( 0.000000000000000000, 1.000000000000000000, 0.000000000000000000 ) ) ;
#9695 = ORIENTED_EDGE ( 'NONE', *, *, #85223, .T. ) ;
#9696 = DIRECTION ( 'NONE',  ( 0.000000000000000000, 1.000000000000000000, 0.000000000000000000 ) ) ;
#9697 = FACE_BOUND ( 'NONE', #95872, .T. ) ;
#9698 = ADVANCED_FACE ( 'NONE', ( #2443 ), #93424, .T. ) ;
#9699 = EDGE_CURVE ( 'NONE', #27344, #65690, #100646, .T. ) ;
#9700 = VECTOR ( 'NONE', #127697, 1000.000000000000000 ) ;
#9701 = EDGE_LOOP ( 'NONE', ( #74981, #73284 ) ) ;
#9702 = AXIS2_PLACEMENT_3D ( 'NONE', #74637, #35373, #95575 ) ;
#9703 = DIRECTION ( 'NONE',  ( -0.000000000000000000, 1.000000000000000000, -0.000000000000000000 ) ) ;
#9704 = ORIENTED_EDGE ( 'NONE', *, *, #89209, .F. ) ;
#9705 = CARTESIAN_POINT ( 'NONE',  ( 5.649999999999936406, 2.500000000000000000, -6.148780366869526226 ) ) ;
#9706 = CARTESIAN_POINT ( 'NONE',  ( -8.750000000000007105, 12.50000000000000000, 7.122917578226811486 ) ) ;
#9707 = CARTESIAN_POINT ( 'NONE',  ( -11.24999999999996447, 12.50000000000000000, -6.560283801567336148 ) ) ;
#9708 = LINE ( 'NONE', #30004, #36191 ) ;
#9709 = DIRECTION ( 'NONE',  ( 0.000000000000000000, 0.000000000000000000, -1.000000000000000000 ) ) ;
#9710 = EDGE_LOOP ( 'NONE', ( #17713, #116716 ) ) ;
#9713 = ORIENTED_EDGE ( 'NONE', *, *, #107997, .F. ) ;
#9712 = AXIS2_PLACEMENT_3D ( 'NONE', #3696, #92736, #52799 ) ;
#9711 = CONICAL_SURFACE ( 'NONE', #22249, 0.09999999999999999167, 0.003490658503988666988 ) ;
#9714 = ORIENTED_EDGE ( 'NONE', *, *, #57353, .F. ) ;
#9715 = CARTESIAN_POINT ( 'NONE',  ( -11.25000000000000000, 2.500000000000000000, -2.857883832488649745 ) ) ;
#9716 = DIRECTION ( 'NONE',  ( 0.000000000000000000, 0.000000000000000000, 1.000000000000000000 ) ) ;
#9717 = DIRECTION ( 'NONE',  ( 0.000000000000000000, 1.000000000000000000, 0.000000000000000000 ) ) ;
#9719 = ORIENTED_EDGE ( 'NONE', *, *, #58265, .T. ) ;
#9718 = ORIENTED_EDGE ( 'NONE', *, *, #42804, .T. ) ;
#9720 = ORIENTED_EDGE ( 'NONE', *, *, #110180, .T. ) ;
#9721 = DIRECTION ( 'NONE',  ( 0.000000000000000000, 1.000000000000000000, 0.000000000000000000 ) ) ;
#9723 = AXIS2_PLACEMENT_3D ( 'NONE', #87861, #8650, #59074 ) ;
#9722 = CONICAL_SURFACE ( 'NONE', #11853, 0.1000000000000002554, 0.003490658503988666988 ) ;
#9724 = DIRECTION ( 'NONE',  ( 0.000000000000000000, -0.000000000000000000, 1.000000000000000000 ) ) ;
#9725 = AXIS2_PLACEMENT_3D ( 'NONE', #112598, #123672, #124350 ) ;
#9726 = APPLICATION_PROTOCOL_DEFINITION ( 'draft international standard', 'automotive_design', 1998, #24625 ) ;
#9727 = DIRECTION ( 'NONE',  ( 0.000000000000000000, -0.000000000000000000, 1.000000000000000000 ) ) ;
#9728 = LINE ( 'NONE', #69939, #33605 ) ;
#9729 = CARTESIAN_POINT ( 'NONE',  ( 8.549999999999918998, 2.500000000000000000, 6.741600689897071952 ) ) ;
#9730 = CARTESIAN_POINT ( 'NONE',  ( 185.7083333333333428, -4.445597072760163471, -7.699999999999919353 ) ) ;
#9731 = DIRECTION ( 'NONE',  ( 0.000000000000000000, -0.9999939076577903929, 0.003490651415223739937 ) ) ;
#9732 = DIRECTION ( 'NONE',  ( 0.000000000000000000, -0.000000000000000000, 1.000000000000000000 ) ) ;
#9733 = EDGE_LOOP ( 'NONE', ( #12367, #52725, #112623, #38120 ) ) ;
#9734 = EDGE_LOOP ( 'NONE', ( #128776, #111263 ) ) ;
#9735 = DIRECTION ( 'NONE',  ( 0.000000000000000000, 1.000000000000000000, 0.000000000000000000 ) ) ;
#9736 = DIRECTION ( 'NONE',  ( 0.000000000000000000, 1.000000000000000000, 0.000000000000000000 ) ) ;
#9737 = VERTEX_POINT ( 'NONE', #111778 ) ;
#9738 = VERTEX_POINT ( 'NONE', #92119 ) ;
#9739 = CARTESIAN_POINT ( 'NONE',  ( 185.6510416670080303, 4.367472073101518859, -7.564683531249999149 ) ) ;
#9740 = CARTESIAN_POINT ( 'NONE',  ( -0.2000000000000412836, 2.500000000000000000, 4.676537180435972552 ) ) ;
#9741 = CONICAL_SURFACE ( 'NONE', #47305, 0.1000000000000002554, 0.003490658503988666988 ) ;
#9742 = LINE ( 'NONE', #49688, #56177 ) ;
#9743 = CONICAL_SURFACE ( 'NONE', #7663, 0.1000000000000002554, 0.003490658503988666988 ) ;
#9744 = DIRECTION ( 'NONE',  ( 0.000000000000000000, 0.000000000000000000, -1.000000000000000000 ) ) ;
#9745 = ADVANCED_FACE ( 'NONE', ( #62041 ), #27858, .T. ) ;
#9746 = DIRECTION ( 'NONE',  ( -0.000000000000000000, -1.000000000000000000, -0.000000000000000000 ) ) ;
#9747 = AXIS2_PLACEMENT_3D ( 'NONE', #117455, #129277, #57943 ) ;
#9748 = DIRECTION ( 'NONE',  ( 0.000000000000000000, 0.000000000000000000, -1.000000000000000000 ) ) ;
#9749 = CARTESIAN_POINT ( 'NONE',  ( -7.500000000000011546, 12.50000000000000000, 3.702399969078682407 ) ) ;
#9750 = AXIS2_PLACEMENT_3D ( 'NONE', #15773, #66167, #5944 ) ;
#9751 = CIRCLE ( 'NONE', #68327, 0.1000000000000002554 ) ;
#9752 = DIRECTION ( 'NONE',  ( 0.000000000000000000, 0.000000000000000000, 1.000000000000000000 ) ) ;
#9753 = ORIENTED_EDGE ( 'NONE', *, *, #9103, .T. ) ;
#9754 = AXIS2_PLACEMENT_3D ( 'NONE', #111895, #124294, #112548 ) ;
#9755 = ORIENTED_EDGE ( 'NONE', *, *, #117610, .F. ) ;
#9756 = VERTEX_POINT ( 'NONE', #65233 ) ;
#9757 = ORIENTED_EDGE ( 'NONE', *, *, #126160, .T. ) ;
#9758 = FACE_OUTER_BOUND ( 'NONE', #103387, .T. ) ;
#9759 = DIRECTION ( 'NONE',  ( -0.000000000000000000, 1.000000000000000000, -0.000000000000000000 ) ) ;
#9760 = CIRCLE ( 'NONE', #66183, 0.1000000000000002554 ) ;
#9761 = ORIENTED_EDGE ( 'NONE', *, *, #14671, .F. ) ;
#9762 = CARTESIAN_POINT ( 'NONE',  ( 9.799999999999913669, 2.500000000000000000, -3.983716857408426293 ) ) ;
#9763 = DIRECTION ( 'NONE',  ( 0.000000000000000000, 0.000000000000000000, 1.000000000000000000 ) ) ;
#9765 = AXIS2_PLACEMENT_3D ( 'NONE', #125731, #84540, #124472 ) ;
#9764 = AXIS2_PLACEMENT_3D ( 'NONE', #44986, #84892, #124829 ) ;
#9766 = CARTESIAN_POINT ( 'NONE',  ( 129.5000000000000000, 0.000000000000000000, -6.000000000000000000 ) ) ;
#9768 = ORIENTED_EDGE ( 'NONE', *, *, #83699, .T. ) ;
#9767 = DIRECTION ( 'NONE',  ( 0.000000000000000000, 0.000000000000000000, 1.000000000000000000 ) ) ;
#9769 = DIRECTION ( 'NONE',  ( 0.000000000000000000, -0.9999939076577903929, 0.003490651415223739937 ) ) ;
#9770 = LINE ( 'NONE', #129576, #106379 ) ;
#9771 = ORIENTED_EDGE ( 'NONE', *, *, #116023, .T. ) ;
#9772 = ORIENTED_EDGE ( 'NONE', *, *, #110161, .T. ) ;
#9773 = ORIENTED_EDGE ( 'NONE', *, *, #30941, .F. ) ;
#9774 = ORIENTED_EDGE ( 'NONE', *, *, #66681, .F. ) ;
#9775 = FACE_OUTER_BOUND ( 'NONE', #68908, .T. ) ;
#9776 = FACE_OUTER_BOUND ( 'NONE', #1579, .T. ) ;
#9777 = DIRECTION ( 'NONE',  ( 0.000000000000000000, -0.000000000000000000, 1.000000000000000000 ) ) ;
#9778 = EDGE_CURVE ( 'NONE', #125732, #27245, #113540, .T. ) ;
#9779 = ORIENTED_EDGE ( 'NONE', *, *, #124799, .T. ) ;
#9780 = DIRECTION ( 'NONE',  ( 0.000000000000000000, 0.000000000000000000, 1.000000000000000000 ) ) ;
#9781 = CARTESIAN_POINT ( 'NONE',  ( 7.099999999999925926, 2.500000000000000000, 0.6928203230275494784 ) ) ;
#9782 = EDGE_CURVE ( 'NONE', #98804, #114933, #84291, .T. ) ;
#9783 = FACE_OUTER_BOUND ( 'NONE', #5889, .T. ) ;
#9784 = DIRECTION ( 'NONE',  ( 0.000000000000000000, 0.000000000000000000, 1.000000000000000000 ) ) ;
#9785 = EDGE_CURVE ( 'NONE', #102868, #117684, #38340, .T. ) ;
#9786 = EDGE_LOOP ( 'NONE', ( #91625, #23686, #60724, #41252 ) ) ;
#9787 = AXIS2_PLACEMENT_3D ( 'NONE', #100799, #19687, #92273 ) ;
#9788 = PLANE ( 'NONE',  #79264 ) ;
#9789 = VECTOR ( 'NONE', #1872, 1000.000000000000000 ) ;
#9790 = ORIENTED_EDGE ( 'NONE', *, *, #94333, .T. ) ;
#9791 = ADVANCED_FACE ( 'NONE', ( #46246 ), #5025, .T. ) ;
#9793 = VERTEX_POINT ( 'NONE', #103889 ) ;
#9792 = EDGE_CURVE ( 'NONE', #115818, #126669, #15321, .T. ) ;
#9794 = CARTESIAN_POINT ( 'NONE',  ( 0.8499999999999553468, 2.500000000000000000, -2.857883832488653741 ) ) ;
#9795 = ADVANCED_FACE ( 'NONE', ( #96620 ), #82155, .T. ) ;
#9796 = LINE ( 'NONE', #98167, #100431 ) ;
#9797 = EDGE_CURVE ( 'NONE', #18483, #77736, #24686, .T. ) ;
#9798 = FACE_BOUND ( 'NONE', #82594, .T. ) ;
#9799 = CARTESIAN_POINT ( 'NONE',  ( 184.5312500006828031, 9.429780353434619030E-16, -7.700000000000000178 ) ) ;
#9800 = DIRECTION ( 'NONE',  ( -0.000000000000000000, 1.000000000000000000, -0.000000000000000000 ) ) ;
#9802 = AXIS2_PLACEMENT_3D ( 'NONE', #11265, #51218, #803 ) ;
#9801 = AXIS2_PLACEMENT_3D ( 'NONE', #109930, #79810, #119727 ) ;
#9803 = CARTESIAN_POINT ( 'NONE',  ( 14.14999999999989555, 2.500000000000000000, 2.065063509461097624 ) ) ;
#9804 = EDGE_LOOP ( 'NONE', ( #38983, #56572 ) ) ;
#9805 = DIRECTION ( 'NONE',  ( -0.000000000000000000, 1.000000000000000000, -0.000000000000000000 ) ) ;
#9806 = DIRECTION ( 'NONE',  ( 0.000000000000000000, 0.000000000000000000, 1.000000000000000000 ) ) ;
#9808 = ADVANCED_FACE ( 'NONE', ( #54773 ), #75970, .T. ) ;
#9807 = VECTOR ( 'NONE', #63634, 1000.000000000000000 ) ;
#9809 = DIRECTION ( 'NONE',  ( 0.000000000000000000, 0.000000000000000000, 1.000000000000000000 ) ) ;
#9810 = CARTESIAN_POINT ( 'NONE',  ( 1.449999999999951772, 2.500000000000000000, -6.148780366869526226 ) ) ;
#9811 = ORIENTED_EDGE ( 'NONE', *, *, #65699, .F. ) ;
#9812 = CIRCLE ( 'NONE', #22350, 0.1000000000000002554 ) ;
#9813 = DIRECTION ( 'NONE',  ( 0.000000000000000000, 0.000000000000000000, -1.000000000000000000 ) ) ;
#9814 = CIRCLE ( 'NONE', #99711, 0.1000000000000000056 ) ;
#9815 = DIRECTION ( 'NONE',  ( 0.000000000000000000, 0.000000000000000000, 1.000000000000000000 ) ) ;
#9816 = EDGE_LOOP ( 'NONE', ( #35705, #53150, #87910, #56757 ) ) ;
#9817 = ORIENTED_EDGE ( 'NONE', *, *, #122609, .F. ) ;
#9818 = LINE ( 'NONE', #81767, #60733 ) ;
#9819 = CARTESIAN_POINT ( 'NONE',  ( 13.09999999999989839, 12.50000000000000000, -0.3464101615137783474 ) ) ;
#9820 = FACE_BOUND ( 'NONE', #71787, .T. ) ;
#9821 = LINE ( 'NONE', #110594, #116257 ) ;
#9822 = DIRECTION ( 'NONE',  ( 1.000000000000000000, 0.000000000000000000, 0.000000000000000000 ) ) ;
#9823 = ORIENTED_EDGE ( 'NONE', *, *, #66936, .F. ) ;
#9825 = EDGE_CURVE ( 'NONE', #10582, #112123, #16765, .T. ) ;
#9824 = DIRECTION ( 'NONE',  ( -0.000000000000000000, -1.000000000000000000, -0.000000000000000000 ) ) ;
#9826 = CARTESIAN_POINT ( 'NONE',  ( 184.6666666666666856, -6.668395609140176816, -3.850000000000003642 ) ) ;
#9827 = VERTEX_POINT ( 'NONE', #36458 ) ;
#9828 = FACE_OUTER_BOUND ( 'NONE', #115970, .T. ) ;
#9829 = DIRECTION ( 'NONE',  ( 0.000000000000000000, 1.000000000000000000, 0.000000000000000000 ) ) ;
#9830 = AXIS2_PLACEMENT_3D ( 'NONE', #121354, #53287, #70975 ) ;
#9831 = EDGE_CURVE ( 'NONE', #85857, #50468, #104524, .T. ) ;
#9832 = ADVANCED_FACE ( 'NONE', ( #125454 ), #76368, .T. ) ;
#9833 = DIRECTION ( 'NONE',  ( 0.000000000000000000, 0.000000000000000000, 1.000000000000000000 ) ) ;
#9834 = CARTESIAN_POINT ( 'NONE',  ( 9.149999999999916866, 2.500000000000000000, -2.757883832488654097 ) ) ;
#9835 = EDGE_CURVE ( 'NONE', #107613, #53181, #124169, .T. ) ;
#9836 = AXIS2_PLACEMENT_3D ( 'NONE', #101928, #32564, #24011 ) ;
#9837 = VERTEX_POINT ( 'NONE', #94702 ) ;
#9838 = AXIS2_PLACEMENT_3D ( 'NONE', #50500, #102196, #90413 ) ;
#9839 = EDGE_CURVE ( 'NONE', #55841, #26633, #103165, .T. ) ;
#9840 = CARTESIAN_POINT ( 'NONE',  ( 2.899999999999946620, 2.500000000000000000, 0.5928203230275495006 ) ) ;
#9841 = CARTESIAN_POINT ( 'NONE',  ( -4.350000000000023626, 12.50000000000000000, -1.883746621131363375 ) ) ;
#9842 = DIRECTION ( 'NONE',  ( 0.000000000000000000, 1.000000000000000000, 0.000000000000000000 ) ) ;
#9843 = CARTESIAN_POINT ( 'NONE',  ( -10.85000000000000142, 2.500000000000000000, -5.702370205355745902 ) ) ;
#9844 = ORIENTED_EDGE ( 'NONE', *, *, #63116, .F. ) ;
#9845 = EDGE_LOOP ( 'NONE', ( #69300, #82147 ) ) ;
#9846 = CIRCLE ( 'NONE', #76657, 0.1000000000000002554 ) ;
#9847 = EDGE_CURVE ( 'NONE', #29739, #21836, #56691, .T. ) ;
#9848 = DIRECTION ( 'NONE',  ( 0.000000000000000000, 0.000000000000000000, 1.000000000000000000 ) ) ;
#9849 = CONICAL_SURFACE ( 'NONE', #43049, 0.09999999999999982514, 0.003490658503988666988 ) ;
#9851 = EDGE_LOOP ( 'NONE', ( #80452, #95524 ) ) ;
#9850 = ADVANCED_FACE ( 'NONE', ( #66528 ), #6942, .T. ) ;
#9852 = FACE_OUTER_BOUND ( 'NONE', #44801, .T. ) ;
#9853 = CARTESIAN_POINT ( 'NONE',  ( -7.900000000000014566, 2.500000000000000000, -4.330127018922201643 ) ) ;
#9854 = EDGE_CURVE ( 'NONE', #64742, #92706, #36295, .T. ) ;
#9857 = EDGE_CURVE ( 'NONE', #1183, #61868, #115676, .T. ) ;
#9856 = AXIS2_PLACEMENT_3D ( 'NONE', #17714, #88385, #126400 ) ;
#9855 = CIRCLE ( 'NONE', #106089, 0.09999999999999982514 ) ;
#9858 = DIRECTION ( 'NONE',  ( 0.000000000000000000, 0.000000000000000000, 1.000000000000000000 ) ) ;
#9859 = ORIENTED_EDGE ( 'NONE', *, *, #16821, .F. ) ;
#9860 = DIRECTION ( 'NONE',  ( 0.000000000000000000, 0.000000000000000000, 1.000000000000000000 ) ) ;
#9861 = CARTESIAN_POINT ( 'NONE',  ( -12.09999999999999432, 2.500000000000000000, 3.637306695894644726 ) ) ;
#9862 = CARTESIAN_POINT ( 'NONE',  ( 0.8499999999999545697, 12.50000000000000000, 2.922977105672686982 ) ) ;
#9863 = CARTESIAN_POINT ( 'NONE',  ( -6.050000000000020250, 2.500000000000000000, -2.611473670974877592 ) ) ;
#9864 = CARTESIAN_POINT ( 'NONE',  ( -9.999999999999971578, 12.50000000000000000, -4.330127018922197202 ) ) ;
#9866 = ADVANCED_FACE ( 'NONE', ( #18072 ), #46742, .T. ) ;
#9865 = CARTESIAN_POINT ( 'NONE',  ( 3.099999999999945466, 2.500000000000000000, 0.3464101615137735735 ) ) ;
#9867 = ORIENTED_EDGE ( 'NONE', *, *, #3436, .F. ) ;
#9868 = EDGE_LOOP ( 'NONE', ( #10515, #71762 ) ) ;
#9869 = DIRECTION ( 'NONE',  ( 0.000000000000000000, -0.000000000000000000, 1.000000000000000000 ) ) ;
#9870 = ORIENTED_EDGE ( 'NONE', *, *, #92905, .F. ) ;
#9871 = CARTESIAN_POINT ( 'NONE',  ( 104.7003906511443461, 6.718614722302491238, 3.770225884972850494 ) ) ;
#9873 = ORIENTED_EDGE ( 'NONE', *, *, #3292, .T. ) ;
#9872 = EDGE_LOOP ( 'NONE', ( #35421, #4507, #38197, #15860 ) ) ;
#9874 = VERTEX_POINT ( 'NONE', #78955 ) ;
#9875 = VECTOR ( 'NONE', #127392, 1000.000000000000000 ) ;
#9876 = DIRECTION ( 'NONE',  ( 0.000000000000000000, 1.000000000000000000, 0.000000000000000000 ) ) ;
#9877 = PLANE ( 'NONE',  #77838 ) ;
#9878 = DIRECTION ( 'NONE',  ( 0.000000000000000000, -1.846105847067148515E-16, -1.000000000000000000 ) ) ;
#9879 =( NAMED_UNIT ( * ) PLANE_ANGLE_UNIT ( ) SI_UNIT ( $, .RADIAN. ) );
#9880 = DIRECTION ( 'NONE',  ( -0.000000000000000000, 1.000000000000000000, -0.000000000000000000 ) ) ;
#9881 = CARTESIAN_POINT ( 'NONE',  ( 4.799999999999937650, 2.500000000000000000, -4.083716857408426826 ) ) ;
#9882 = DIRECTION ( 'NONE',  ( 0.000000000000000000, 0.000000000000000000, 1.000000000000000000 ) ) ;
#9883 = CARTESIAN_POINT ( 'NONE',  ( 9.999999999999948486, 12.50000000000000000, -4.330127018922201643 ) ) ;
#9884 = DIRECTION ( 'NONE',  ( -0.000000000000000000, 1.000000000000000000, -0.000000000000000000 ) ) ;
#9885 = CARTESIAN_POINT ( 'NONE',  ( 8.949999999999915801, 2.500000000000000000, 6.841600689897072485 ) ) ;
#9886 = ORIENTED_EDGE ( 'NONE', *, *, #77039, .T. ) ;
#9888 = VERTEX_POINT ( 'NONE', #48849 ) ;
#9887 = CIRCLE ( 'NONE', #76786, 0.1000000000000000472 ) ;
#9889 = CONICAL_SURFACE ( 'NONE', #14066, 0.1000000000000002554, 0.003490658503988666988 ) ;
#9890 = FACE_OUTER_BOUND ( 'NONE', #88075, .T. ) ;
#9891 = ORIENTED_EDGE ( 'NONE', *, *, #89462, .T. ) ;
#9892 = ORIENTED_EDGE ( 'NONE', *, *, #749, .F. ) ;
#9893 = LINE ( 'NONE', #61, #77548 ) ;
#9895 = CIRCLE ( 'NONE', #112310, 0.1000000000000000056 ) ;
#9894 = AXIS2_PLACEMENT_3D ( 'NONE', #9629, #89480, #129437 ) ;
#9896 = DIRECTION ( 'NONE',  ( 0.000000000000000000, 1.000000000000000000, 0.000000000000000000 ) ) ;
#9897 = CIRCLE ( 'NONE', #99785, 0.06509327318403745899 ) ;
#9898 = EDGE_CURVE ( 'NONE', #32791, #31641, #69720, .T. ) ;
#9899 = CARTESIAN_POINT ( 'NONE',  ( 12.94999999999990337, 2.500000000000000000, 2.065063509461097624 ) ) ;
#9900 = CARTESIAN_POINT ( 'NONE',  ( -13.34999999999999076, 12.50000000000000000, -2.230156782645137170 ) ) ;
#9901 = LINE ( 'NONE', #717, #101114 ) ;
#9902 = ORIENTED_EDGE ( 'NONE', *, *, #115815, .F. ) ;
#9903 = AXIS2_PLACEMENT_3D ( 'NONE', #111887, #82444, #9815 ) ;
#9904 = EDGE_LOOP ( 'NONE', ( #34686, #50514, #114934, #75756 ) ) ;
#9905 = CARTESIAN_POINT ( 'NONE',  ( 1.049999999999953637, 12.50000000000000000, 2.511473670974873507 ) ) ;
#9906 = CONICAL_SURFACE ( 'NONE', #81009, 0.1000000000000002554, 0.003490658503988666988 ) ;
#9907 = ORIENTED_EDGE ( 'NONE', *, *, #115339, .T. ) ;
#9908 = DIRECTION ( 'NONE',  ( -4.274815082592931898E-19, -0.9999939076577903929, -0.003490651415223739937 ) ) ;
#9909 = ORIENTED_EDGE ( 'NONE', *, *, #9680, .T. ) ;
#9910 = EDGE_CURVE ( 'NONE', #22838, #25337, #19543, .T. ) ;
#9911 = ORIENTED_EDGE ( 'NONE', *, *, #3505, .F. ) ;
#9912 = CARTESIAN_POINT ( 'NONE',  ( -3.750000000000029310, 2.500000000000000000, -7.188010851410854052 ) ) ;
#9913 = FACE_OUTER_BOUND ( 'NONE', #67963, .T. ) ;
#9914 = DIRECTION ( 'NONE',  ( 0.000000000000000000, 0.000000000000000000, -1.000000000000000000 ) ) ;
#9915 = DIRECTION ( 'NONE',  ( -0.000000000000000000, -1.000000000000000000, -0.000000000000000000 ) ) ;
#9916 = AXIS2_PLACEMENT_3D ( 'NONE', #78615, #38022, #77944 ) ;
#9917 = DIRECTION ( 'NONE',  ( -0.000000000000000000, 1.000000000000000000, -0.000000000000000000 ) ) ;
#9918 = ORIENTED_EDGE ( 'NONE', *, *, #107806, .F. ) ;
#9919 = DIRECTION ( 'NONE',  ( -0.000000000000000000, 1.000000000000000000, -0.000000000000000000 ) ) ;
#9920 = PLANE ( 'NONE',  #82889 ) ;
#9921 = CARTESIAN_POINT ( 'NONE',  ( 3.299999999999942979, 12.50000000000000000, 4.395220292106234439 ) ) ;
#9922 = CARTESIAN_POINT ( 'NONE',  ( -12.89999999999999147, 2.500000000000000000, 1.843143693225357538E-15 ) ) ;
#9923 = AXIS2_PLACEMENT_3D ( 'NONE', #44466, #115784, #94213 ) ;
#9924 = AXIS2_PLACEMENT_3D ( 'NONE', #117884, #17749, #97609 ) ;
#9925 = DIRECTION ( 'NONE',  ( 0.000000000000000000, 0.000000000000000000, 1.000000000000000000 ) ) ;
#9926 = VERTEX_POINT ( 'NONE', #98550 ) ;
#9927 = CONICAL_SURFACE ( 'NONE', #20398, 0.1000000000000000056, 0.003490658503988666988 ) ;
#9928 = ORIENTED_EDGE ( 'NONE', *, *, #124499, .T. ) ;
#9929 = DIRECTION ( 'NONE',  ( -0.000000000000000000, -1.000000000000000000, -0.000000000000000000 ) ) ;
#9930 = AXIS2_PLACEMENT_3D ( 'NONE', #2934, #2259, #43512 ) ;
#9931 = EDGE_LOOP ( 'NONE', ( #102016, #31362 ) ) ;
#9932 = AXIS2_PLACEMENT_3D ( 'NONE', #122701, #61861, #103052 ) ;
#9933 = CARTESIAN_POINT ( 'NONE',  ( 17.17279024593006298, -1.352253750625425743, 5.266180533622979887 ) ) ;
#9934 = CARTESIAN_POINT ( 'NONE',  ( 0.3999999999999619971, 2.500000000000000000, -1.084202172485504434E-16 ) ) ;
#9935 = CIRCLE ( 'NONE', #112343, 0.1000000000000002554 ) ;
#9936 = EDGE_CURVE ( 'NONE', #122938, #68683, #69761, .T. ) ;
#9937 = VERTEX_POINT ( 'NONE', #97285 ) ;
#9938 = DIRECTION ( 'NONE',  ( 0.000000000000000000, -0.9999939076577903929, 0.003490651415223739937 ) ) ;
#9940 = CIRCLE ( 'NONE', #16175, 0.06509327318403743123 ) ;
#9939 = DIRECTION ( 'NONE',  ( -0.000000000000000000, 1.000000000000000000, -0.000000000000000000 ) ) ;
#9941 = CARTESIAN_POINT ( 'NONE',  ( -6.850000000000013856, 12.50000000000000000, 2.576566944158910744 ) ) ;
#9942 = DIRECTION ( 'NONE',  ( 0.000000000000000000, 0.000000000000000000, 1.000000000000000000 ) ) ;
#9943 = EDGE_CURVE ( 'NONE', #1764, #33342, #80190, .T. ) ;
#9945 = CIRCLE ( 'NONE', #122817, 0.1000000000000002554 ) ;
#9944 = AXIS2_PLACEMENT_3D ( 'NONE', #25661, #76061, #74135 ) ;
#9946 = LINE ( 'NONE', #40056, #20579 ) ;
#9947 = EDGE_LOOP ( 'NONE', ( #73728, #26402 ) ) ;
#9948 = EDGE_CURVE ( 'NONE', #126006, #36337, #69149, .T. ) ;
#9949 = ADVANCED_FACE ( 'NONE', ( #87453 ), #71221, .T. ) ;
#9950 = EDGE_CURVE ( 'NONE', #120872, #43692, #77632, .T. ) ;
#9952 = ADVANCED_FACE ( 'NONE', ( #59977 ), #64952, .T. ) ;
#9951 = CARTESIAN_POINT ( 'NONE',  ( 21.15177371151417773, 2.593223176056361545, -4.151029080743465549 ) ) ;
#9953 = EDGE_CURVE ( 'NONE', #6356, #47855, #35718, .T. ) ;
#9954 = DIRECTION ( 'NONE',  ( 0.000000000000000000, 1.000000000000000000, 0.000000000000000000 ) ) ;
#9955 = CARTESIAN_POINT ( 'NONE',  ( 2.099999999999949463, 12.50000000000000000, 0.6928203230275494784 ) ) ;
#9956 = ORIENTED_EDGE ( 'NONE', *, *, #118438, .T. ) ;
#9957 = CARTESIAN_POINT ( 'NONE',  ( -4.600000000000024514, 12.50000000000000000, 3.572213422710607489 ) ) ;
#9958 = ORIENTED_EDGE ( 'NONE', *, *, #110883, .F. ) ;
#9959 = DIRECTION ( 'NONE',  ( -0.000000000000000000, 1.000000000000000000, -0.000000000000000000 ) ) ;
#9960 = DIRECTION ( 'NONE',  ( 0.000000000000000000, 1.000000000000000000, 0.000000000000000000 ) ) ;
#9962 = EDGE_CURVE ( 'NONE', #22161, #98907, #81686, .T. ) ;
#9961 = VECTOR ( 'NONE', #16252, 1000.000000000000000 ) ;
#9963 = CARTESIAN_POINT ( 'NONE',  ( -4.076600168545496672E-14, 12.50000000000000000, -5.022947341949754119 ) ) ;
#9964 = ORIENTED_EDGE ( 'NONE', *, *, #98410, .T. ) ;
#9965 = EDGE_CURVE ( 'NONE', #1501, #114265, #108864, .T. ) ;
#9967 = EDGE_CURVE ( 'NONE', #33641, #105724, #52433, .T. ) ;
#9966 = CARTESIAN_POINT ( 'NONE',  ( 3.349999999999943689, 2.500000000000000000, 1.472243186433545459 ) ) ;
#9968 = CARTESIAN_POINT ( 'NONE',  ( 0.8499999999999553468, 2.500000000000000000, 1.572243186433545548 ) ) ;
#9969 = ORIENTED_EDGE ( 'NONE', *, *, #122375, .F. ) ;
#9970 = DIRECTION ( 'NONE',  ( -0.000000000000000000, 1.000000000000000000, -0.000000000000000000 ) ) ;
#9971 = ORIENTED_EDGE ( 'NONE', *, *, #103662, .T. ) ;
#9972 = DIRECTION ( 'NONE',  ( 0.000000000000000000, 0.000000000000000000, 1.000000000000000000 ) ) ;
#9973 = AXIS2_PLACEMENT_3D ( 'NONE', #10044, #117382, #49344 ) ;
#9974 = VECTOR ( 'NONE', #56454, 1000.000000000000000 ) ;
#9975 = ORIENTED_EDGE ( 'NONE', *, *, #115747, .T. ) ;
#9976 = FACE_OUTER_BOUND ( 'NONE', #107554, .T. ) ;
#9977 = LINE ( 'NONE', #19801, #91918 ) ;
#9978 = EDGE_LOOP ( 'NONE', ( #108802, #47738 ) ) ;
#9979 = ORIENTED_EDGE ( 'NONE', *, *, #2687, .T. ) ;
#9980 = CARTESIAN_POINT ( 'NONE',  ( -5.400000000000019895, 2.500000000000000000, 0.09999999999999772959 ) ) ;
#9981 = DIRECTION ( 'NONE',  ( 0.000000000000000000, 1.000000000000000000, 0.000000000000000000 ) ) ;
#9982 = EDGE_LOOP ( 'NONE', ( #37754, #39301, #85937, #82280 ) ) ;
#9983 = CIRCLE ( 'NONE', #79051, 0.06509327318403745899 ) ;
#9984 = CARTESIAN_POINT ( 'NONE',  ( 5.649999999999936406, 12.50000000000000000, -6.148780366869526226 ) ) ;
#9985 = CARTESIAN_POINT ( 'NONE',  ( 187.1093750003414016, 9.264065473108010111E-16, -7.564683531250000925 ) ) ;
#9986 = CONICAL_SURFACE ( 'NONE', #58120, 0.1000000000000000472, 0.003490658503988666988 ) ;
#9987 = CONICAL_SURFACE ( 'NONE', #10274, 0.1000000000000000472, 0.003490658503988666988 ) ;
#9988 = CARTESIAN_POINT ( 'NONE',  ( 129.5000000000000000, 1.500000000000000000, 6.000000000000000000 ) ) ;
#9989 = CARTESIAN_POINT ( 'NONE',  ( 103.1666495638042278, 8.605133039442083742, 1.322232749994941781 ) ) ;
#9990 = LINE ( 'NONE', #19136, #86451 ) ;
#9991 = CARTESIAN_POINT ( 'NONE',  ( 5.399999999999935518, 2.500000000000000000, -4.430127018922202176 ) ) ;
#9992 = CARTESIAN_POINT ( 'NONE',  ( -8.749999999999975131, 12.50000000000000000, -2.165063509461101710 ) ) ;
#9993 = AXIS2_PLACEMENT_3D ( 'NONE', #27528, #67437, #30792 ) ;
#9994 = EDGE_LOOP ( 'NONE', ( #124785, #27878 ) ) ;
#9995 = ORIENTED_EDGE ( 'NONE', *, *, #82182, .F. ) ;
#9996 = VERTEX_POINT ( 'NONE', #58661 ) ;
#9997 = EDGE_LOOP ( 'NONE', ( #24205, #115791 ) ) ;
#9998 = DIRECTION ( 'NONE',  ( 0.000000000000000000, 0.000000000000000000, 1.000000000000000000 ) ) ;
#9999 = DIRECTION ( 'NONE',  ( 0.000000000000000000, 0.000000000000000000, 1.000000000000000000 ) ) ;
#10000 = AXIS2_PLACEMENT_3D ( 'NONE', #48079, #38926, #117417 ) ;
#10001 = CARTESIAN_POINT ( 'NONE',  ( -5.600000000000023626, 2.500000000000000000, -3.983716857408426293 ) ) ;
#10002 = ORIENTED_EDGE ( 'NONE', *, *, #45262, .T. ) ;
#10003 = FACE_BOUND ( 'NONE', #56246, .T. ) ;
#10004 = VERTEX_POINT ( 'NONE', #28556 ) ;
#10005 = ADVANCED_FACE ( 'NONE', ( #68460 ), #88760, .T. ) ;
#10006 = DIRECTION ( 'NONE',  ( 0.000000000000000000, 0.000000000000000000, 1.000000000000000000 ) ) ;
#10007 = CARTESIAN_POINT ( 'NONE',  ( -1.250000000000001110, 2.500000000000000000, -6.595190528383302109 ) ) ;
#10008 = ADVANCED_FACE ( 'NONE', ( #109020 ), #110998, .T. ) ;
#10009 = CARTESIAN_POINT ( 'NONE',  ( 1.649999999999948841, 12.50000000000000000, 6.495190528383297135 ) ) ;
#10010 = CIRCLE ( 'NONE', #30957, 0.06509327318403745899 ) ;
#10011 = FACE_OUTER_BOUND ( 'NONE', #10972, .T. ) ;
#10012 = ADVANCED_FACE ( 'NONE', ( #27248 ), #115104, .T. ) ;
#10013 = CARTESIAN_POINT ( 'NONE',  ( -5.850000000000018296, 2.500000000000000000, 7.188010851410848723 ) ) ;
#10014 = COLOUR_RGB ( '', 0.66274510, 0.83137255, 0.94901961) ;
#10015 = CARTESIAN_POINT ( 'NONE',  ( -7.700000000000016165, 2.500000000000000000, 0.3464101615137735735 ) ) ;
#10016 = DIRECTION ( 'NONE',  ( 0.000000000000000000, 1.000000000000000000, 0.000000000000000000 ) ) ;
#10017 = DIRECTION ( 'NONE',  ( 0.000000000000000000, 1.000000000000000000, 0.000000000000000000 ) ) ;
#10018 = VECTOR ( 'NONE', #49341, 1000.000000000000000 ) ;
#10020 = EDGE_CURVE ( 'NONE', #28942, #124332, #125583, .T. ) ;
#10019 = CARTESIAN_POINT ( 'NONE',  ( -5.850000000000022737, 12.50000000000000000, -6.495190528383302464 ) ) ;
#10021 = ORIENTED_EDGE ( 'NONE', *, *, #98158, .F. ) ;
#10023 = ORIENTED_EDGE ( 'NONE', *, *, #65325, .F. ) ;
#10022 = CONICAL_SURFACE ( 'NONE', #56065, 0.1000000000000002554, 0.003490658503988666988 ) ;
#10024 = EDGE_LOOP ( 'NONE', ( #3052, #91029, #94387, #5564 ) ) ;
#10025 = VERTEX_POINT ( 'NONE', #92625 ) ;
#10026 = DIRECTION ( 'NONE',  ( 0.000000000000000000, 1.000000000000000000, 0.000000000000000000 ) ) ;
#10027 = CARTESIAN_POINT ( 'NONE',  ( 3.549999999999944755, 2.500000000000000000, -6.841600689897077814 ) ) ;
#10029 = ORIENTED_EDGE ( 'NONE', *, *, #45778, .T. ) ;
#10028 = ORIENTED_EDGE ( 'NONE', *, *, #78258, .T. ) ;
#10031 = ORIENTED_EDGE ( 'NONE', *, *, #72682, .T. ) ;
#10030 = VECTOR ( 'NONE', #26438, 1000.000000000000000 ) ;
#10033 = AXIS2_PLACEMENT_3D ( 'NONE', #29182, #29812, #117504 ) ;
#10032 = CARTESIAN_POINT ( 'NONE',  ( 184.5000000000000000, 0.000000000000000000, 0.000000000000000000 ) ) ;
#10034 = AXIS2_PLACEMENT_3D ( 'NONE', #54850, #93506, #34610 ) ;
#10035 = DIRECTION ( 'NONE',  ( -0.000000000000000000, 1.000000000000000000, -0.000000000000000000 ) ) ;
#10036 = CARTESIAN_POINT ( 'NONE',  ( -8.950000000000008171, 12.50000000000000000, 1.818653347947321475 ) ) ;
#10037 = DIRECTION ( 'NONE',  ( 0.000000000000000000, 0.000000000000000000, 1.000000000000000000 ) ) ;
#10038 = CARTESIAN_POINT ( 'NONE',  ( 7.299999999999926104, 2.500000000000000000, 4.676537180435972552 ) ) ;
#10039 = CARTESIAN_POINT ( 'NONE',  ( 162.5000000000000000, 0.5000000000000000000, -7.500000000000005329 ) ) ;
#10040 = DIRECTION ( 'NONE',  ( -4.274815082592931898E-19, -0.9999939076577903929, -0.003490651415223739937 ) ) ;
#10041 = AXIS2_PLACEMENT_3D ( 'NONE', #17421, #57370, #107757 ) ;
#10042 = ADVANCED_FACE ( 'NONE', ( #93272 ), #12711, .T. ) ;
#10043 = EDGE_LOOP ( 'NONE', ( #80725, #110389, #109277, #8163 ) ) ;
#10044 = CARTESIAN_POINT ( 'NONE',  ( 4.799999999999939426, 2.500000000000000000, -4.676537180435977881 ) ) ;
#10045 = VERTEX_POINT ( 'NONE', #112278 ) ;
#10047 = AXIS2_PLACEMENT_3D ( 'NONE', #99861, #98534, #69742 ) ;
#10046 = CIRCLE ( 'NONE', #85254, 0.06509327318403745899 ) ;
#10048 = ORIENTED_EDGE ( 'NONE', *, *, #29335, .F. ) ;
#10049 = EDGE_LOOP ( 'NONE', ( #3958, #78134 ) ) ;
#10050 = LINE ( 'NONE', #110812, #121623 ) ;
#10051 =( BOUNDED_SURFACE ( )  B_SPLINE_SURFACE ( 3, 2, ( 
 ( #128578, #59839, #50625 ),
 ( #120020, #129220, #88621 ),
 ( #9420, #31017, #118073 ),
 ( #108254, #110200, #90547 ) ),
 .UNSPECIFIED., .F., .F., .F. ) 
 B_SPLINE_SURFACE_WITH_KNOTS ( ( 4, 4 ),
 ( 3, 3 ),
 ( 0.02228103309872378826, 0.02393870366795248020 ),
 ( 0.000000000000000000, 1.000000000000000000 ),
 .UNSPECIFIED. ) 
 GEOMETRIC_REPRESENTATION_ITEM ( )  RATIONAL_B_SPLINE_SURFACE ( (
 ( 1.000000000000000000, 0.9066952437723002634, 1.000000000000000000),
 ( 1.000000000000000000, 0.9065452688549063831, 1.000000000000000000),
 ( 1.000000000000000000, 0.9065452844449193304, 1.000000000000000000),
 ( 1.000000000000000000, 0.9066952434955795059, 1.000000000000000000) ) ) 
 REPRESENTATION_ITEM ( '' )  SURFACE ( )  );
#10052 = ORIENTED_EDGE ( 'NONE', *, *, #14633, .F. ) ;
#10053 = ORIENTED_EDGE ( 'NONE', *, *, #44334, .T. ) ;
#10054 = CARTESIAN_POINT ( 'NONE',  ( 9.149999999999916866, 12.50000000000000000, -2.857883832488653741 ) ) ;
#10055 = FACE_OUTER_BOUND ( 'NONE', #79138, .T. ) ;
#10056 = CARTESIAN_POINT ( 'NONE',  ( -10.00000000000000533, 2.500000000000000000, -5.022947341949749678 ) ) ;
#10057 = ADVANCED_FACE ( 'NONE', ( #30508 ), #14753, .T. ) ;
#10058 = DIRECTION ( 'NONE',  ( -0.000000000000000000, 1.000000000000000000, -0.000000000000000000 ) ) ;
#10059 = LINE ( 'NONE', #110195, #83855 ) ;
#10060 = EDGE_LOOP ( 'NONE', ( #72756, #66283, #22042, #43302 ) ) ;
#10061 = LINE ( 'NONE', #18588, #99330 ) ;
#10062 = ORIENTED_EDGE ( 'NONE', *, *, #1024, .T. ) ;
#10063 = PLANE ( 'NONE',  #81785 ) ;
#10064 = EDGE_LOOP ( 'NONE', ( #129156, #35746 ) ) ;
#10065 = CARTESIAN_POINT ( 'NONE',  ( 109.7910216395279122, 7.340097168400048666, 4.671023614519715927 ) ) ;
#10066 = PLANE ( 'NONE',  #90904 ) ;
#10067 = CIRCLE ( 'NONE', #35211, 0.09999999999999982514 ) ;
#10068 = ORIENTED_EDGE ( 'NONE', *, *, #95970, .T. ) ;
#10070 = AXIS2_PLACEMENT_3D ( 'NONE', #32572, #53486, #22104 ) ;
#10069 = DIRECTION ( 'NONE',  ( 0.000000000000000000, -0.000000000000000000, 1.000000000000000000 ) ) ;
#10071 = ADVANCED_FACE ( 'NONE', ( #111621 ), #197, .T. ) ;
#10072 = CARTESIAN_POINT ( 'NONE',  ( 3.349999999999941913, 12.50000000000000000, 5.802370205355744659 ) ) ;
#10073 = VERTEX_POINT ( 'NONE', #22617 ) ;
#10074 = AXIS2_PLACEMENT_3D ( 'NONE', #53094, #21045, #760 ) ;
#10075 = LINE ( 'NONE', #8759, #115562 ) ;
#10076 = ORIENTED_EDGE ( 'NONE', *, *, #81200, .F. ) ;
#10077 = EDGE_LOOP ( 'NONE', ( #84665, #82895 ) ) ;
#10078 = DIRECTION ( 'NONE',  ( 0.000000000000000000, 0.000000000000000000, 1.000000000000000000 ) ) ;
#10079 = DIRECTION ( 'NONE',  ( 0.000000000000000000, 1.000000000000000000, 0.000000000000000000 ) ) ;
#10080 = CARTESIAN_POINT ( 'NONE',  ( 185.0468750003414016, -8.734944146203032389, -1.604583208406768146E-15 ) ) ;
#10081 = LINE ( 'NONE', #50031, #78588 ) ;
#10082 = AXIS2_PLACEMENT_3D ( 'NONE', #89494, #68554, #129450 ) ;
#10083 = CARTESIAN_POINT ( 'NONE',  ( 13.14999999999989733, 2.500000000000000000, -2.511473670974877948 ) ) ;
#10084 = CIRCLE ( 'NONE', #97897, 0.1000000000000002554 ) ;
#10085 = ORIENTED_EDGE ( 'NONE', *, *, #82061, .T. ) ;
#10086 = CARTESIAN_POINT ( 'NONE',  ( 5.649999999999934630, 2.500000000000000000, -2.411473670974877859 ) ) ;
#10087 = ORIENTED_EDGE ( 'NONE', *, *, #26743, .F. ) ;
#10088 = DIRECTION ( 'NONE',  ( 0.000000000000000000, -0.9999939076577903929, 0.003490651415223739937 ) ) ;
#10090 = AXIS2_PLACEMENT_3D ( 'NONE', #18207, #17561, #126892 ) ;
#10089 = CARTESIAN_POINT ( 'NONE',  ( -11.64999999999999680, 2.500000000000000000, 1.372243186433545370 ) ) ;
#10091 = EDGE_CURVE ( 'NONE', #127944, #16485, #43543, .T. ) ;
#10092 = VECTOR ( 'NONE', #17794, 1000.000000000000000 ) ;
#10093 = CARTESIAN_POINT ( 'NONE',  ( 186.6718750003414016, 9.264065473108010111E-16, -7.564683531250000925 ) ) ;
#10094 = PLANE ( 'NONE',  #40583 ) ;
#10095 = CARTESIAN_POINT ( 'NONE',  ( -6.650000000000015454, 2.500000000000000000, 7.288010851410849256 ) ) ;
#10096 = DIRECTION ( 'NONE',  ( 0.000000000000000000, 0.000000000000000000, -1.000000000000000000 ) ) ;
#10097 = CARTESIAN_POINT ( 'NONE',  ( 108.0000000000000142, 8.500000000000000000, 0.000000000000000000 ) ) ;
#10098 = EDGE_LOOP ( 'NONE', ( #101218, #32105 ) ) ;
#10099 = ADVANCED_FACE ( 'NONE', ( #42245 ), #62905, .T. ) ;
#10100 = CIRCLE ( 'NONE', #18499, 0.1000000000000002554 ) ;
#10101 = LINE ( 'NONE', #108924, #56385 ) ;
#10102 = DIRECTION ( 'NONE',  ( 0.000000000000000000, -1.846105847067148022E-16, 1.000000000000000000 ) ) ;
#10103 = DIRECTION ( 'NONE',  ( -0.000000000000000000, 1.000000000000000000, -0.000000000000000000 ) ) ;
#10104 = PRESENTATION_LAYER_ASSIGNMENT (  '', '', ( #66523 ) ) ;
#10105 = ADVANCED_FACE ( 'NONE', ( #51432 ), #75418, .T. ) ;
#10106 = EDGE_CURVE ( 'NONE', #126067, #65404, #87926, .T. ) ;
#10107 = ADVANCED_FACE ( 'NONE', ( #120791 ), #23187, .T. ) ;
#10108 = EDGE_CURVE ( 'NONE', #106239, #27297, #123534, .T. ) ;
#10109 = ORIENTED_EDGE ( 'NONE', *, *, #20277, .T. ) ;
#10110 = AXIS2_PLACEMENT_3D ( 'NONE', #121436, #71701, #40978 ) ;
#10111 = CARTESIAN_POINT ( 'NONE',  ( 2.099999999999950351, 2.500000000000000000, -4.330127018922201643 ) ) ;
#10112 = ORIENTED_EDGE ( 'NONE', *, *, #7997, .T. ) ;
#10113 = VERTEX_POINT ( 'NONE', #110952 ) ;
#10114 = DIRECTION ( 'NONE',  ( 0.000000000000000000, 0.000000000000000000, -1.000000000000000000 ) ) ;
#10115 = EDGE_CURVE ( 'NONE', #68058, #98606, #67073, .T. ) ;
#10116 = EDGE_CURVE ( 'NONE', #83265, #8819, #56620, .T. ) ;
#10117 = EDGE_LOOP ( 'NONE', ( #50682, #117539 ) ) ;
#10118 = CIRCLE ( 'NONE', #1780, 0.06509327318403745899 ) ;
#10119 = CARTESIAN_POINT ( 'NONE',  ( 6.699999999999928235, 2.500000000000000000, 0.09999999999999772959 ) ) ;
#10120 = LINE ( 'NONE', #40223, #13025 ) ;
#10121 = EDGE_CURVE ( 'NONE', #37337, #1478, #54492, .T. ) ;
#10122 = ORIENTED_EDGE ( 'NONE', *, *, #112026, .T. ) ;
#10123 = EDGE_CURVE ( 'NONE', #527, #70003, #48237, .T. ) ;
#10125 = EDGE_CURVE ( 'NONE', #107157, #11464, #52696, .T. ) ;
#10124 = CARTESIAN_POINT ( 'NONE',  ( -7.700000000000010836, 12.50000000000000000, 3.983716857408420964 ) ) ;
#10126 = FACE_OUTER_BOUND ( 'NONE', #66385, .T. ) ;
#10127 = CARTESIAN_POINT ( 'NONE',  ( -5.450000000000023270, 12.50000000000000000, -2.230156782645139391 ) ) ;
#10128 = VECTOR ( 'NONE', #67257, 1000.000000000000000 ) ;
#10129 = EDGE_CURVE ( 'NONE', #99984, #65002, #98399, .T. ) ;
#10130 = ORIENTED_EDGE ( 'NONE', *, *, #71145, .F. ) ;
#10132 = CONICAL_SURFACE ( 'NONE', #45650, 0.1000000000000002554, 0.003490658503988666988 ) ;
#10131 = CIRCLE ( 'NONE', #31001, 0.1000000000000002554 ) ;
#10133 = ORIENTED_EDGE ( 'NONE', *, *, #59203, .F. ) ;
#10134 = ORIENTED_EDGE ( 'NONE', *, *, #66099, .T. ) ;
#10135 = CARTESIAN_POINT ( 'NONE',  ( 5.399999999999933742, 2.500000000000000000, -0.1000000000000023925 ) ) ;
#10136 = CARTESIAN_POINT ( 'NONE',  ( 7.899999999999924860, 2.500000000000000000, 3.637306695894644726 ) ) ;
#10137 = CARTESIAN_POINT ( 'NONE',  ( -3.300000000000027800, 12.50000000000000000, -4.265033745738164406 ) ) ;
#10138 = FACE_BOUND ( 'NONE', #51115, .T. ) ;
#10139 = VERTEX_POINT ( 'NONE', #82163 ) ;
#10140 = DIRECTION ( 'NONE',  ( 0.000000000000000000, 0.000000000000000000, 1.000000000000000000 ) ) ;
#10141 = CARTESIAN_POINT ( 'NONE',  ( 12.89999999999990266, 2.500000000000000000, 3.737306695894644371 ) ) ;
#10142 = ORIENTED_EDGE ( 'NONE', *, *, #117137, .F. ) ;
#10143 = FACE_OUTER_BOUND ( 'NONE', #86244, .T. ) ;
#10144 = DIRECTION ( 'NONE',  ( 0.000000000000000000, 0.000000000000000000, 1.000000000000000000 ) ) ;
#10145 = CARTESIAN_POINT ( 'NONE',  ( -3.350000000000032507, 2.500000000000000000, -6.495190528383302464 ) ) ;
#10146 = DIRECTION ( 'NONE',  ( 0.000000000000000000, -0.9999939076577903929, 0.003490651415223739937 ) ) ;
#10147 = AXIS2_PLACEMENT_3D ( 'NONE', #87874, #78745, #27047 ) ;
#10148 = CARTESIAN_POINT ( 'NONE',  ( -8.150000000000014566, 12.50000000000000000, -6.148780366869520897 ) ) ;
#10149 = CARTESIAN_POINT ( 'NONE',  ( 7.299999999999924327, 12.50000000000000000, 0.4115034346978109769 ) ) ;
#10150 = DIRECTION ( 'NONE',  ( 0.000000000000000000, -0.000000000000000000, 1.000000000000000000 ) ) ;
#10151 = CIRCLE ( 'NONE', #123022, 0.06509327318403745899 ) ;
#10152 = VECTOR ( 'NONE', #103447, 1000.000000000000000 ) ;
#10153 = ORIENTED_EDGE ( 'NONE', *, *, #31291, .T. ) ;
#10154 = ORIENTED_EDGE ( 'NONE', *, *, #67446, .T. ) ;
#10155 = CIRCLE ( 'NONE', #52020, 0.06509327318403745899 ) ;
#10156 = ORIENTED_EDGE ( 'NONE', *, *, #11879, .T. ) ;
#10157 = ORIENTED_EDGE ( 'NONE', *, *, #110114, .T. ) ;
#10158 = CARTESIAN_POINT ( 'NONE',  ( -11.05000000000000249, 12.50000000000000000, -6.213873640053560798 ) ) ;
#10159 = DIRECTION ( 'NONE',  ( -0.000000000000000000, 1.000000000000000000, -0.000000000000000000 ) ) ;
#10160 = ORIENTED_EDGE ( 'NONE', *, *, #73767, .F. ) ;
#10161 = FACE_BOUND ( 'NONE', #92678, .T. ) ;
#10162 = PLANE ( 'NONE',  #68802 ) ;
#10163 = AXIS2_PLACEMENT_3D ( 'NONE', #117876, #56380, #86487 ) ;
#10164 = AXIS2_PLACEMENT_3D ( 'NONE', #45159, #26154, #14374 ) ;
#10165 = EDGE_CURVE ( 'NONE', #106006, #40443, #41982, .T. ) ;
#10166 = AXIS2_PLACEMENT_3D ( 'NONE', #94958, #24918, #95594 ) ;
#10167 = VECTOR ( 'NONE', #120613, 1000.000000000000000 ) ;
#10168 = CARTESIAN_POINT ( 'NONE',  ( 3.349999999999943689, 2.500000000000000000, 1.372243186433545370 ) ) ;
#10169 = ADVANCED_FACE ( 'NONE', ( #122731 ), #2334, .T. ) ;
#10170 = DIRECTION ( 'NONE',  ( 0.000000000000000000, 0.000000000000000000, 1.000000000000000000 ) ) ;
#10171 = CARTESIAN_POINT ( 'NONE',  ( -3.350000000000028955, 12.50000000000000000, 5.802370205355744659 ) ) ;
#10172 = FACE_OUTER_BOUND ( 'NONE', #24662, .T. ) ;
#10173 = DIRECTION ( 'NONE',  ( 0.000000000000000000, -0.9999939076577903929, 0.003490651415223739937 ) ) ;
#10174 = VERTEX_POINT ( 'NONE', #45478 ) ;
#10175 = AXIS2_PLACEMENT_3D ( 'NONE', #52148, #81598, #11564 ) ;
#10176 = ADVANCED_FACE ( 'NONE', ( #83466 ), #74922, .T. ) ;
#10177 = ORIENTED_EDGE ( 'NONE', *, *, #35053, .F. ) ;
#10178 = AXIS2_PLACEMENT_3D ( 'NONE', #66735, #5240, #25514 ) ;
#10179 = ORIENTED_EDGE ( 'NONE', *, *, #60516, .F. ) ;
#10180 = ORIENTED_EDGE ( 'NONE', *, *, #55762, .T. ) ;
#10181 = VERTEX_POINT ( 'NONE', #14683 ) ;
#10182 = VERTEX_POINT ( 'NONE', #53992 ) ;
#10183 = CARTESIAN_POINT ( 'NONE',  ( -0.8500000000000395017, 2.500000000000000000, 6.495190528383297135 ) ) ;
#10184 = DIRECTION ( 'NONE',  ( 0.000000000000000000, 1.000000000000000000, 0.000000000000000000 ) ) ;
#10185 = EDGE_LOOP ( 'NONE', ( #50471, #33302 ) ) ;
#10186 = CARTESIAN_POINT ( 'NONE',  ( -13.74999999999995381, 2.500000000000000000, 2.065063509461101621 ) ) ;
#10187 = CIRCLE ( 'NONE', #47844, 0.1000000000000000472 ) ;
#10188 = CARTESIAN_POINT ( 'NONE',  ( 7.049999999999926992, 12.50000000000000000, 2.099970236277060032 ) ) ;
#10189 = CARTESIAN_POINT ( 'NONE',  ( 185.7343750003414016, 8.734944146203032389, 5.348610694689227483E-16 ) ) ;
#10190 = CARTESIAN_POINT ( 'NONE',  ( 11.44999999999990514, 2.500000000000000000, -6.048780366869526581 ) ) ;
#10191 = FACE_OUTER_BOUND ( 'NONE', #14531, .T. ) ;
#10192 = AXIS2_PLACEMENT_3D ( 'NONE', #109402, #119870, #31496 ) ;
#10193 = ORIENTED_EDGE ( 'NONE', *, *, #50639, .F. ) ;
#10194 = DIRECTION ( 'NONE',  ( 0.000000000000000000, 0.000000000000000000, 1.000000000000000000 ) ) ;
#10195 = ORIENTED_EDGE ( 'NONE', *, *, #89306, .F. ) ;
#10196 = EDGE_LOOP ( 'NONE', ( #18457, #105235 ) ) ;
#10197 = AXIS2_PLACEMENT_3D ( 'NONE', #64765, #124349, #113218 ) ;
#10198 = DIRECTION ( 'NONE',  ( 0.000000000000000000, 1.000000000000000000, 0.000000000000000000 ) ) ;
#10199 = DIRECTION ( 'NONE',  ( 0.000000000000000000, 0.000000000000000000, 1.000000000000000000 ) ) ;
#10200 = CARTESIAN_POINT ( 'NONE',  ( 0.8499999999999553468, 2.500000000000000000, 2.165063509461097713 ) ) ;
#10201 = VERTEX_POINT ( 'NONE', #125306 ) ;
#10202 = AXIS2_PLACEMENT_3D ( 'NONE', #48053, #126614, #76223 ) ;
#10203 = ORIENTED_EDGE ( 'NONE', *, *, #83296, .T. ) ;
#10204 = EDGE_CURVE ( 'NONE', #93739, #121068, #124363, .T. ) ;
#10205 = DIRECTION ( 'NONE',  ( 0.000000000000000000, 1.000000000000000000, 0.000000000000000000 ) ) ;
#10206 = AXIS2_PLACEMENT_3D ( 'NONE', #3978, #83827, #105418 ) ;
#10207 = DIRECTION ( 'NONE',  ( 0.000000000000000000, 0.000000000000000000, -1.000000000000000000 ) ) ;
#10208 = CARTESIAN_POINT ( 'NONE',  ( -10.00000000000000355, 12.50000000000000000, -0.7579135962115916003 ) ) ;
#10209 = CARTESIAN_POINT ( 'NONE',  ( 8.299999999999922551, 2.500000000000000000, -0.1000000000000023925 ) ) ;
#10210 = ORIENTED_EDGE ( 'NONE', *, *, #38957, .T. ) ;
#10211 = LINE ( 'NONE', #72363, #85768 ) ;
#10212 = AXIS2_PLACEMENT_3D ( 'NONE', #25806, #33694, #84071 ) ;
#10213 = VERTEX_POINT ( 'NONE', #85380 ) ;
#10214 = FACE_OUTER_BOUND ( 'NONE', #89986, .T. ) ;
#10215 = ORIENTED_EDGE ( 'NONE', *, *, #12098, .T. ) ;
#10216 = CARTESIAN_POINT ( 'NONE',  ( -9.600000000000008527, 2.500000000000000000, -4.330127018922197202 ) ) ;
#10218 = AXIS2_PLACEMENT_3D ( 'NONE', #60217, #54243, #32696 ) ;
#10217 = AXIS2_PLACEMENT_3D ( 'NONE', #2023, #101529, #32161 ) ;
#10219 = CARTESIAN_POINT ( 'NONE',  ( 15.79999999999989058, 2.500000000000000000, -2.385244779468109755E-15 ) ) ;
#10220 = DIRECTION ( 'NONE',  ( 0.000000000000000000, 1.000000000000000000, 0.000000000000000000 ) ) ;
#10221 = EDGE_CURVE ( 'NONE', #14604, #92039, #67169, .T. ) ;
#10222 = ADVANCED_FACE ( 'NONE', ( #35644 ), #33750, .T. ) ;
#10223 = LINE ( 'NONE', #50159, #114883 ) ;
#10224 = VERTEX_POINT ( 'NONE', #124012 ) ;
#10225 = CARTESIAN_POINT ( 'NONE',  ( 17.49862860983209245, -2.500000000000000000, 4.081131818001135336 ) ) ;
#10227 = CIRCLE ( 'NONE', #1796, 0.06509327318403745899 ) ;
#10226 = VECTOR ( 'NONE', #26008, 1000.000000000000000 ) ;
#10228 = DIRECTION ( 'NONE',  ( -0.000000000000000000, -1.000000000000000000, -0.000000000000000000 ) ) ;
#10229 = ORIENTED_EDGE ( 'NONE', *, *, #164, .T. ) ;
#10230 = EDGE_LOOP ( 'NONE', ( #87209, #36426 ) ) ;
#10232 = ORIENTED_EDGE ( 'NONE', *, *, #5784, .F. ) ;
#10231 = ADVANCED_FACE ( 'NONE', ( #113550 ), #95851, .T. ) ;
#10233 = DIRECTION ( 'NONE',  ( 0.000000000000000000, 0.000000000000000000, -1.000000000000000000 ) ) ;
#10234 = DIRECTION ( 'NONE',  ( 0.000000000000000000, -0.9999939076577903929, 0.003490651415223739937 ) ) ;
#10235 = FACE_OUTER_BOUND ( 'NONE', #72739, .T. ) ;
#10236 = DIRECTION ( 'NONE',  ( 0.000000000000000000, 0.000000000000000000, 1.000000000000000000 ) ) ;
#10237 = CARTESIAN_POINT ( 'NONE',  ( -12.89999999999999147, 2.500000000000000000, -0.7928203230275501223 ) ) ;
#10238 = CARTESIAN_POINT ( 'NONE',  ( -6.650000000000019007, 2.500000000000000000, -5.802370205355749988 ) ) ;
#10239 = DIRECTION ( 'NONE',  ( 0.000000000000000000, 0.000000000000000000, -1.000000000000000000 ) ) ;
#10240 = CARTESIAN_POINT ( 'NONE',  ( -0.6500000000000403233, 2.500000000000000000, 6.248780366869520542 ) ) ;
#10241 = FACE_OUTER_BOUND ( 'NONE', #80105, .T. ) ;
#10242 = AXIS2_PLACEMENT_3D ( 'NONE', #8370, #48309, #28679 ) ;
#10243 = CONICAL_SURFACE ( 'NONE', #93863, 0.1000000000000002554, 0.003490658503988666988 ) ;
#10244 = AXIS2_PLACEMENT_3D ( 'NONE', #79779, #30047, #109892 ) ;
#10245 = VERTEX_POINT ( 'NONE', #116122 ) ;
#10246 = DIRECTION ( 'NONE',  ( 0.000000000000000000, 1.000000000000000000, 0.000000000000000000 ) ) ;
#10247 = DIRECTION ( 'NONE',  ( 0.000000000000000000, -0.9999939076577903929, 0.003490651415223739937 ) ) ;
#10248 = CARTESIAN_POINT ( 'NONE',  ( 12.69999999999989981, 2.500000000000000000, -0.3464101615137783474 ) ) ;
#10249 = DIRECTION ( 'NONE',  ( -0.000000000000000000, 1.000000000000000000, -0.000000000000000000 ) ) ;
#10250 = CARTESIAN_POINT ( 'NONE',  ( 6.849999999999930367, 12.50000000000000000, -6.841600689897078702 ) ) ;
#10251 = VECTOR ( 'NONE', #125345, 1000.000000000000000 ) ;
#10252 = ORIENTED_EDGE ( 'NONE', *, *, #10121, .F. ) ;
#10253 = CIRCLE ( 'NONE', #116842, 0.06509327318403745899 ) ;
#10254 = DIRECTION ( 'NONE',  ( 0.000000000000000000, 1.000000000000000000, 0.000000000000000000 ) ) ;
#10255 = EDGE_CURVE ( 'NONE', #56832, #30668, #65028, .T. ) ;
#10256 = CIRCLE ( 'NONE', #77063, 0.06509327318403745899 ) ;
#10257 = DIRECTION ( 'NONE',  ( 0.000000000000000000, 0.000000000000000000, 1.000000000000000000 ) ) ;
#10259 = EDGE_LOOP ( 'NONE', ( #33853, #41497, #85202, #50407 ) ) ;
#10258 = DIRECTION ( 'NONE',  ( 0.000000000000000000, -0.000000000000000000, 1.000000000000000000 ) ) ;
#10260 = EDGE_CURVE ( 'NONE', #89429, #125138, #34367, .T. ) ;
#10262 = EDGE_CURVE ( 'NONE', #72798, #88688, #79723, .T. ) ;
#10261 = AXIS2_PLACEMENT_3D ( 'NONE', #113479, #13334, #55219 ) ;
#10263 = EDGE_LOOP ( 'NONE', ( #117870, #106023 ) ) ;
#10264 = LINE ( 'NONE', #2344, #86471 ) ;
#10265 = AXIS2_PLACEMENT_3D ( 'NONE', #61456, #71919, #91544 ) ;
#10266 = ORIENTED_EDGE ( 'NONE', *, *, #114870, .F. ) ;
#10267 = ORIENTED_EDGE ( 'NONE', *, *, #48638, .F. ) ;
#10268 = DIRECTION ( 'NONE',  ( 0.000000000000000000, 0.000000000000000000, 1.000000000000000000 ) ) ;
#10269 = EDGE_CURVE ( 'NONE', #13525, #68129, #85961, .T. ) ;
#10270 = EDGE_CURVE ( 'NONE', #60027, #51534, #125932, .T. ) ;
#10271 = ADVANCED_FACE ( 'NONE', ( #85999 ), #44164, .T. ) ;
#10272 = DIRECTION ( 'NONE',  ( 0.000000000000000000, 0.000000000000000000, -1.000000000000000000 ) ) ;
#10273 = DIRECTION ( 'NONE',  ( 0.000000000000000000, 0.000000000000000000, 1.000000000000000000 ) ) ;
#10274 = AXIS2_PLACEMENT_3D ( 'NONE', #78784, #38204, #37564 ) ;
#10275 = ORIENTED_EDGE ( 'NONE', *, *, #80598, .F. ) ;
#10276 = ADVANCED_FACE ( 'NONE', ( #74281 ), #102694, .T. ) ;
#10277 = CARTESIAN_POINT ( 'NONE',  ( 184.7083333333333428, -4.445597072760175017, -7.699999999999898037 ) ) ;
#10278 = ORIENTED_EDGE ( 'NONE', *, *, #25010, .T. ) ;
#10279 = VECTOR ( 'NONE', #38211, 1000.000000000000000 ) ;
#10280 = FACE_OUTER_BOUND ( 'NONE', #58839, .T. ) ;
#10281 = DIRECTION ( 'NONE',  ( 0.000000000000000000, -0.000000000000000000, 1.000000000000000000 ) ) ;
#10282 = DIRECTION ( 'NONE',  ( -0.000000000000000000, -1.000000000000000000, -0.000000000000000000 ) ) ;
#10283 = EDGE_CURVE ( 'NONE', #92342, #26773, #16621, .T. ) ;
#10284 = EDGE_LOOP ( 'NONE', ( #25411, #70188 ) ) ;
#10285 = ORIENTED_EDGE ( 'NONE', *, *, #25745, .F. ) ;
#10286 = EDGE_LOOP ( 'NONE', ( #28362, #66749 ) ) ;
#10287 = EDGE_LOOP ( 'NONE', ( #76051, #104201, #24533, #127231 ) ) ;
#10288 = ORIENTED_EDGE ( 'NONE', *, *, #51644, .F. ) ;
#10289 = DIRECTION ( 'NONE',  ( -0.000000000000000000, 1.000000000000000000, -0.000000000000000000 ) ) ;
#10290 = CARTESIAN_POINT ( 'NONE',  ( 10.89704209861837647, 2.499999999999872990, 8.980393935569876973 ) ) ;
#10291 = DIRECTION ( 'NONE',  ( 0.000000000000000000, -0.9999939076577903929, 0.003490651415223739937 ) ) ;
#10292 = FACE_BOUND ( 'NONE', #8559, .T. ) ;
#10293 = PLANE ( 'NONE',  #30617 ) ;
#10294 = CARTESIAN_POINT ( 'NONE',  ( -9.550000000000002487, 2.500000000000000000, 6.395190528383296602 ) ) ;
#10295 = CIRCLE ( 'NONE', #35433, 0.06509327318403745899 ) ;
#10296 = CARTESIAN_POINT ( 'NONE',  ( -5.600000000000020073, 2.500000000000000000, -0.4464101615137782142 ) ) ;
#10297 = DIRECTION ( 'NONE',  ( 0.000000000000000000, 0.000000000000000000, 1.000000000000000000 ) ) ;
#10298 = AXIS2_PLACEMENT_3D ( 'NONE', #604, #116194, #55357 ) ;
#10299 = DIRECTION ( 'NONE',  ( 0.000000000000000000, -0.9999939076577903929, 0.003490651415223739937 ) ) ;
#10300 = DIRECTION ( 'NONE',  ( 0.000000000000000000, -0.9999939076577903929, 0.003490651415223739937 ) ) ;
#10301 = CIRCLE ( 'NONE', #18700, 0.1000000000000002554 ) ;
#10302 = CARTESIAN_POINT ( 'NONE',  ( -3.100000000000028511, 2.500000000000000000, -0.3464101615137782364 ) ) ;
#10303 = DIRECTION ( 'NONE',  ( 0.000000000000000000, -0.9999939076577903929, 0.003490651415223739937 ) ) ;
#10305 = CONICAL_SURFACE ( 'NONE', #125323, 0.09999999999999999167, 0.003490658503988666988 ) ;
#10304 = VECTOR ( 'NONE', #48241, 1000.000000000000000 ) ;
#10306 = ORIENTED_EDGE ( 'NONE', *, *, #129115, .T. ) ;
#10307 = ORIENTED_EDGE ( 'NONE', *, *, #46934, .F. ) ;
#10308 = VERTEX_POINT ( 'NONE', #14043 ) ;
#10309 = ORIENTED_EDGE ( 'NONE', *, *, #122529, .F. ) ;
#10310 = CARTESIAN_POINT ( 'NONE',  ( -3.350000000000029399, 2.500000000000000000, 6.495190528383297135 ) ) ;
#10311 = DIRECTION ( 'NONE',  ( -4.274815082592931898E-19, -0.9999939076577903929, -0.003490651415223739937 ) ) ;
#10312 = FACE_BOUND ( 'NONE', #115454, .T. ) ;
#10313 = DIRECTION ( 'NONE',  ( 0.000000000000000000, -0.9999939076577903929, 0.003490651415223739937 ) ) ;
#10315 = CIRCLE ( 'NONE', #6086, 0.06509327318403745899 ) ;
#10314 = CIRCLE ( 'NONE', #8153, 0.1000000000000002554 ) ;
#10316 = EDGE_CURVE ( 'NONE', #29957, #82736, #33702, .T. ) ;
#10317 = ORIENTED_EDGE ( 'NONE', *, *, #13465, .T. ) ;
#10318 = DIRECTION ( 'NONE',  ( -0.000000000000000000, -1.000000000000000000, -0.000000000000000000 ) ) ;
#10319 = DIRECTION ( 'NONE',  ( 0.000000000000000000, 1.000000000000000000, 0.000000000000000000 ) ) ;
#10320 = LINE ( 'NONE', #20145, #122079 ) ;
#10321 = CARTESIAN_POINT ( 'NONE',  ( 9.349999999999916156, 2.500000000000000000, 6.741600689897071952 ) ) ;
#10322 = ORIENTED_EDGE ( 'NONE', *, *, #100961, .T. ) ;
#10323 = CARTESIAN_POINT ( 'NONE',  ( 14.34999999999989306, 12.50000000000000000, -2.511473670974877948 ) ) ;
#10324 = EDGE_CURVE ( 'NONE', #31484, #6262, #12799, .T. ) ;
#10325 = ORIENTED_EDGE ( 'NONE', *, *, #42018, .F. ) ;
#10326 = ORIENTED_EDGE ( 'NONE', *, *, #49141, .T. ) ;
#10327 = CONICAL_SURFACE ( 'NONE', #83505, 0.09999999999999982514, 0.003490658503988666988 ) ;
#10328 = CARTESIAN_POINT ( 'NONE',  ( 187.4609375001707008, 0.000000000000000000, 7.632341765625000107 ) ) ;
#10329 = DIRECTION ( 'NONE',  ( 1.000000000000000000, 0.000000000000000000, 0.000000000000000000 ) ) ;
#10330 = ORIENTED_EDGE ( 'NONE', *, *, #64792, .T. ) ;
#10331 = AXIS2_PLACEMENT_3D ( 'NONE', #5089, #103955, #36516 ) ;
#10332 = DIRECTION ( 'NONE',  ( -0.000000000000000000, -1.000000000000000000, -0.000000000000000000 ) ) ;
#10333 = CIRCLE ( 'NONE', #93865, 0.06509327318403745899 ) ;
#10334 = DIRECTION ( 'NONE',  ( -0.000000000000000000, -1.000000000000000000, -0.000000000000000000 ) ) ;
#10335 = DIRECTION ( 'NONE',  ( 0.000000000000000000, 0.000000000000000000, 1.000000000000000000 ) ) ;
#10336 = ORIENTED_EDGE ( 'NONE', *, *, #112879, .F. ) ;
#10337 = LINE ( 'NONE', #41754, #105888 ) ;
#10338 = ORIENTED_EDGE ( 'NONE', *, *, #23260, .F. ) ;
#10339 = FACE_OUTER_BOUND ( 'NONE', #107515, .T. ) ;
#10340 = VECTOR ( 'NONE', #97313, 1000.000000000000000 ) ;
#10341 = VERTEX_POINT ( 'NONE', #97134 ) ;
#10342 = CARTESIAN_POINT ( 'NONE',  ( 110.2489501364907198, 6.266397739826595092, 4.477399565010155236 ) ) ;
#10343 = ORIENTED_EDGE ( 'NONE', *, *, #115651, .T. ) ;
#10344 = DIRECTION ( 'NONE',  ( 0.000000000000000000, 0.000000000000000000, -1.000000000000000000 ) ) ;
#10345 = CARTESIAN_POINT ( 'NONE',  ( -6.850000000000013856, 2.500000000000000000, 2.511473670974873507 ) ) ;
#10346 = DIRECTION ( 'NONE',  ( 0.000000000000000000, -0.000000000000000000, 1.000000000000000000 ) ) ;
#10347 = DIRECTION ( 'NONE',  ( 0.000000000000000000, 0.000000000000000000, 1.000000000000000000 ) ) ;
#10348 = CARTESIAN_POINT ( 'NONE',  ( -10.40000000000000213, 2.500000000000000000, -4.922947341949749145 ) ) ;
#10349 = ORIENTED_EDGE ( 'NONE', *, *, #84997, .F. ) ;
#10350 = ORIENTED_EDGE ( 'NONE', *, *, #97974, .T. ) ;
#10353 = ORIENTED_EDGE ( 'NONE', *, *, #120614, .T. ) ;
#10352 = EDGE_CURVE ( 'NONE', #56130, #93998, #88008, .T. ) ;
#10351 = AXIS2_PLACEMENT_3D ( 'NONE', #30401, #70306, #10703 ) ;
#10354 = DIRECTION ( 'NONE',  ( -0.000000000000000000, -1.000000000000000000, -0.000000000000000000 ) ) ;
#10355 = CIRCLE ( 'NONE', #71001, 0.1000000000000002554 ) ;
#10356 = CARTESIAN_POINT ( 'NONE',  ( 4.349999999999940137, 12.50000000000000000, -2.511473670974877948 ) ) ;
#10357 = CARTESIAN_POINT ( 'NONE',  ( 11.84999999999990727, 12.50000000000000000, 6.841600689897072485 ) ) ;
#10359 = ORIENTED_EDGE ( 'NONE', *, *, #53160, .T. ) ;
#10358 = ORIENTED_EDGE ( 'NONE', *, *, #53673, .F. ) ;
#10360 = ORIENTED_EDGE ( 'NONE', *, *, #114124, .T. ) ;
#10361 = CARTESIAN_POINT ( 'NONE',  ( 8.549999999999924327, 2.500000000000000000, -6.841600689897077814 ) ) ;
#10362 = ORIENTED_EDGE ( 'NONE', *, *, #76940, .F. ) ;
#10364 = EDGE_CURVE ( 'NONE', #109058, #33086, #14934, .T. ) ;
#10363 = CARTESIAN_POINT ( 'NONE',  ( 11.44999999999990870, 12.50000000000000000, -1.883746621131363597 ) ) ;
#10365 = CONTEXT_DEPENDENT_SHAPE_REPRESENTATION ( #63993, #66075 ) ;
#10366 = CARTESIAN_POINT ( 'NONE',  ( 6.649999999999931966, 12.50000000000000000, -5.802370205355749988 ) ) ;
#10367 = CARTESIAN_POINT ( 'NONE',  ( 97.50000000000000000, 0.000000000000000000, 0.000000000000000000 ) ) ;
#10368 = DIRECTION ( 'NONE',  ( -4.274815082592931898E-19, -0.9999939076577903929, -0.003490651415223739937 ) ) ;
#10369 = CARTESIAN_POINT ( 'NONE',  ( -8.950000000000009948, 2.500000000000000000, -1.718653347947326049 ) ) ;
#10370 = AXIS2_PLACEMENT_3D ( 'NONE', #110799, #49978, #89869 ) ;
#10371 = CARTESIAN_POINT ( 'NONE',  ( -8.100000000000010303, 2.500000000000000000, 4.083716857408421497 ) ) ;
#10372 = ADVANCED_FACE ( 'NONE', ( #129209 ), #59158, .T. ) ;
#10373 = EDGE_CURVE ( 'NONE', #3125, #55337, #108241, .T. ) ;
#10374 = CARTESIAN_POINT ( 'NONE',  ( 12.04999999999990479, 2.500000000000000000, 2.265063509461097357 ) ) ;
#10375 = VERTEX_POINT ( 'NONE', #18576 ) ;
#10376 = EDGE_LOOP ( 'NONE', ( #91942, #128514 ) ) ;
#10377 = CARTESIAN_POINT ( 'NONE',  ( 11.04999999999990656, 12.50000000000000000, -6.213873640053564351 ) ) ;
#10378 = ADVANCED_FACE ( 'NONE', ( #118704 ), #42083, .T. ) ;
#10379 = EDGE_LOOP ( 'NONE', ( #94276, #128373, #80964, #94938 ) ) ;
#10380 = EDGE_LOOP ( 'NONE', ( #5509, #123472, #55811, #92993 ) ) ;
#10381 = EDGE_CURVE ( 'NONE', #2782, #17144, #29551, .T. ) ;
#10382 = CARTESIAN_POINT ( 'NONE',  ( 185.2343750003414016, 8.734944146203032389, 5.348610694689227483E-16 ) ) ;
#10383 = FACE_OUTER_BOUND ( 'NONE', #45505, .T. ) ;
#10384 = DIRECTION ( 'NONE',  ( 0.000000000000000000, 0.000000000000000000, 1.000000000000000000 ) ) ;
#10385 = FACE_OUTER_BOUND ( 'NONE', #62794, .T. ) ;
#10386 = CARTESIAN_POINT ( 'NONE',  ( 7.499999999999927169, 2.500000000000000000, -5.022947341949754119 ) ) ;
#10387 = DIRECTION ( 'NONE',  ( -4.274815082592931898E-19, -0.9999939076577903929, -0.003490651415223739937 ) ) ;
#10388 = DIRECTION ( 'NONE',  ( 0.000000000000000000, -0.000000000000000000, 1.000000000000000000 ) ) ;
#10389 = CIRCLE ( 'NONE', #129553, 0.1000000000000002554 ) ;
#10390 = DIRECTION ( 'NONE',  ( 0.000000000000000000, 1.000000000000000000, 0.000000000000000000 ) ) ;
#10391 = VERTEX_POINT ( 'NONE', #49352 ) ;
#10392 = AXIS2_PLACEMENT_3D ( 'NONE', #73034, #5563, #92677 ) ;
#10393 = EDGE_LOOP ( 'NONE', ( #28580, #116103 ) ) ;
#10394 = AXIS2_PLACEMENT_3D ( 'NONE', #126564, #38179, #95805 ) ;
#10395 = VERTEX_POINT ( 'NONE', #97781 ) ;
#10396 = ORIENTED_EDGE ( 'NONE', *, *, #68744, .F. ) ;
#10397 = DIRECTION ( 'NONE',  ( 0.000000000000000000, -0.9999939076577903929, 0.003490651415223739937 ) ) ;
#10398 = CARTESIAN_POINT ( 'NONE',  ( -9.800000000000006040, 12.50000000000000000, -4.676537180435974328 ) ) ;
#10401 = EDGE_LOOP ( 'NONE', ( #106524, #16514 ) ) ;
#10400 = CIRCLE ( 'NONE', #37611, 0.1000000000000002554 ) ;
#10399 = AXIS2_PLACEMENT_3D ( 'NONE', #110218, #9439, #19910 ) ;
#10402 = DIRECTION ( 'NONE',  ( -4.274815082592931898E-19, -0.9999939076577903929, -0.003490651415223739937 ) ) ;
#10403 = EDGE_CURVE ( 'NONE', #99398, #104575, #27465, .T. ) ;
#10404 = CARTESIAN_POINT ( 'NONE',  ( 186.2395833340161175, 4.445597072760147483, 7.699999999999948663 ) ) ;
#10405 = CARTESIAN_POINT ( 'NONE',  ( -4.200000000000029488, 2.500000000000000000, -4.230127018922201998 ) ) ;
#10407 = ORIENTED_EDGE ( 'NONE', *, *, #13081, .T. ) ;
#10406 = DIRECTION ( 'NONE',  ( 0.000000000000000000, 1.000000000000000000, 0.000000000000000000 ) ) ;
#10408 = DIRECTION ( 'NONE',  ( 0.000000000000000000, 0.000000000000000000, -1.000000000000000000 ) ) ;
#10409 = EDGE_CURVE ( 'NONE', #78466, #33313, #16977, .T. ) ;
#10410 = CARTESIAN_POINT ( 'NONE',  ( -3.100000000000028511, 2.500000000000000000, 0.3464101615137736845 ) ) ;
#10411 = ORIENTED_EDGE ( 'NONE', *, *, #1075, .F. ) ;
#10412 = ORIENTED_EDGE ( 'NONE', *, *, #42994, .F. ) ;
#10413 = ORIENTED_EDGE ( 'NONE', *, *, #90137, .T. ) ;
#10414 = ORIENTED_EDGE ( 'NONE', *, *, #14397, .F. ) ;
#10415 = CARTESIAN_POINT ( 'NONE',  ( 12.69999999999989981, 12.50000000000000000, -0.2813168883297409439 ) ) ;
#10416 = EDGE_CURVE ( 'NONE', #2020, #74876, #58799, .T. ) ;
#10417 = ADVANCED_FACE ( 'NONE', ( #27108 ), #47400, .T. ) ;
#10418 = EDGE_CURVE ( 'NONE', #96223, #11828, #119346, .T. ) ;
#10419 = LINE ( 'NONE', #50349, #115697 ) ;
#10420 = CARTESIAN_POINT ( 'NONE',  ( 9.799999999999915445, 2.500000000000000000, 3.983716857408420964 ) ) ;
#10421 = CONICAL_SURFACE ( 'NONE', #117007, 0.1000000000000002554, 0.003490658503988666988 ) ;
#10422 = ADVANCED_FACE ( 'NONE', ( #69601 ), #100634, .T. ) ;
#10423 = DIRECTION ( 'NONE',  ( -4.274815082592931898E-19, -0.9999939076577903929, -0.003490651415223739937 ) ) ;
#10424 = ORIENTED_EDGE ( 'NONE', *, *, #38710, .F. ) ;
#10425 = CARTESIAN_POINT ( 'NONE',  ( -10.85000000000000142, 2.500000000000000000, -2.165063509461097713 ) ) ;
#10426 = DIRECTION ( 'NONE',  ( 0.000000000000000000, -0.000000000000000000, 1.000000000000000000 ) ) ;
#10427 = DIRECTION ( 'NONE',  ( 0.000000000000000000, -0.000000000000000000, 1.000000000000000000 ) ) ;
#10428 = CARTESIAN_POINT ( 'NONE',  ( -10.45000000000000462, 12.50000000000000000, -2.099970236277060476 ) ) ;
#10430 = ADVANCED_FACE ( 'NONE', ( #87936 ), #14849, .T. ) ;
#10429 = CIRCLE ( 'NONE', #77334, 3.500000000000000000 ) ;
#10431 = ORIENTED_EDGE ( 'NONE', *, *, #93477, .T. ) ;
#10432 = EDGE_CURVE ( 'NONE', #26094, #49778, #56711, .T. ) ;
#10433 = CARTESIAN_POINT ( 'NONE',  ( 11.24999999999990585, 12.50000000000000000, 2.857883832488649301 ) ) ;
#10434 = ORIENTED_EDGE ( 'NONE', *, *, #125767, .F. ) ;
#10435 = ORIENTED_EDGE ( 'NONE', *, *, #88989, .T. ) ;
#10436 = DIRECTION ( 'NONE',  ( 0.000000000000000000, 1.000000000000000000, 0.000000000000000000 ) ) ;
#10437 = CARTESIAN_POINT ( 'NONE',  ( 2.099999999999947686, 2.500000000000000000, 4.922947341949748257 ) ) ;
#10438 = FACE_BOUND ( 'NONE', #97319, .T. ) ;
#10439 = AXIS2_PLACEMENT_3D ( 'NONE', #63271, #42355, #31888 ) ;
#10440 = PLANE ( 'NONE',  #57609 ) ;
#10441 = CARTESIAN_POINT ( 'NONE',  ( 8.149999999999920419, 2.500000000000000000, -1.818653347947325916 ) ) ;
#10442 = DIRECTION ( 'NONE',  ( 0.000000000000000000, 0.000000000000000000, 1.000000000000000000 ) ) ;
#10443 = CONICAL_SURFACE ( 'NONE', #123310, 0.09999999999999982514, 0.003490658503988666988 ) ;
#10444 = CIRCLE ( 'NONE', #2122, 0.1000000000000000472 ) ;
#10445 = DIRECTION ( 'NONE',  ( 0.000000000000000000, 1.000000000000000000, 0.000000000000000000 ) ) ;
#10446 = CARTESIAN_POINT ( 'NONE',  ( -12.89999999999999147, 2.500000000000000000, 5.022947341949748790 ) ) ;
#10447 = DIRECTION ( 'NONE',  ( 0.000000000000000000, 0.000000000000000000, 1.000000000000000000 ) ) ;
#10448 = CARTESIAN_POINT ( 'NONE',  ( -11.64999999999999680, 2.500000000000000000, 7.188010851410848723 ) ) ;
#10449 = ORIENTED_EDGE ( 'NONE', *, *, #78188, .F. ) ;
#10450 = CONICAL_SURFACE ( 'NONE', #33457, 0.1000000000000002554, 0.003490658503988666988 ) ;
#10451 = DIRECTION ( 'NONE',  ( 0.000000000000000000, 0.000000000000000000, 1.000000000000000000 ) ) ;
#10452 = DIRECTION ( 'NONE',  ( 0.000000000000000000, -0.9999939076577903929, 0.003490651415223739937 ) ) ;
#10453 = CIRCLE ( 'NONE', #35602, 0.09999999999999982514 ) ;
#10454 = ORIENTED_EDGE ( 'NONE', *, *, #28755, .T. ) ;
#10455 = ORIENTED_EDGE ( 'NONE', *, *, #64339, .F. ) ;
#10456 = DIRECTION ( 'NONE',  ( 0.000000000000000000, -1.000000000000000000, 0.000000000000000000 ) ) ;
#10457 = CARTESIAN_POINT ( 'NONE',  ( -11.24999999999996270, 12.50000000000000000, 6.495190528383297135 ) ) ;
#10458 = FACE_BOUND ( 'NONE', #81099, .T. ) ;
#10459 = CARTESIAN_POINT ( 'NONE',  ( 2.699999999999944666, 2.500000000000000000, 4.576537180435972019 ) ) ;
#10460 = DIRECTION ( 'NONE',  ( -0.000000000000000000, -1.000000000000000000, -0.000000000000000000 ) ) ;
#10461 = ADVANCED_FACE ( 'NONE', ( #128562 ), #81766, .T. ) ;
#10462 = ORIENTED_EDGE ( 'NONE', *, *, #112154, .F. ) ;
#10463 = DIRECTION ( 'NONE',  ( 0.000000000000000000, 1.000000000000000000, 0.000000000000000000 ) ) ;
#10464 = DIRECTION ( 'NONE',  ( 0.000000000000000000, 0.000000000000000000, -1.000000000000000000 ) ) ;
#10465 = ORIENTED_EDGE ( 'NONE', *, *, #101781, .T. ) ;
#10466 = CARTESIAN_POINT ( 'NONE',  ( -12.49999999999999467, 2.500000000000000000, 0.5928203230275536084 ) ) ;
#10467 = DIRECTION ( 'NONE',  ( 0.000000000000000000, 0.000000000000000000, 1.000000000000000000 ) ) ;
#10468 = EDGE_CURVE ( 'NONE', #60755, #88674, #106938, .T. ) ;
#10469 = CARTESIAN_POINT ( 'NONE',  ( 12.49999999999990585, 12.50000000000000000, 3.702399969078682407 ) ) ;
#10470 = CARTESIAN_POINT ( 'NONE',  ( 2.049999999999950084, 2.500000000000000000, 2.165063509461097713 ) ) ;
#10471 = VERTEX_POINT ( 'NONE', #28405 ) ;
#10472 = DIRECTION ( 'NONE',  ( -0.000000000000000000, 1.000000000000000000, -0.000000000000000000 ) ) ;
#10474 = CIRCLE ( 'NONE', #123359, 0.06509327318403745899 ) ;
#10473 = AXIS2_PLACEMENT_3D ( 'NONE', #91236, #30408, #41516 ) ;
#10475 = DIRECTION ( 'NONE',  ( 0.000000000000000000, 1.000000000000000000, 0.000000000000000000 ) ) ;
#10476 = DIRECTION ( 'NONE',  ( 0.000000000000000000, -0.000000000000000000, 1.000000000000000000 ) ) ;
#10477 = CARTESIAN_POINT ( 'NONE',  ( 1.249999999999988454, 2.500000000000000000, -2.165063509461101710 ) ) ;
#10478 = ORIENTED_EDGE ( 'NONE', *, *, #61124, .T. ) ;
#10479 = EDGE_LOOP ( 'NONE', ( #38773, #96171, #50215, #74747 ) ) ;
#10480 = CARTESIAN_POINT ( 'NONE',  ( -8.750000000000008882, 12.50000000000000000, -2.857883832488653741 ) ) ;
#10481 = ORIENTED_EDGE ( 'NONE', *, *, #110242, .T. ) ;
#10482 = DIRECTION ( 'NONE',  ( 0.000000000000000000, 1.000000000000000000, 0.000000000000000000 ) ) ;
#10484 = DIRECTION ( 'NONE',  ( 0.000000000000000000, 0.000000000000000000, 1.000000000000000000 ) ) ;
#10483 = AXIS2_PLACEMENT_3D ( 'NONE', #47929, #28280, #96351 ) ;
#10485 = CARTESIAN_POINT ( 'NONE',  ( 10.84999999999990905, 12.50000000000000000, 1.537336459617582918 ) ) ;
#10486 = EDGE_LOOP ( 'NONE', ( #93915, #95916, #77096, #37661 ) ) ;
#10487 = DIRECTION ( 'NONE',  ( 0.000000000000000000, 1.000000000000000000, 0.000000000000000000 ) ) ;
#10488 = CARTESIAN_POINT ( 'NONE',  ( -5.450000000000023270, 2.500000000000000000, -6.495190528383302464 ) ) ;
#10489 = DIRECTION ( 'NONE',  ( 0.000000000000000000, 0.000000000000000000, 1.000000000000000000 ) ) ;
#10490 = DIRECTION ( 'NONE',  ( 0.000000000000000000, -0.000000000000000000, 1.000000000000000000 ) ) ;
#10491 = DIRECTION ( 'NONE',  ( 0.000000000000000000, 1.000000000000000000, 0.000000000000000000 ) ) ;
#10492 = DIRECTION ( 'NONE',  ( 0.000000000000000000, 0.000000000000000000, 1.000000000000000000 ) ) ;
#10493 = ORIENTED_EDGE ( 'NONE', *, *, #124185, .F. ) ;
#10494 = ORIENTED_EDGE ( 'NONE', *, *, #83444, .F. ) ;
#10495 = DIRECTION ( 'NONE',  ( 0.000000000000000000, 1.000000000000000000, 0.000000000000000000 ) ) ;
#10496 = VERTEX_POINT ( 'NONE', #32935 ) ;
#10497 = CARTESIAN_POINT ( 'NONE',  ( 2.099999999999950351, 2.500000000000000000, -4.330127018922201643 ) ) ;
#10499 = ORIENTED_EDGE ( 'NONE', *, *, #31682, .T. ) ;
#10498 = ORIENTED_EDGE ( 'NONE', *, *, #60829, .T. ) ;
#10500 = VERTEX_POINT ( 'NONE', #49995 ) ;
#10501 = CARTESIAN_POINT ( 'NONE',  ( 17.50000000000000000, 0.8333333333333378112, -3.999999999999996447 ) ) ;
#10502 = AXIS2_PLACEMENT_3D ( 'NONE', #30181, #121756, #62218 ) ;
#10504 = EDGE_CURVE ( 'NONE', #50078, #120592, #73454, .T. ) ;
#10503 = DIRECTION ( 'NONE',  ( 0.000000000000000000, 1.000000000000000000, 0.000000000000000000 ) ) ;
#10505 = PLANE ( 'NONE',  #83096 ) ;
#10506 = DIRECTION ( 'NONE',  ( 0.000000000000000000, 1.000000000000000000, 0.000000000000000000 ) ) ;
#10507 = CARTESIAN_POINT ( 'NONE',  ( 9.599999999999917932, 12.50000000000000000, -2.276824562219559311E-15 ) ) ;
#10508 = CARTESIAN_POINT ( 'NONE',  ( 6.249999999999934275, 12.50000000000000000, -7.122917578226816815 ) ) ;
#10509 = DIRECTION ( 'NONE',  ( -4.274815082592931898E-19, -0.9999939076577903929, -0.003490651415223739937 ) ) ;
#10510 = DIRECTION ( 'NONE',  ( -0.000000000000000000, 1.000000000000000000, -0.000000000000000000 ) ) ;
#10511 = ADVANCED_FACE ( 'NONE', ( #870 ), #117336, .T. ) ;
#10512 = EDGE_CURVE ( 'NONE', #38024, #5090, #44205, .T. ) ;
#10514 = VECTOR ( 'NONE', #43776, 1000.000000000000000 ) ;
#10513 = CARTESIAN_POINT ( 'NONE',  ( -1.050000000000037348, 12.50000000000000000, -2.511473670974877948 ) ) ;
#10515 = ORIENTED_EDGE ( 'NONE', *, *, #107886, .F. ) ;
#10516 = EDGE_CURVE ( 'NONE', #12146, #51476, #48328, .T. ) ;
#10518 = EDGE_CURVE ( 'NONE', #123828, #126113, #72838, .T. ) ;
#10517 = CARTESIAN_POINT ( 'NONE',  ( 10.39999999999991509, 12.50000000000000000, 0.6277270498435120194 ) ) ;
#10519 = EDGE_LOOP ( 'NONE', ( #14019, #2750, #22603, #90684 ) ) ;
#10520 = ORIENTED_EDGE ( 'NONE', *, *, #58411, .T. ) ;
#10521 = ADVANCED_FACE ( 'NONE', ( #32293 ), #35953, .T. ) ;
#10522 = DIRECTION ( 'NONE',  ( 0.000000000000000000, 0.000000000000000000, 1.000000000000000000 ) ) ;
#10523 = CARTESIAN_POINT ( 'NONE',  ( -12.09999999999999609, 12.50000000000000000, 4.395220292106234439 ) ) ;
#10524 = VECTOR ( 'NONE', #43921, 1000.000000000000000 ) ;
#10525 = DIRECTION ( 'NONE',  ( -0.000000000000000000, 1.000000000000000000, -0.000000000000000000 ) ) ;
#10526 = AXIS2_PLACEMENT_3D ( 'NONE', #68553, #88844, #109108 ) ;
#10527 = DIRECTION ( 'NONE',  ( 0.000000000000000000, 0.000000000000000000, 1.000000000000000000 ) ) ;
#10528 = DIRECTION ( 'NONE',  ( 0.000000000000000000, 0.000000000000000000, -1.000000000000000000 ) ) ;
#10529 = DIRECTION ( 'NONE',  ( 0.000000000000000000, 1.000000000000000000, 0.000000000000000000 ) ) ;
#10530 = ORIENTED_EDGE ( 'NONE', *, *, #38710, .T. ) ;
#10531 = CONICAL_SURFACE ( 'NONE', #69024, 0.09999999999999999167, 0.003490658503988666988 ) ;
#10532 = EDGE_LOOP ( 'NONE', ( #41848, #38167, #63814, #124519 ) ) ;
#10533 = FACE_OUTER_BOUND ( 'NONE', #26316, .T. ) ;
#10534 = VERTEX_POINT ( 'NONE', #70259 ) ;
#10535 = DIRECTION ( 'NONE',  ( -0.000000000000000000, -1.000000000000000000, -0.000000000000000000 ) ) ;
#10536 = CIRCLE ( 'NONE', #156, 0.1000000000000000472 ) ;
#10537 = ORIENTED_EDGE ( 'NONE', *, *, #36366, .F. ) ;
#10538 = ORIENTED_EDGE ( 'NONE', *, *, #25647, .F. ) ;
#10539 = CARTESIAN_POINT ( 'NONE',  ( 6.699999999999930012, 2.500000000000000000, 4.330127018922196314 ) ) ;
#10540 = DIRECTION ( 'NONE',  ( -0.000000000000000000, -1.000000000000000000, -0.000000000000000000 ) ) ;
#10541 = DIRECTION ( 'NONE',  ( 0.000000000000000000, 0.000000000000000000, -1.000000000000000000 ) ) ;
#10542 = PLANE ( 'NONE',  #96680 ) ;
#10543 = DIRECTION ( 'NONE',  ( 0.000000000000000000, 0.000000000000000000, -1.000000000000000000 ) ) ;
#10544 = ORIENTED_EDGE ( 'NONE', *, *, #5060, .F. ) ;
#10545 = CARTESIAN_POINT ( 'NONE',  ( 13.14999999999990088, 2.500000000000000000, 2.411473670974873862 ) ) ;
#10546 = DIRECTION ( 'NONE',  ( 0.000000000000000000, 1.000000000000000000, 0.000000000000000000 ) ) ;
#10547 = FACE_OUTER_BOUND ( 'NONE', #45300, .T. ) ;
#10548 = CARTESIAN_POINT ( 'NONE',  ( -12.94999999999999218, 12.50000000000000000, 2.165063509461101265 ) ) ;
#10549 = DIRECTION ( 'NONE',  ( 0.000000000000000000, 1.000000000000000000, 0.000000000000000000 ) ) ;
#10550 = VERTEX_POINT ( 'NONE', #23089 ) ;
#10551 = EDGE_LOOP ( 'NONE', ( #100498, #23386 ) ) ;
#10553 = EDGE_CURVE ( 'NONE', #128041, #16283, #63010, .T. ) ;
#10552 = AXIS2_PLACEMENT_3D ( 'NONE', #67834, #18085, #58032 ) ;
#10554 = DIRECTION ( 'NONE',  ( -0.000000000000000000, 1.000000000000000000, -0.000000000000000000 ) ) ;
#10555 = ADVANCED_FACE ( 'NONE', ( #12605 ), #71535, .T. ) ;
#10556 = AXIS2_PLACEMENT_3D ( 'NONE', #82337, #101966, #53517 ) ;
#10557 = EDGE_CURVE ( 'NONE', #82548, #37370, #10050, .T. ) ;
#10558 = EDGE_LOOP ( 'NONE', ( #44370, #73680 ) ) ;
#10559 = DIRECTION ( 'NONE',  ( -4.274815082592931898E-19, -0.9999939076577903929, -0.003490651415223739937 ) ) ;
#10560 = DIRECTION ( 'NONE',  ( 0.000000000000000000, 0.000000000000000000, -1.000000000000000000 ) ) ;
#10561 = EDGE_CURVE ( 'NONE', #115875, #14684, #72202, .T. ) ;
#10562 = ADVANCED_FACE ( 'NONE', ( #22466 ), #73594, .T. ) ;
#10563 = VERTEX_POINT ( 'NONE', #61745 ) ;
#10564 = CARTESIAN_POINT ( 'NONE',  ( 10.19999999999991225, 2.500000000000000000, -4.676537180435978769 ) ) ;
#10565 = LINE ( 'NONE', #22358, #49568 ) ;
#10566 = FACE_OUTER_BOUND ( 'NONE', #35032, .T. ) ;
#10567 = CARTESIAN_POINT ( 'NONE',  ( -14.34999999999998543, 2.500000000000000000, -2.611473670974875372 ) ) ;
#10568 = EDGE_CURVE ( 'NONE', #72837, #121539, #100366, .T. ) ;
#10569 = ADVANCED_FACE ( 'NONE', ( #51916 ), #125819, .T. ) ;
#10570 = DIRECTION ( 'NONE',  ( 0.000000000000000000, 0.000000000000000000, 1.000000000000000000 ) ) ;
#10571 = VERTEX_POINT ( 'NONE', #120642 ) ;
#10572 = CARTESIAN_POINT ( 'NONE',  ( 48.83464596124490953, 3.619824809942020050, -4.313880784154338954 ) ) ;
#10573 = DIRECTION ( 'NONE',  ( 0.000000000000000000, 0.000000000000000000, 1.000000000000000000 ) ) ;
#10574 = EDGE_CURVE ( 'NONE', #90660, #15503, #31005, .T. ) ;
#10575 = DIRECTION ( 'NONE',  ( 0.000000000000000000, -0.9999939076577903929, 0.003490651415223739937 ) ) ;
#10576 = DIRECTION ( 'NONE',  ( 0.000000000000000000, 0.000000000000000000, -1.000000000000000000 ) ) ;
#10577 = VERTEX_POINT ( 'NONE', #21146 ) ;
#10578 = ORIENTED_EDGE ( 'NONE', *, *, #37774, .F. ) ;
#10579 = LINE ( 'NONE', #80644, #79422 ) ;
#10580 = CARTESIAN_POINT ( 'NONE',  ( -12.89999999999999147, 2.500000000000000000, 4.330127018922196314 ) ) ;
#10581 = DIRECTION ( 'NONE',  ( 0.000000000000000000, 1.000000000000000000, 0.000000000000000000 ) ) ;
#10582 = VERTEX_POINT ( 'NONE', #61076 ) ;
#10583 = VECTOR ( 'NONE', #60940, 1000.000000000000000 ) ;
#10584 = FACE_OUTER_BOUND ( 'NONE', #111600, .T. ) ;
#10585 = AXIS2_PLACEMENT_3D ( 'NONE', #59504, #79752, #79125 ) ;
#10586 = CARTESIAN_POINT ( 'NONE',  ( -7.100000000000017408, 12.50000000000000000, 0.6928203230275494784 ) ) ;
#10587 = EDGE_LOOP ( 'NONE', ( #57060, #77842, #67948, #47811 ) ) ;
#10588 = DIRECTION ( 'NONE',  ( 0.000000000000000000, 1.000000000000000000, 0.000000000000000000 ) ) ;
#10589 = ORIENTED_EDGE ( 'NONE', *, *, #26245, .F. ) ;
#10590 = CONICAL_SURFACE ( 'NONE', #31549, 0.09999999999999982514, 0.003490658503988666988 ) ;
#10591 = CARTESIAN_POINT ( 'NONE',  ( 1.649999999999949729, 12.50000000000000000, 7.122917578226811486 ) ) ;
#10592 = EDGE_LOOP ( 'NONE', ( #28315, #82445 ) ) ;
#10593 = DIRECTION ( 'NONE',  ( 0.000000000000000000, 0.000000000000000000, -1.000000000000000000 ) ) ;
#10594 = CARTESIAN_POINT ( 'NONE',  ( 15.40649769635636979, 2.500000000000000444, -5.817321165395405558 ) ) ;
#10595 = EDGE_LOOP ( 'NONE', ( #82146, #93912, #35349, #126249 ) ) ;
#10596 = VERTEX_POINT ( 'NONE', #11335 ) ;
#10597 = CARTESIAN_POINT ( 'NONE',  ( 5.599999999999934808, 2.500000000000000000, -4.083716857408426826 ) ) ;
#10598 = CARTESIAN_POINT ( 'NONE',  ( 5.199999999999935341, 2.500000000000000000, -3.983716857408426293 ) ) ;
#10599 = ORIENTED_EDGE ( 'NONE', *, *, #116495, .F. ) ;
#10600 = DIRECTION ( 'NONE',  ( 0.000000000000000000, 1.000000000000000000, 0.000000000000000000 ) ) ;
#10601 = DIRECTION ( 'NONE',  ( 0.000000000000000000, 1.000000000000000000, 0.000000000000000000 ) ) ;
#10602 = AXIS2_PLACEMENT_3D ( 'NONE', #65815, #94629, #14136 ) ;
#10603 = EDGE_CURVE ( 'NONE', #94142, #57508, #45992, .T. ) ;
#10604 = CARTESIAN_POINT ( 'NONE',  ( 12.89999999999989910, 12.50000000000000000, 0.6277270498435120194 ) ) ;
#10605 = CARTESIAN_POINT ( 'NONE',  ( 4.999999999999936939, 12.50000000000000000, -3.637306695894650055 ) ) ;
#10606 = DIRECTION ( 'NONE',  ( 0.000000000000000000, 0.000000000000000000, 1.000000000000000000 ) ) ;
#10607 = DIRECTION ( 'NONE',  ( 0.000000000000000000, 0.000000000000000000, 1.000000000000000000 ) ) ;
#10608 = CARTESIAN_POINT ( 'NONE',  ( -4.150000000000025224, 2.500000000000000000, 7.188010851410848723 ) ) ;
#10609 = VERTEX_POINT ( 'NONE', #74769 ) ;
#10610 = ORIENTED_EDGE ( 'NONE', *, *, #14501, .T. ) ;
#10611 = ORIENTED_EDGE ( 'NONE', *, *, #23625, .T. ) ;
#10612 = CONICAL_SURFACE ( 'NONE', #42042, 0.1000000000000000472, 0.003490658503988666988 ) ;
#10613 = DIRECTION ( 'NONE',  ( -0.000000000000000000, 1.000000000000000000, -0.000000000000000000 ) ) ;
#10614 = DIRECTION ( 'NONE',  ( -0.000000000000000000, -1.000000000000000000, -0.000000000000000000 ) ) ;
#10615 = DIRECTION ( 'NONE',  ( 0.000000000000000000, 0.000000000000000000, -1.000000000000000000 ) ) ;
#10617 = ORIENTED_EDGE ( 'NONE', *, *, #24648, .T. ) ;
#10616 = ORIENTED_EDGE ( 'NONE', *, *, #71564, .F. ) ;
#10618 = FACE_BOUND ( 'NONE', #33593, .T. ) ;
#10619 = ORIENTED_EDGE ( 'NONE', *, *, #53836, .T. ) ;
#10620 = DIRECTION ( 'NONE',  ( 0.000000000000000000, 0.000000000000000000, 1.000000000000000000 ) ) ;
#10621 = DIRECTION ( 'NONE',  ( -0.000000000000000000, 1.000000000000000000, -0.000000000000000000 ) ) ;
#10622 = CARTESIAN_POINT ( 'NONE',  ( -12.49999999999999467, 12.50000000000000000, -3.637306695894647390 ) ) ;
#10623 = DIRECTION ( 'NONE',  ( 0.000000000000000000, -0.9999939076577903929, 0.003490651415223739937 ) ) ;
#10624 = DIRECTION ( 'NONE',  ( -0.000000000000000000, -1.000000000000000000, -0.000000000000000000 ) ) ;
#10625 = DIRECTION ( 'NONE',  ( 0.000000000000000000, 0.000000000000000000, -1.000000000000000000 ) ) ;
#10626 = CARTESIAN_POINT ( 'NONE',  ( 8.149999999999923972, 12.50000000000000000, 1.818653347947321475 ) ) ;
#10627 = DIRECTION ( 'NONE',  ( 0.000000000000000000, 0.000000000000000000, 1.000000000000000000 ) ) ;
#10628 = DIRECTION ( 'NONE',  ( 0.000000000000000000, -0.000000000000000000, 1.000000000000000000 ) ) ;
#10629 = LINE ( 'NONE', #80703, #15938 ) ;
#10630 = ORIENTED_EDGE ( 'NONE', *, *, #59727, .T. ) ;
#10631 = VERTEX_POINT ( 'NONE', #25020 ) ;
#10632 = VERTEX_POINT ( 'NONE', #55761 ) ;
#10633 = ORIENTED_EDGE ( 'NONE', *, *, #25517, .T. ) ;
#10634 = FACE_OUTER_BOUND ( 'NONE', #126451, .T. ) ;
#10635 = LINE ( 'NONE', #51896, #117616 ) ;
#10636 = CIRCLE ( 'NONE', #121466, 0.06509327318403743123 ) ;
#10638 = ORIENTED_EDGE ( 'NONE', *, *, #128169, .T. ) ;
#10637 = EDGE_LOOP ( 'NONE', ( #33843, #96447 ) ) ;
#10639 = VERTEX_POINT ( 'NONE', #6007 ) ;
#10640 = LINE ( 'NONE', #49336, #37574 ) ;
#10641 = EDGE_CURVE ( 'NONE', #1523, #54360, #115344, .T. ) ;
#10642 = AXIS2_PLACEMENT_3D ( 'NONE', #43927, #83824, #13140 ) ;
#10643 = FACE_OUTER_BOUND ( 'NONE', #14836, .T. ) ;
#10644 = CARTESIAN_POINT ( 'NONE',  ( 0.000000000000000000, 0.000000000000000000, 0.000000000000000000 ) ) ;
#10645 = CARTESIAN_POINT ( 'NONE',  ( -3.750000000000031086, 2.500000000000000000, -5.802370205355749988 ) ) ;
#10646 = CARTESIAN_POINT ( 'NONE',  ( 3.149999999999946176, 2.500000000000000000, -6.741600689897077281 ) ) ;
#10647 = CARTESIAN_POINT ( 'NONE',  ( 2.500000000000002220, 2.500000000000000000, 9.261799387799150907 ) ) ;
#10648 = AXIS2_PLACEMENT_3D ( 'NONE', #99878, #18726, #8892 ) ;
#10649 = CARTESIAN_POINT ( 'NONE',  ( 11.69999999999990870, 12.50000000000000000, 4.395220292106234439 ) ) ;
#10650 = EDGE_CURVE ( 'NONE', #70505, #39225, #104890, .T. ) ;
#10651 = VERTEX_POINT ( 'NONE', #36136 ) ;
#10652 = ADVANCED_FACE ( 'NONE', ( #13245 ), #17130, .T. ) ;
#10653 = CARTESIAN_POINT ( 'NONE',  ( -5.200000000000022382, 2.500000000000000000, 0.2464101615137735679 ) ) ;
#10654 = VERTEX_POINT ( 'NONE', #105519 ) ;
#10655 = ORIENTED_EDGE ( 'NONE', *, *, #53564, .F. ) ;
#10656 = ORIENTED_EDGE ( 'NONE', *, *, #82969, .F. ) ;
#10657 = EDGE_CURVE ( 'NONE', #122805, #39278, #38003, .T. ) ;
#10659 = EDGE_CURVE ( 'NONE', #74338, #54151, #45318, .T. ) ;
#10658 = DIRECTION ( 'NONE',  ( 0.000000000000000000, 0.000000000000000000, -1.000000000000000000 ) ) ;
#10661 = EDGE_LOOP ( 'NONE', ( #60121, #21797 ) ) ;
#10660 = EDGE_CURVE ( 'NONE', #108138, #24484, #26320, .T. ) ;
#10662 = EDGE_CURVE ( 'NONE', #70366, #72904, #123756, .T. ) ;
#10664 = ORIENTED_EDGE ( 'NONE', *, *, #48165, .F. ) ;
#10663 = EDGE_CURVE ( 'NONE', #114904, #35443, #75642, .T. ) ;
#10665 = DIRECTION ( 'NONE',  ( 0.000000000000000000, 0.000000000000000000, -1.000000000000000000 ) ) ;
#10666 = AXIS2_PLACEMENT_3D ( 'NONE', #58179, #68613, #117052 ) ;
#10667 = CARTESIAN_POINT ( 'NONE',  ( -3.350000000000031619, 2.500000000000000000, -7.088010851410853519 ) ) ;
#10668 = CARTESIAN_POINT ( 'NONE',  ( -10.80000000000000071, 12.50000000000000000, 0.06509327318403515528 ) ) ;
#10669 = LINE ( 'NONE', #1511, #123611 ) ;
#10670 = CARTESIAN_POINT ( 'NONE',  ( -4.999999999999990230, 12.50000000000000000, -4.330127018922201643 ) ) ;
#10671 = DIRECTION ( 'NONE',  ( 0.000000000000000000, 1.000000000000000000, 0.000000000000000000 ) ) ;
#10672 = ADVANCED_FACE ( 'NONE', ( #4704 ), #83924, .T. ) ;
#10673 = CARTESIAN_POINT ( 'NONE',  ( 13.29999999999990301, 2.500000000000000000, 4.330127018922196314 ) ) ;
#10674 = CIRCLE ( 'NONE', #14870, 0.06509327318403745899 ) ;
#10675 = EDGE_CURVE ( 'NONE', #43290, #20224, #34863, .T. ) ;
#10676 = AXIS2_PLACEMENT_3D ( 'NONE', #37110, #116927, #97310 ) ;
#10677 = VERTEX_POINT ( 'NONE', #114678 ) ;
#10678 = ORIENTED_EDGE ( 'NONE', *, *, #93773, .T. ) ;
#10679 = CARTESIAN_POINT ( 'NONE',  ( 9.149999999999920419, 2.500000000000000000, 2.857883832488649301 ) ) ;
#10680 = FACE_OUTER_BOUND ( 'NONE', #54665, .T. ) ;
#10681 = ORIENTED_EDGE ( 'NONE', *, *, #124698, .F. ) ;
#10682 = CARTESIAN_POINT ( 'NONE',  ( -3.350000000000031619, 2.500000000000000000, -5.702370205355749455 ) ) ;
#10683 = CARTESIAN_POINT ( 'NONE',  ( -4.150000000000025224, 2.500000000000000000, 7.288010851410849256 ) ) ;
#10684 = EDGE_LOOP ( 'NONE', ( #129611, #10396, #228, #107681 ) ) ;
#10685 = CONICAL_SURFACE ( 'NONE', #4416, 0.09999999999999982514, 0.003490658503988666988 ) ;
#10686 = CONICAL_SURFACE ( 'NONE', #108895, 0.09999999999999982514, 0.003490658503988666988 ) ;
#10687 = DIRECTION ( 'NONE',  ( 0.000000000000000000, -0.9999939076577903929, 0.003490651415223739937 ) ) ;
#10688 = EDGE_LOOP ( 'NONE', ( #47845, #110115 ) ) ;
#10689 = ORIENTED_EDGE ( 'NONE', *, *, #5632, .F. ) ;
#10690 = DIRECTION ( 'NONE',  ( -4.274815082592931898E-19, -0.9999939076577903929, -0.003490651415223739937 ) ) ;
#10691 = DIRECTION ( 'NONE',  ( -0.000000000000000000, 1.000000000000000000, -0.000000000000000000 ) ) ;
#10692 = CARTESIAN_POINT ( 'NONE',  ( -1.650000000000034772, 12.50000000000000000, 2.099970236277060032 ) ) ;
#10693 = DIRECTION ( 'NONE',  ( 0.000000000000000000, -0.000000000000000000, 1.000000000000000000 ) ) ;
#10694 = CONICAL_SURFACE ( 'NONE', #113118, 0.09999999999999982514, 0.003490658503988666988 ) ;
#10695 = CIRCLE ( 'NONE', #25371, 0.1000000000000002554 ) ;
#10696 = CARTESIAN_POINT ( 'NONE',  ( 5.649999999999934630, 2.500000000000000000, 6.148780366869520897 ) ) ;
#10697 = EDGE_LOOP ( 'NONE', ( #109898, #53620, #81214, #33966 ) ) ;
#10698 = CARTESIAN_POINT ( 'NONE',  ( -8.550000000000007816, 12.50000000000000000, 6.213873640053558134 ) ) ;
#10699 = EDGE_CURVE ( 'NONE', #42755, #21163, #127892, .T. ) ;
#10700 = ADVANCED_FACE ( 'NONE', ( #13896 ), #85225, .T. ) ;
#10701 = VERTEX_POINT ( 'NONE', #55125 ) ;
#10702 = CARTESIAN_POINT ( 'NONE',  ( -11.84999999999999609, 2.500000000000000000, 2.411473670974873862 ) ) ;
#10703 = DIRECTION ( 'NONE',  ( 0.000000000000000000, 0.000000000000000000, 1.000000000000000000 ) ) ;
#10704 = EDGE_CURVE ( 'NONE', #16035, #48618, #50616, .T. ) ;
#10705 = AXIS2_PLACEMENT_3D ( 'NONE', #99019, #87884, #78093 ) ;
#10706 = CIRCLE ( 'NONE', #4438, 0.09999999999999982514 ) ;
#10707 = CARTESIAN_POINT ( 'NONE',  ( 186.0885416670080872, -6.551208109652273848, -3.782341765625003571 ) ) ;
#10708 = DIRECTION ( 'NONE',  ( 0.000000000000000000, -0.9999939076577903929, 0.003490651415223739937 ) ) ;
#10709 = DIRECTION ( 'NONE',  ( -0.000000000000000000, -1.000000000000000000, -0.000000000000000000 ) ) ;
#10710 = ADVANCED_FACE ( 'NONE', ( #115975 ), #53206, .T. ) ;
#10711 = CARTESIAN_POINT ( 'NONE',  ( 10.84999999999990905, 2.500000000000000000, 1.372243186433545370 ) ) ;
#10712 = CARTESIAN_POINT ( 'NONE',  ( 179.5000000000000000, 0.000000000000000000, 0.000000000000000000 ) ) ;
#10713 = EDGE_LOOP ( 'NONE', ( #53905, #115457 ) ) ;
#10714 = ADVANCED_FACE ( 'NONE', ( #3444 ), #90306, .T. ) ;
#10715 = DIRECTION ( 'NONE',  ( -0.000000000000000000, 1.000000000000000000, -0.000000000000000000 ) ) ;
#10716 = EDGE_CURVE ( 'NONE', #74312, #27189, #29697, .T. ) ;
#10717 = DIRECTION ( 'NONE',  ( -0.000000000000000000, -1.000000000000000000, -0.000000000000000000 ) ) ;
#10718 = FACE_OUTER_BOUND ( 'NONE', #60015, .T. ) ;
#10719 = EDGE_LOOP ( 'NONE', ( #55411, #61029, #45707, #39880 ) ) ;
#10720 = EDGE_CURVE ( 'NONE', #56841, #123082, #117235, .T. ) ;
#10721 = DIRECTION ( 'NONE',  ( -0.000000000000000000, 1.000000000000000000, -0.000000000000000000 ) ) ;
#10722 = ORIENTED_EDGE ( 'NONE', *, *, #36268, .F. ) ;
#10723 = ORIENTED_EDGE ( 'NONE', *, *, #82134, .F. ) ;
#10724 = DIRECTION ( 'NONE',  ( 0.000000000000000000, 0.000000000000000000, 1.000000000000000000 ) ) ;
#10725 = AXIS2_PLACEMENT_3D ( 'NONE', #27427, #105362, #88948 ) ;
#10726 = AXIS2_PLACEMENT_3D ( 'NONE', #65082, #54002, #14689 ) ;
#10727 = VERTEX_POINT ( 'NONE', #67493 ) ;
#10728 = CARTESIAN_POINT ( 'NONE',  ( 187.3593750003414016, 0.000000000000000000, 7.564683531250000925 ) ) ;
#10729 = FACE_OUTER_BOUND ( 'NONE', #107087, .T. ) ;
#10730 = EDGE_LOOP ( 'NONE', ( #88628, #25723 ) ) ;
#10732 = CARTESIAN_POINT ( 'NONE',  ( -6.650000000000018119, 12.50000000000000000, -7.188010851410854052 ) ) ;
#10731 = AXIS2_PLACEMENT_3D ( 'NONE', #94956, #65472, #77867 ) ;
#10733 = CIRCLE ( 'NONE', #25410, 0.1000000000000002554 ) ;
#10734 = FACE_OUTER_BOUND ( 'NONE', #116078, .T. ) ;
#10735 = VECTOR ( 'NONE', #35020, 1000.000000000000000 ) ;
#10736 = DIRECTION ( 'NONE',  ( 0.000000000000000000, 1.000000000000000000, 0.000000000000000000 ) ) ;
#10737 = ADVANCED_FACE ( 'NONE', ( #47896 ), #119557, .T. ) ;
#10738 = EDGE_LOOP ( 'NONE', ( #9690, #40134, #37091, #123826 ) ) ;
#10739 = EDGE_LOOP ( 'NONE', ( #68036, #16677, #76196, #53537 ) ) ;
#10740 = VERTEX_POINT ( 'NONE', #76699 ) ;
#10741 = FACE_OUTER_BOUND ( 'NONE', #54431, .T. ) ;
#10742 = FACE_OUTER_BOUND ( 'NONE', #119104, .T. ) ;
#10743 = DIRECTION ( 'NONE',  ( 0.000000000000000000, 1.000000000000000000, 0.000000000000000000 ) ) ;
#10744 = FACE_BOUND ( 'NONE', #127212, .T. ) ;
#10745 = ORIENTED_EDGE ( 'NONE', *, *, #58487, .F. ) ;
#10746 = LINE ( 'NONE', #121369, #67894 ) ;
#10747 = CARTESIAN_POINT ( 'NONE',  ( -1.050000000000038680, 12.50000000000000000, 2.511473670974873507 ) ) ;
#10748 = ORIENTED_EDGE ( 'NONE', *, *, #84745, .F. ) ;
#10749 = DIRECTION ( 'NONE',  ( 0.000000000000000000, -0.9999939076577903929, 0.003490651415223739937 ) ) ;
#10750 = LINE ( 'NONE', #30450, #67976 ) ;
#10751 = ADVANCED_FACE ( 'NONE', ( #108079 ), #16468, .T. ) ;
#10752 = CARTESIAN_POINT ( 'NONE',  ( 12.29999999999990301, 2.500000000000000000, -0.3464101615137782364 ) ) ;
#10753 = DIRECTION ( 'NONE',  ( 0.000000000000000000, 1.000000000000000000, 0.000000000000000000 ) ) ;
#10754 = DIRECTION ( 'NONE',  ( 0.000000000000000000, 1.000000000000000000, 0.000000000000000000 ) ) ;
#10755 = CARTESIAN_POINT ( 'NONE',  ( 11.89999999999990798, 12.50000000000000000, -4.611443907251939756 ) ) ;
#10756 = CARTESIAN_POINT ( 'NONE',  ( -14.14999999999998614, 2.500000000000000000, 2.165063509461101265 ) ) ;
#10757 = VECTOR ( 'NONE', #106512, 1000.000000000000000 ) ;
#10758 = AXIS2_PLACEMENT_3D ( 'NONE', #68332, #30366, #120663 ) ;
#10759 = VERTEX_POINT ( 'NONE', #66222 ) ;
#10760 = VERTEX_POINT ( 'NONE', #38067 ) ;
#10761 = EDGE_LOOP ( 'NONE', ( #6609, #14538 ) ) ;
#10762 = VERTEX_POINT ( 'NONE', #39380 ) ;
#10763 = CARTESIAN_POINT ( 'NONE',  ( 11.89999999999990443, 2.500000000000000000, -0.3464101615137782364 ) ) ;
#10764 = DIRECTION ( 'NONE',  ( 1.000000000000000000, -0.000000000000000000, -0.000000000000000000 ) ) ;
#10765 = EDGE_LOOP ( 'NONE', ( #127914, #49127, #24922, #34068 ) ) ;
#10766 = EDGE_CURVE ( 'NONE', #26528, #3892, #23422, .T. ) ;
#10767 = FACE_BOUND ( 'NONE', #21816, .T. ) ;
#10768 = CONICAL_SURFACE ( 'NONE', #127873, 0.09999999999999982514, 0.003490658503988666988 ) ;
#10769 = CARTESIAN_POINT ( 'NONE',  ( 6.249999999999932498, 2.500000000000000000, 5.702370205355745014 ) ) ;
#10770 = CONICAL_SURFACE ( 'NONE', #4504, 0.09999999999999982514, 0.003490658503988666988 ) ;
#10771 = CARTESIAN_POINT ( 'NONE',  ( 14.99999999999989342, 2.500000000000000000, -0.6928203230275541413 ) ) ;
#10772 = AXIS2_PLACEMENT_3D ( 'NONE', #48236, #117589, #105870 ) ;
#10773 = PLANE ( 'NONE',  #3158 ) ;
#10774 = DIRECTION ( 'NONE',  ( 0.000000000000000000, 0.000000000000000000, -1.000000000000000000 ) ) ;
#10775 = CARTESIAN_POINT ( 'NONE',  ( 14.79999999999989235, 12.50000000000000000, 0.3464101615137735735 ) ) ;
#10777 = DIRECTION ( 'NONE',  ( -4.274815082592931898E-19, -0.9999939076577903929, -0.003490651415223739937 ) ) ;
#10776 =( BOUNDED_CURVE ( )  B_SPLINE_CURVE ( 2, ( #120233, #10277, #71122, #69842, #60679, #49569, #120867 ),
 .UNSPECIFIED., .F., .F. ) 
 B_SPLINE_CURVE_WITH_KNOTS ( ( 3, 2, 2, 3 ),
 ( 0.7857142857142862535, 0.8095238095238102005, 0.8333333333333340365, 0.8571428571428578724 ),
 .UNSPECIFIED. ) 
 CURVE ( )  GEOMETRIC_REPRESENTATION_ITEM ( )  RATIONAL_B_SPLINE_CURVE ( ( 0.9999999999999968914, 0.8660254037844418162, 1.000000000000000000, 0.8660254037844387076, 1.000000000000000000, 0.8660254037844343777, 1.000000000000004441 ) ) 
 REPRESENTATION_ITEM ( '' )  );
#10778 = FACE_OUTER_BOUND ( 'NONE', #80822, .T. ) ;
#10779 = DIRECTION ( 'NONE',  ( 0.000000000000000000, 0.000000000000000000, 1.000000000000000000 ) ) ;
#10780 = ORIENTED_EDGE ( 'NONE', *, *, #96681, .T. ) ;
#10781 = VECTOR ( 'NONE', #93342, 1000.000000000000000 ) ;
#10782 = ORIENTED_EDGE ( 'NONE', *, *, #123892, .F. ) ;
#10783 = CIRCLE ( 'NONE', #44252, 0.06509327318403745899 ) ;
#10784 = VERTEX_POINT ( 'NONE', #126454 ) ;
#10785 = ORIENTED_EDGE ( 'NONE', *, *, #77814, .F. ) ;
#10786 = ORIENTED_EDGE ( 'NONE', *, *, #10990, .F. ) ;
#10787 = ORIENTED_EDGE ( 'NONE', *, *, #90608, .T. ) ;
#10788 = CIRCLE ( 'NONE', #119468, 0.06509327318403745899 ) ;
#10789 = CARTESIAN_POINT ( 'NONE',  ( 6.249999999999932498, 12.50000000000000000, -2.792790559304616504 ) ) ;
#10790 = EDGE_LOOP ( 'NONE', ( #104052, #13089, #11313, #6444 ) ) ;
#10791 = EDGE_CURVE ( 'NONE', #74876, #2020, #27613, .T. ) ;
#10792 = CARTESIAN_POINT ( 'NONE',  ( -10.85000000000000142, 2.500000000000000000, 6.595190528383296780 ) ) ;
#10793 = CONICAL_SURFACE ( 'NONE', #119567, 0.09999999999999999167, 0.003490658503988666988 ) ;
#10794 = VECTOR ( 'NONE', #109037, 1000.000000000000000 ) ;
#10795 = CARTESIAN_POINT ( 'NONE',  ( 185.8177083336747444, 4.367472073101515306, 7.564683531250000925 ) ) ;
#10796 = FACE_OUTER_BOUND ( 'NONE', #96872, .T. ) ;
#10797 = DIRECTION ( 'NONE',  ( -0.000000000000000000, -1.000000000000000000, -0.000000000000000000 ) ) ;
#10798 = VERTEX_POINT ( 'NONE', #97625 ) ;
#10799 = CARTESIAN_POINT ( 'NONE',  ( -12.69999999999999218, 2.500000000000000000, -4.576537180435974683 ) ) ;
#10800 = EDGE_CURVE ( 'NONE', #97332, #64242, #44355, .T. ) ;
#10801 = VERTEX_POINT ( 'NONE', #66865 ) ;
#10802 = EDGE_LOOP ( 'NONE', ( #77142, #125439, #22246, #44843 ) ) ;
#10803 = FACE_OUTER_BOUND ( 'NONE', #27578, .T. ) ;
#10804 = ADVANCED_FACE ( 'NONE', ( #79291 ), #77792, .T. ) ;
#10805 = DIRECTION ( 'NONE',  ( -4.274815082592931898E-19, -0.9999939076577903929, -0.003490651415223739937 ) ) ;
#10807 = EDGE_CURVE ( 'NONE', #13428, #20160, #4612, .T. ) ;
#10806 = DIRECTION ( 'NONE',  ( -4.274815082592931898E-19, -0.9999939076577903929, -0.003490651415223739937 ) ) ;
#10808 = ADVANCED_FACE ( 'NONE', ( #98258 ), #71435, .T. ) ;
#10809 = EDGE_CURVE ( 'NONE', #79461, #98821, #94430, .T. ) ;
#10810 = ORIENTED_EDGE ( 'NONE', *, *, #98310, .T. ) ;
#10811 = ORIENTED_EDGE ( 'NONE', *, *, #65834, .T. ) ;
#10812 = DIRECTION ( 'NONE',  ( -1.000000000000000000, -0.000000000000000000, -0.000000000000000000 ) ) ;
#10814 = EDGE_CURVE ( 'NONE', #63398, #69417, #31842, .T. ) ;
#10813 = CARTESIAN_POINT ( 'NONE',  ( 5.449999999999937117, 12.50000000000000000, -6.495190528383302464 ) ) ;
#10815 = DIRECTION ( 'NONE',  ( 0.000000000000000000, -0.9999939076577903929, 0.003490651415223739937 ) ) ;
#10817 = CARTESIAN_POINT ( 'NONE',  ( -9.800000000000006040, 2.500000000000000000, 0.3464101615137735735 ) ) ;
#10816 = AXIS2_PLACEMENT_3D ( 'NONE', #1908, #10445, #111879 ) ;
#10818 = ORIENTED_EDGE ( 'NONE', *, *, #44863, .T. ) ;
#10819 = AXIS2_PLACEMENT_3D ( 'NONE', #128754, #78997, #90734 ) ;
#10820 = AXIS2_PLACEMENT_3D ( 'NONE', #55136, #23751, #95065 ) ;
#10821 = B_SPLINE_CURVE_WITH_KNOTS ( 'NONE', 3,
 ( #98586, #61274, #49524, #110359, #89434, #100534, #101194, #71083 ),
 .UNSPECIFIED., .F., .F.,
 ( 4, 2, 2, 4 ),
 ( 0.002994103107820098031, 0.003957537843903998452, 0.004920972579987898873, 0.006847842052155699716 ),
 .UNSPECIFIED. ) ;
#10822 = LINE ( 'NONE', #20681, #4200 ) ;
#10823 = EDGE_CURVE ( 'NONE', #28983, #34057, #127723, .T. ) ;
#10824 = ORIENTED_EDGE ( 'NONE', *, *, #85053, .T. ) ;
#10825 = LINE ( 'NONE', #100515, #25987 ) ;
#10826 = ADVANCED_FACE ( 'NONE', ( #68156 ), #121712, .T. ) ;
#10828 = EDGE_CURVE ( 'NONE', #35122, #42109, #78651, .T. ) ;
#10827 = AXIS2_PLACEMENT_3D ( 'NONE', #54230, #11716, #121667 ) ;
#10829 = ORIENTED_EDGE ( 'NONE', *, *, #125053, .F. ) ;
#10830 = CARTESIAN_POINT ( 'NONE',  ( 17.50000000000000000, 2.500000000000000000, 4.000000000000000000 ) ) ;
#10831 = CIRCLE ( 'NONE', #98667, 0.06509327318403745899 ) ;
#10832 = CARTESIAN_POINT ( 'NONE',  ( 81.97074409615474622, -3.937872622146114221, 6.123955080831738229 ) ) ;
#10833 = CARTESIAN_POINT ( 'NONE',  ( -10.40000000000000213, 2.500000000000000000, 0.7928203230275495672 ) ) ;
#10834 = CIRCLE ( 'NONE', #42266, 0.06509327318403745899 ) ;
#10836 = EDGE_CURVE ( 'NONE', #26300, #67411, #119658, .T. ) ;
#10835 = DIRECTION ( 'NONE',  ( -0.000000000000000000, 1.000000000000000000, -0.000000000000000000 ) ) ;
#10837 = ORIENTED_EDGE ( 'NONE', *, *, #33947, .F. ) ;
#10838 = CIRCLE ( 'NONE', #84008, 0.09999999999999982514 ) ;
#10839 = DIRECTION ( 'NONE',  ( 0.000000000000000000, -0.9999939076577903929, 0.003490651415223739937 ) ) ;
#10840 = CARTESIAN_POINT ( 'NONE',  ( -2.700000000000029932, 12.50000000000000000, -4.741630453620015118 ) ) ;
#10841 = ORIENTED_EDGE ( 'NONE', *, *, #55764, .F. ) ;
#10842 = ORIENTED_EDGE ( 'NONE', *, *, #114460, .T. ) ;
#10843 = ORIENTED_EDGE ( 'NONE', *, *, #122751, .T. ) ;
#10844 = CARTESIAN_POINT ( 'NONE',  ( 10.59999999999990905, 12.50000000000000000, 4.676537180435972552 ) ) ;
#10845 = CARTESIAN_POINT ( 'NONE',  ( 179.5000000000000000, -1.000000000000025535, 7.634788798650553154 ) ) ;
#10846 = CARTESIAN_POINT ( 'NONE',  ( 2.499999999999945377, 2.500000000000000000, 4.922947341949748257 ) ) ;
#10847 = DIRECTION ( 'NONE',  ( 0.000000000000000000, 1.000000000000000000, 0.000000000000000000 ) ) ;
#10848 = DIRECTION ( 'NONE',  ( -0.000000000000000000, 1.000000000000000000, -0.000000000000000000 ) ) ;
#10849 = DIRECTION ( 'NONE',  ( -0.000000000000000000, -1.000000000000000000, -0.000000000000000000 ) ) ;
#10850 = DIRECTION ( 'NONE',  ( -0.000000000000000000, 1.000000000000000000, -0.000000000000000000 ) ) ;
#10851 = DIRECTION ( 'NONE',  ( -0.000000000000000000, -1.000000000000000000, -0.000000000000000000 ) ) ;
#10852 = LINE ( 'NONE', #8291, #38040 ) ;
#10853 = AXIS2_PLACEMENT_3D ( 'NONE', #34422, #123413, #92676 ) ;
#10854 = CIRCLE ( 'NONE', #21343, 0.06509327318403745899 ) ;
#10855 = ORIENTED_EDGE ( 'NONE', *, *, #76135, .F. ) ;
#10856 = CARTESIAN_POINT ( 'NONE',  ( -8.950000000000004619, 2.500000000000000000, 6.048780366869521252 ) ) ;
#10857 = DIRECTION ( 'NONE',  ( 0.000000000000000000, 0.000000000000000000, -1.000000000000000000 ) ) ;
#10858 = DIRECTION ( 'NONE',  ( 0.000000000000000000, 1.000000000000000000, 0.000000000000000000 ) ) ;
#10859 = FACE_OUTER_BOUND ( 'NONE', #119418, .T. ) ;
#10860 = AXIS2_PLACEMENT_3D ( 'NONE', #126834, #19443, #47630 ) ;
#10861 = AXIS2_PLACEMENT_3D ( 'NONE', #50144, #71059, #12756 ) ;
#10862 = ORIENTED_EDGE ( 'NONE', *, *, #54967, .F. ) ;
#10863 = DIRECTION ( 'NONE',  ( 0.000000000000000000, 1.000000000000000000, 0.000000000000000000 ) ) ;
#10864 = ADVANCED_FACE ( 'NONE', ( #58996 ), #71546, .T. ) ;
#10865 = AXIS2_PLACEMENT_3D ( 'NONE', #54495, #94414, #114703 ) ;
#10866 = AXIS2_PLACEMENT_3D ( 'NONE', #17294, #47442, #106978 ) ;
#10867 = EDGE_CURVE ( 'NONE', #70927, #30745, #13030, .T. ) ;
#10868 = DIRECTION ( 'NONE',  ( -0.000000000000000000, 1.000000000000000000, -0.000000000000000000 ) ) ;
#10870 = EDGE_LOOP ( 'NONE', ( #38015, #121632 ) ) ;
#10869 = DIRECTION ( 'NONE',  ( 0.000000000000000000, 1.000000000000000000, 0.000000000000000000 ) ) ;
#10871 = CIRCLE ( 'NONE', #111227, 0.06509327318403745899 ) ;
#10872 = ORIENTED_EDGE ( 'NONE', *, *, #61935, .F. ) ;
#10873 = EDGE_CURVE ( 'NONE', #102784, #15089, #62225, .T. ) ;
#10875 = AXIS2_PLACEMENT_3D ( 'NONE', #61001, #21076, #29610 ) ;
#10874 = DIRECTION ( 'NONE',  ( 0.000000000000000000, 0.000000000000000000, 1.000000000000000000 ) ) ;
#10876 = EDGE_LOOP ( 'NONE', ( #14427, #11680, #110711, #127759 ) ) ;
#10877 = AXIS2_PLACEMENT_3D ( 'NONE', #10598, #88531, #99006 ) ;
#10879 = ORIENTED_EDGE ( 'NONE', *, *, #26098, .F. ) ;
#10878 = AXIS2_PLACEMENT_3D ( 'NONE', #93763, #64293, #7946 ) ;
#10880 = AXIS2_PLACEMENT_3D ( 'NONE', #124487, #125743, #104816 ) ;
#10881 = DIRECTION ( 'NONE',  ( -0.000000000000000000, -1.000000000000000000, -0.000000000000000000 ) ) ;
#10882 = CIRCLE ( 'NONE', #59040, 0.09999999999999982514 ) ;
#10883 = DIRECTION ( 'NONE',  ( 0.000000000000000000, 1.000000000000000000, 0.000000000000000000 ) ) ;
#10884 = DIRECTION ( 'NONE',  ( 0.000000000000000000, 1.000000000000000000, 0.000000000000000000 ) ) ;
#10885 = CARTESIAN_POINT ( 'NONE',  ( -6.050000000000018474, 12.50000000000000000, 6.776507416713035248 ) ) ;
#10886 = VERTEX_POINT ( 'NONE', #20992 ) ;
#10887 = CONICAL_SURFACE ( 'NONE', #23434, 0.1000000000000002554, 0.003490658503988666988 ) ;
#10888 = FACE_OUTER_BOUND ( 'NONE', #104389, .T. ) ;
#10889 = VERTEX_POINT ( 'NONE', #40664 ) ;
#10890 = CARTESIAN_POINT ( 'NONE',  ( 16.73289298692834492, 0.7002450284443078043, 5.897165230072824116 ) ) ;
#10891 = DIRECTION ( 'NONE',  ( 0.000000000000000000, 1.000000000000000000, 0.000000000000000000 ) ) ;
#10892 = EDGE_LOOP ( 'NONE', ( #24681, #83998, #116537, #71270 ) ) ;
#10893 = ORIENTED_EDGE ( 'NONE', *, *, #33180, .T. ) ;
#10894 = EDGE_LOOP ( 'NONE', ( #62682, #127832 ) ) ;
#10895 = ORIENTED_EDGE ( 'NONE', *, *, #107631, .T. ) ;
#10896 = CARTESIAN_POINT ( 'NONE',  ( 0.3999999999999563904, 2.500000000000000000, 3.637306695894644726 ) ) ;
#10897 = DIRECTION ( 'NONE',  ( 0.000000000000000000, 0.000000000000000000, -1.000000000000000000 ) ) ;
#10898 = DIRECTION ( 'NONE',  ( 0.000000000000000000, 0.000000000000000000, 1.000000000000000000 ) ) ;
#10899 = FACE_BOUND ( 'NONE', #16600, .T. ) ;
#10900 = CARTESIAN_POINT ( 'NONE',  ( 4.599999999999937472, 2.500000000000000000, 0.7928203230275495672 ) ) ;
#10901 = CARTESIAN_POINT ( 'NONE',  ( 184.7395833340161460, 4.445597072760117285, 7.699999999999999289 ) ) ;
#10902 = DIRECTION ( 'NONE',  ( 0.000000000000000000, 0.000000000000000000, -1.000000000000000000 ) ) ;
#10903 = CARTESIAN_POINT ( 'NONE',  ( -5.650000000000019895, 2.500000000000000000, 2.511473670974873507 ) ) ;
#10904 = CONICAL_SURFACE ( 'NONE', #69418, 0.1000000000000000472, 0.003490658503988666988 ) ;
#10905 = AXIS2_PLACEMENT_3D ( 'NONE', #78045, #125217, #116674 ) ;
#10907 = AXIS2_PLACEMENT_3D ( 'NONE', #1356, #20368, #69448 ) ;
#10906 = CARTESIAN_POINT ( 'NONE',  ( -12.94999999999999218, 12.50000000000000000, -2.165063509461099489 ) ) ;
#10908 = DIRECTION ( 'NONE',  ( 0.000000000000000000, -0.000000000000000000, 1.000000000000000000 ) ) ;
#10909 = CARTESIAN_POINT ( 'NONE',  ( 11.89999999999990798, 2.500000000000000000, -3.883716857408426648 ) ) ;
#10910 = CONICAL_SURFACE ( 'NONE', #17168, 0.1000000000000002554, 0.003490658503988666988 ) ;
#10912 = FACE_OUTER_BOUND ( 'NONE', #58568, .T. ) ;
#10911 = AXIS2_PLACEMENT_3D ( 'NONE', #117115, #125021, #26185 ) ;
#10913 = VECTOR ( 'NONE', #38048, 1000.000000000000000 ) ;
#10914 = ORIENTED_EDGE ( 'NONE', *, *, #20478, .T. ) ;
#10915 = EDGE_LOOP ( 'NONE', ( #106284, #71012, #54914, #88635 ) ) ;
#10916 = ORIENTED_EDGE ( 'NONE', *, *, #66892, .T. ) ;
#10917 = ORIENTED_EDGE ( 'NONE', *, *, #23704, .F. ) ;
#10919 = EDGE_CURVE ( 'NONE', #61864, #44929, #69481, .T. ) ;
#10918 = VECTOR ( 'NONE', #6768, 1000.000000000000000 ) ;
#10920 = DIRECTION ( 'NONE',  ( 0.000000000000000000, 0.000000000000000000, 1.000000000000000000 ) ) ;
#10921 = CIRCLE ( 'NONE', #52808, 0.1000000000000002554 ) ;
#10922 = CARTESIAN_POINT ( 'NONE',  ( 105.5000000000000142, -1.500000000000000222, -1.322875655532295136 ) ) ;
#10923 = ORIENTED_EDGE ( 'NONE', *, *, #87822, .F. ) ;
#10924 = ADVANCED_FACE ( 'NONE', ( #90365 ), #29781, .T. ) ;
#10925 = FACE_BOUND ( 'NONE', #13229, .T. ) ;
#10926 = AXIS2_PLACEMENT_3D ( 'NONE', #22808, #62726, #20853 ) ;
#10927 = DIRECTION ( 'NONE',  ( 0.000000000000000000, -0.000000000000000000, 1.000000000000000000 ) ) ;
#10928 = ORIENTED_EDGE ( 'NONE', *, *, #125660, .T. ) ;
#10929 = CARTESIAN_POINT ( 'NONE',  ( -9.150000000000009237, 12.50000000000000000, 1.537336459617582918 ) ) ;
#10930 = CARTESIAN_POINT ( 'NONE',  ( -6.250000000000021316, 2.500000000000000000, -5.702370205355749455 ) ) ;
#10931 = ADVANCED_FACE ( 'NONE', ( #60917 ), #89738, .T. ) ;
#10932 = DIRECTION ( 'NONE',  ( 0.000000000000000000, 0.000000000000000000, 1.000000000000000000 ) ) ;
#10933 = FACE_OUTER_BOUND ( 'NONE', #2957, .T. ) ;
#10934 = EDGE_LOOP ( 'NONE', ( #25257, #54587, #106461, #27104 ) ) ;
#10935 = DIRECTION ( 'NONE',  ( -0.000000000000000000, 1.000000000000000000, -0.000000000000000000 ) ) ;
#10936 = AXIS2_PLACEMENT_3D ( 'NONE', #48764, #97205, #48112 ) ;
#10937 = ORIENTED_EDGE ( 'NONE', *, *, #77809, .F. ) ;
#10938 = EDGE_LOOP ( 'NONE', ( #7864, #29800 ) ) ;
#10939 = CARTESIAN_POINT ( 'NONE',  ( 8.099999999999923261, 12.50000000000000000, -3.983716857408426293 ) ) ;
#10940 = CARTESIAN_POINT ( 'NONE',  ( -5.800000000000018474, 2.500000000000000000, 4.430127018922196847 ) ) ;
#10941 = VERTEX_POINT ( 'NONE', #10517 ) ;
#10942 = DIRECTION ( 'NONE',  ( 0.000000000000000000, 0.000000000000000000, 1.000000000000000000 ) ) ;
#10943 = CIRCLE ( 'NONE', #36120, 0.06509327318403745899 ) ;
#10945 = DIRECTION ( 'NONE',  ( 0.000000000000000000, 0.000000000000000000, 1.000000000000000000 ) ) ;
#10944 = STYLED_ITEM ( 'NONE', ( #84767 ), #58374 ) ;
#10947 = ADVANCED_FACE ( 'NONE', ( #9890 ), #92477, .T. ) ;
#10946 = DIRECTION ( 'NONE',  ( -0.000000000000000000, 1.000000000000000000, -0.000000000000000000 ) ) ;
#10948 = CARTESIAN_POINT ( 'NONE',  ( 12.29999999999990656, 2.500000000000000000, 3.983716857408420964 ) ) ;
#10949 = ORIENTED_EDGE ( 'NONE', *, *, #67403, .T. ) ;
#10950 = CARTESIAN_POINT ( 'NONE',  ( -11.64999999999999680, 2.500000000000000000, -2.857883832488649745 ) ) ;
#10951 = AXIS2_PLACEMENT_3D ( 'NONE', #39613, #59245, #57945 ) ;
#10952 = ORIENTED_EDGE ( 'NONE', *, *, #48216, .F. ) ;
#10953 = DIRECTION ( 'NONE',  ( 0.000000000000000000, 0.000000000000000000, 1.000000000000000000 ) ) ;
#10954 = CONICAL_SURFACE ( 'NONE', #115414, 0.1000000000000000472, 0.003490658503988666988 ) ;
#10956 = ADVANCED_FACE ( 'NONE', ( #82511 ), #102141, .T. ) ;
#10955 = AXIS2_PLACEMENT_3D ( 'NONE', #108841, #11290, #110146 ) ;
#10957 = ORIENTED_EDGE ( 'NONE', *, *, #27576, .T. ) ;
#10958 = AXIS2_PLACEMENT_3D ( 'NONE', #36352, #7499, #78197 ) ;
#10959 = PLANE ( 'NONE',  #93544 ) ;
#10960 = ORIENTED_EDGE ( 'NONE', *, *, #81749, .F. ) ;
#10961 = DIRECTION ( 'NONE',  ( 0.000000000000000000, 0.000000000000000000, 1.000000000000000000 ) ) ;
#10962 = CARTESIAN_POINT ( 'NONE',  ( 8.149999999999920419, 12.50000000000000000, -2.511473670974877948 ) ) ;
#10963 = EDGE_CURVE ( 'NONE', #65382, #113506, #49833, .T. ) ;
#10964 = CARTESIAN_POINT ( 'NONE',  ( 8.349999999999919709, 12.50000000000000000, 7.188010851410848723 ) ) ;
#10966 = EDGE_CURVE ( 'NONE', #53057, #107141, #61178, .T. ) ;
#10965 = DIRECTION ( 'NONE',  ( 0.000000000000000000, -0.000000000000000000, 1.000000000000000000 ) ) ;
#10967 = EDGE_CURVE ( 'NONE', #34976, #52139, #96662, .T. ) ;
#10968 = DIRECTION ( 'NONE',  ( 0.000000000000000000, 0.000000000000000000, 1.000000000000000000 ) ) ;
#10969 = ADVANCED_FACE ( 'NONE', ( #19714 ), #11166, .T. ) ;
#10970 = AXIS2_PLACEMENT_3D ( 'NONE', #48434, #98172, #30755 ) ;
#10971 = ORIENTED_EDGE ( 'NONE', *, *, #487, .F. ) ;
#10972 = EDGE_LOOP ( 'NONE', ( #89741, #81144, #33266, #127752 ) ) ;
#10973 = AXIS2_PLACEMENT_3D ( 'NONE', #39320, #79223, #39941 ) ;
#10974 = EDGE_LOOP ( 'NONE', ( #75182, #26315, #90798, #73399 ) ) ;
#10975 = LINE ( 'NONE', #120947, #76934 ) ;
#10977 = VECTOR ( 'NONE', #37893, 1000.000000000000000 ) ;
#10976 = FACE_OUTER_BOUND ( 'NONE', #68668, .T. ) ;
#10978 = CONICAL_SURFACE ( 'NONE', #115436, 0.1000000000000002554, 0.003490658503988666988 ) ;
#10979 = CIRCLE ( 'NONE', #48666, 0.1000000000000002554 ) ;
#10980 = EDGE_CURVE ( 'NONE', #27825, #50205, #51120, .T. ) ;
#10981 = FACE_OUTER_BOUND ( 'NONE', #6371, .T. ) ;
#10983 = VERTEX_POINT ( 'NONE', #111286 ) ;
#10982 = ORIENTED_EDGE ( 'NONE', *, *, #7307, .F. ) ;
#10984 = EDGE_LOOP ( 'NONE', ( #66985, #118411, #88207, #40553 ) ) ;
#10985 = ADVANCED_FACE ( 'NONE', ( #30192 ), #75744, .T. ) ;
#10986 = CARTESIAN_POINT ( 'NONE',  ( -6.850000000000017408, 12.50000000000000000, -6.841600689897077814 ) ) ;
#10987 = AXIS2_PLACEMENT_3D ( 'NONE', #3860, #103365, #24155 ) ;
#10988 = ORIENTED_EDGE ( 'NONE', *, *, #19548, .F. ) ;
#10989 = DIRECTION ( 'NONE',  ( -0.000000000000000000, 1.000000000000000000, -0.000000000000000000 ) ) ;
#10990 = EDGE_CURVE ( 'NONE', #48757, #97573, #94608, .T. ) ;
#10991 = EDGE_CURVE ( 'NONE', #77648, #102955, #20358, .T. ) ;
#10992 = DIRECTION ( 'NONE',  ( -0.000000000000000000, 1.000000000000000000, -0.000000000000000000 ) ) ;
#10993 = AXIS2_PLACEMENT_3D ( 'NONE', #108674, #19660, #59611 ) ;
#10994 = DIRECTION ( 'NONE',  ( -0.000000000000000000, 1.000000000000000000, -0.000000000000000000 ) ) ;
#10995 = CARTESIAN_POINT ( 'NONE',  ( 1.649999999999951505, 12.50000000000000000, 1.537336459617582918 ) ) ;
#10996 = CARTESIAN_POINT ( 'NONE',  ( -9.150000000000009237, 2.500000000000000000, -2.265063509461101798 ) ) ;
#10997 = DIRECTION ( 'NONE',  ( 0.000000000000000000, 0.000000000000000000, -1.000000000000000000 ) ) ;
#10998 = EDGE_CURVE ( 'NONE', #33342, #119894, #56943, .T. ) ;
#11000 = ADVANCED_FACE ( 'NONE', ( #705 ), #522, .T. ) ;
#10999 = DIRECTION ( 'NONE',  ( -0.000000000000000000, -1.000000000000000000, -0.000000000000000000 ) ) ;
#11001 = ORIENTED_EDGE ( 'NONE', *, *, #48554, .T. ) ;
#11002 = ORIENTED_EDGE ( 'NONE', *, *, #40574, .T. ) ;
#11003 = CARTESIAN_POINT ( 'NONE',  ( -10.80000000000000071, 2.500000000000000000, -0.1000000000000022815 ) ) ;
#11004 = DIRECTION ( 'NONE',  ( 1.000000000000000000, 0.000000000000000000, 0.000000000000000000 ) ) ;
#11005 = VERTEX_POINT ( 'NONE', #54960 ) ;
#11006 = ORIENTED_EDGE ( 'NONE', *, *, #56895, .F. ) ;
#11007 = CIRCLE ( 'NONE', #126024, 0.09999999999999982514 ) ;
#11008 = CARTESIAN_POINT ( 'NONE',  ( 185.0677083336747160, -4.367472073101514418, -7.564683531250002702 ) ) ;
#11009 = CARTESIAN_POINT ( 'NONE',  ( 1.899999999999949507, 2.500000000000000000, 4.676537180435972552 ) ) ;
#11010 = DIRECTION ( 'NONE',  ( 0.000000000000000000, -0.9999939076577903929, 0.003490651415223739937 ) ) ;
#11011 = CARTESIAN_POINT ( 'NONE',  ( -14.14999999999998792, 2.500000000000000000, -1.372243186433547812 ) ) ;
#11012 = DIRECTION ( 'NONE',  ( -0.000000000000000000, 1.000000000000000000, -0.000000000000000000 ) ) ;
#11013 = DIRECTION ( 'NONE',  ( 0.000000000000000000, 0.000000000000000000, -1.000000000000000000 ) ) ;
#11014 = VECTOR ( 'NONE', #93857, 1000.000000000000000 ) ;
#11015 = DIRECTION ( 'NONE',  ( -0.000000000000000000, -1.000000000000000000, -0.000000000000000000 ) ) ;
#11016 = CARTESIAN_POINT ( 'NONE',  ( -1.900000000000034106, 2.500000000000000000, 0.2464101615137735679 ) ) ;
#11017 = AXIS2_PLACEMENT_3D ( 'NONE', #102109, #51726, #122401 ) ;
#11018 = AXIS2_PLACEMENT_3D ( 'NONE', #30534, #96177, #20696 ) ;
#11019 = FACE_OUTER_BOUND ( 'NONE', #128007, .T. ) ;
#11020 = EDGE_LOOP ( 'NONE', ( #59276, #58185, #81162, #50206 ) ) ;
#11021 = AXIS2_PLACEMENT_3D ( 'NONE', #110037, #60309, #100212 ) ;
#11022 = EDGE_LOOP ( 'NONE', ( #32612, #54673, #14738, #102572 ) ) ;
#11023 = AXIS2_PLACEMENT_3D ( 'NONE', #128601, #109581, #68997 ) ;
#11024 = ORIENTED_EDGE ( 'NONE', *, *, #96532, .T. ) ;
#11025 = AXIS2_PLACEMENT_3D ( 'NONE', #56215, #57526, #43372 ) ;
#11026 = AXIS2_PLACEMENT_3D ( 'NONE', #92138, #111796, #102601 ) ;
#11027 = AXIS2_PLACEMENT_3D ( 'NONE', #95358, #89240, #19865 ) ;
#11028 = EDGE_LOOP ( 'NONE', ( #97553, #124010 ) ) ;
#11029 = ORIENTED_EDGE ( 'NONE', *, *, #83308, .F. ) ;
#11030 = FACE_OUTER_BOUND ( 'NONE', #55435, .T. ) ;
#11031 = DIRECTION ( 'NONE',  ( 0.000000000000000000, 1.000000000000000000, 0.000000000000000000 ) ) ;
#11032 = VECTOR ( 'NONE', #71087, 1000.000000000000000 ) ;
#11033 = EDGE_LOOP ( 'NONE', ( #79626, #43338, #121142, #37243 ) ) ;
#11034 = DIRECTION ( 'NONE',  ( 0.000000000000000000, -0.9999939076577903929, 0.003490651415223739937 ) ) ;
#11035 = EDGE_CURVE ( 'NONE', #85157, #29857, #98722, .T. ) ;
#11036 = FACE_OUTER_BOUND ( 'NONE', #98318, .T. ) ;
#11037 = EDGE_CURVE ( 'NONE', #117332, #48425, #64778, .T. ) ;
#11038 = DIRECTION ( 'NONE',  ( 0.000000000000000000, 1.000000000000000000, 0.000000000000000000 ) ) ;
#11040 = VERTEX_POINT ( 'NONE', #85070 ) ;
#11039 = CARTESIAN_POINT ( 'NONE',  ( -9.600000000000008527, 12.50000000000000000, -4.330127018922197202 ) ) ;
#11041 = DIRECTION ( 'NONE',  ( 0.000000000000000000, 0.000000000000000000, 1.000000000000000000 ) ) ;
#11042 = DIRECTION ( 'NONE',  ( 0.000000000000000000, 1.000000000000000000, 0.000000000000000000 ) ) ;
#11043 = ORIENTED_EDGE ( 'NONE', *, *, #7436, .F. ) ;
#11044 = ORIENTED_EDGE ( 'NONE', *, *, #116070, .F. ) ;
#11045 = ORIENTED_EDGE ( 'NONE', *, *, #20915, .F. ) ;
#11046 = VERTEX_POINT ( 'NONE', #62855 ) ;
#11047 = DIRECTION ( 'NONE',  ( 0.000000000000000000, 0.000000000000000000, 1.000000000000000000 ) ) ;
#11049 = AXIS2_PLACEMENT_3D ( 'NONE', #106213, #16517, #97031 ) ;
#11048 = CARTESIAN_POINT ( 'NONE',  ( -9.150000000000009237, 2.500000000000000000, -7.088010851410848190 ) ) ;
#11050 = DIRECTION ( 'NONE',  ( 0.000000000000000000, -0.9999939076577903929, 0.003490651415223739937 ) ) ;
#11051 = CIRCLE ( 'NONE', #23584, 0.09999999999999982514 ) ;
#11052 = DIRECTION ( 'NONE',  ( 0.000000000000000000, 0.000000000000000000, 1.000000000000000000 ) ) ;
#11053 = VERTEX_POINT ( 'NONE', #13088 ) ;
#11054 = CARTESIAN_POINT ( 'NONE',  ( 9.149999999999916866, 12.50000000000000000, 7.122917578226811486 ) ) ;
#11055 = CARTESIAN_POINT ( 'NONE',  ( 20.80940928220344688, -0.7000174339600981899, -4.161255421338320382 ) ) ;
#11056 = LINE ( 'NONE', #39910, #278 ) ;
#11057 = DIRECTION ( 'NONE',  ( 0.000000000000000000, 0.000000000000000000, 1.000000000000000000 ) ) ;
#11058 = CIRCLE ( 'NONE', #15248, 0.1000000000000000472 ) ;
#11059 = AXIS2_PLACEMENT_3D ( 'NONE', #88942, #39227, #37901 ) ;
#11060 = AXIS2_PLACEMENT_3D ( 'NONE', #47860, #7909, #25614 ) ;
#11061 = EDGE_LOOP ( 'NONE', ( #14258, #29682, #87909, #93982 ) ) ;
#11062 = AXIS2_PLACEMENT_3D ( 'NONE', #66272, #6676, #46634 ) ;
#11063 = EDGE_LOOP ( 'NONE', ( #53079, #15574 ) ) ;
#11064 = ORIENTED_EDGE ( 'NONE', *, *, #110064, .F. ) ;
#11065 = DIRECTION ( 'NONE',  ( 0.000000000000000000, 0.000000000000000000, 1.000000000000000000 ) ) ;
#11066 = CARTESIAN_POINT ( 'NONE',  ( -1.650000000000035660, 2.500000000000000000, 2.957883832488649389 ) ) ;
#11067 = FACE_BOUND ( 'NONE', #72849, .T. ) ;
#11068 = CARTESIAN_POINT ( 'NONE',  ( -13.34999999999999076, 12.50000000000000000, 2.857883832488652853 ) ) ;
#11070 = DIRECTION ( 'NONE',  ( 0.000000000000000000, -0.000000000000000000, 1.000000000000000000 ) ) ;
#11069 = AXIS2_PLACEMENT_3D ( 'NONE', #3217, #21557, #43158 ) ;
#11072 = CARTESIAN_POINT ( 'NONE',  ( -15.19999999999998330, 12.50000000000000000, 0.3464101615137758494 ) ) ;
#11071 = CIRCLE ( 'NONE', #111131, 0.1000000000000002554 ) ;
#11073 = EDGE_CURVE ( 'NONE', #66202, #128693, #38202, .T. ) ;
#11074 = CIRCLE ( 'NONE', #617, 0.06509327318403745899 ) ;
#11075 = CONICAL_SURFACE ( 'NONE', #82206, 0.1000000000000002554, 0.003490658503988666988 ) ;
#11076 = CARTESIAN_POINT ( 'NONE',  ( 0.7999999999999553024, 12.50000000000000000, -4.330127018922201643 ) ) ;
#11077 = DIRECTION ( 'NONE',  ( -4.274815082592931898E-19, -0.9999939076577903929, -0.003490651415223739937 ) ) ;
#11078 = AXIS2_PLACEMENT_3D ( 'NONE', #28671, #9665, #68576 ) ;
#11079 = CARTESIAN_POINT ( 'NONE',  ( 186.3229166673494319, -4.445597072760092416, 7.700000000000049916 ) ) ;
#11080 = ORIENTED_EDGE ( 'NONE', *, *, #23802, .T. ) ;
#11081 = DIRECTION ( 'NONE',  ( 0.000000000000000000, 1.000000000000000000, 0.000000000000000000 ) ) ;
#11082 = CARTESIAN_POINT ( 'NONE',  ( 2.299999999999947864, 12.50000000000000000, 3.918623584224383727 ) ) ;
#11083 = AXIS2_PLACEMENT_3D ( 'NONE', #18849, #19497, #109153 ) ;
#11084 = ORIENTED_EDGE ( 'NONE', *, *, #105579, .T. ) ;
#11085 = ORIENTED_EDGE ( 'NONE', *, *, #43784, .F. ) ;
#11086 = ADVANCED_FACE ( 'NONE', ( #45161 ), #53681, .T. ) ;
#11087 = FACE_OUTER_BOUND ( 'NONE', #58184, .T. ) ;
#11089 = EDGE_CURVE ( 'NONE', #4826, #44047, #65275, .T. ) ;
#11088 = CARTESIAN_POINT ( 'NONE',  ( 15.79999999999989058, 12.50000000000000000, -2.385244779468109755E-15 ) ) ;
#11090 = FACE_BOUND ( 'NONE', #56302, .T. ) ;
#11091 = CARTESIAN_POINT ( 'NONE',  ( 15.62915144542246004, -2.500000000000000444, -5.624002559040088833 ) ) ;
#11092 = FACE_OUTER_BOUND ( 'NONE', #28171, .T. ) ;
#11094 = ORIENTED_EDGE ( 'NONE', *, *, #77282, .T. ) ;
#11093 = CONICAL_SURFACE ( 'NONE', #48687, 0.09999999999999982514, 0.003490658503988666988 ) ;
#11096 = AXIS2_PLACEMENT_3D ( 'NONE', #119708, #1229, #40539 ) ;
#11095 = DIRECTION ( 'NONE',  ( 0.000000000000000000, -0.9999939076577903929, 0.003490651415223739937 ) ) ;
#11097 = EDGE_CURVE ( 'NONE', #126294, #114390, #111322, .T. ) ;
#11098 = DIRECTION ( 'NONE',  ( -4.274815082592931898E-19, -0.9999939076577903929, -0.003490651415223739937 ) ) ;
#11099 = ORIENTED_EDGE ( 'NONE', *, *, #13287, .T. ) ;
#11100 = CARTESIAN_POINT ( 'NONE',  ( -4.150000000000024336, 2.500000000000000000, 1.472243186433545459 ) ) ;
#11101 = DIRECTION ( 'NONE',  ( 0.000000000000000000, 1.000000000000000000, 0.000000000000000000 ) ) ;
#11102 = AXIS2_PLACEMENT_3D ( 'NONE', #4277, #74983, #75608 ) ;
#11103 = VECTOR ( 'NONE', #11095, 1000.000000000000000 ) ;
#11104 = AXIS2_PLACEMENT_3D ( 'NONE', #92784, #22128, #3114 ) ;
#11105 = AXIS2_PLACEMENT_3D ( 'NONE', #78834, #97163, #99754 ) ;
#11106 = DIRECTION ( 'NONE',  ( 0.000000000000000000, 0.000000000000000000, -1.000000000000000000 ) ) ;
#11107 = CARTESIAN_POINT ( 'NONE',  ( -9.150000000000005684, 2.500000000000000000, 7.188010851410848723 ) ) ;
#11108 = CONICAL_SURFACE ( 'NONE', #44583, 0.09999999999999982514, 0.003490658503988666988 ) ;
#11110 = EDGE_LOOP ( 'NONE', ( #12604, #50491, #24644, #25817 ) ) ;
#11109 = AXIS2_PLACEMENT_3D ( 'NONE', #67872, #19410, #8304 ) ;
#11111 = CIRCLE ( 'NONE', #17367, 0.1000000000000002554 ) ;
#11112 = FACE_OUTER_BOUND ( 'NONE', #128764, .T. ) ;
#11113 = FACE_OUTER_BOUND ( 'NONE', #85102, .T. ) ;
#11114 = CARTESIAN_POINT ( 'NONE',  ( 2.899999999999945732, 2.500000000000000000, 0.09999999999999761857 ) ) ;
#11115 = VECTOR ( 'NONE', #101318, 1000.000000000000000 ) ;
#11116 = ORIENTED_EDGE ( 'NONE', *, *, #99395, .F. ) ;
#11117 = ORIENTED_EDGE ( 'NONE', *, *, #64113, .F. ) ;
#11118 = DIRECTION ( 'NONE',  ( -0.000000000000000000, -1.000000000000000000, -0.000000000000000000 ) ) ;
#11119 = AXIS2_PLACEMENT_3D ( 'NONE', #40693, #11189, #98942 ) ;
#11120 = ORIENTED_EDGE ( 'NONE', *, *, #103788, .F. ) ;
#11121 = DIRECTION ( 'NONE',  ( 0.000000000000000000, -0.9999939076577903929, 0.003490651415223739937 ) ) ;
#11122 = CARTESIAN_POINT ( 'NONE',  ( 3.749999999999978684, 2.500000000000000000, -6.495190528383302464 ) ) ;
#11123 = EDGE_CURVE ( 'NONE', #844, #126108, #3927, .T. ) ;
#11124 = DIRECTION ( 'NONE',  ( -4.274815082592931898E-19, -0.9999939076577903929, -0.003490651415223739937 ) ) ;
#11125 = ORIENTED_EDGE ( 'NONE', *, *, #127782, .T. ) ;
#11126 = DIRECTION ( 'NONE',  ( -0.000000000000000000, -1.000000000000000000, -0.000000000000000000 ) ) ;
#11127 = CARTESIAN_POINT ( 'NONE',  ( -7.950000000000012612, 2.500000000000000000, 2.165063509461097713 ) ) ;
#11128 = DIRECTION ( 'NONE',  ( -4.274815082592931898E-19, -0.9999939076577903929, -0.003490651415223739937 ) ) ;
#11129 = DIRECTION ( 'NONE',  ( 0.000000000000000000, 0.000000000000000000, 1.000000000000000000 ) ) ;
#11130 = PLANE ( 'NONE',  #77884 ) ;
#11131 = ADVANCED_FACE ( 'NONE', ( #35337 ), #10978, .T. ) ;
#11132 = CARTESIAN_POINT ( 'NONE',  ( 3.149999999999946176, 2.500000000000000000, -6.841600689897077814 ) ) ;
#11133 = EDGE_CURVE ( 'NONE', #46899, #33469, #113229, .T. ) ;
#11134 = VECTOR ( 'NONE', #65654, 1000.000000000000000 ) ;
#11135 = ORIENTED_EDGE ( 'NONE', *, *, #44217, .T. ) ;
#11136 = ORIENTED_EDGE ( 'NONE', *, *, #52627, .T. ) ;
#11137 = DIRECTION ( 'NONE',  ( 0.000000000000000000, 0.000000000000000000, -1.000000000000000000 ) ) ;
#11138 = EDGE_LOOP ( 'NONE', ( #49901, #1675 ) ) ;
#11139 = DIRECTION ( 'NONE',  ( 0.000000000000000000, 0.000000000000000000, 1.000000000000000000 ) ) ;
#11140 = EDGE_CURVE ( 'NONE', #8844, #120440, #19301, .T. ) ;
#11142 = EDGE_LOOP ( 'NONE', ( #87301, #41231, #105542, #3784 ) ) ;
#11141 = ORIENTED_EDGE ( 'NONE', *, *, #18972, .F. ) ;
#11143 = ADVANCED_FACE ( 'NONE', ( #73965 ), #84424, .T. ) ;
#11144 = EDGE_LOOP ( 'NONE', ( #23408, #72454, #100022, #39450 ) ) ;
#11145 = EDGE_CURVE ( 'NONE', #12263, #47265, #23571, .T. ) ;
#11146 = DIRECTION ( 'NONE',  ( 0.000000000000000000, 0.000000000000000000, -1.000000000000000000 ) ) ;
#11147 = ADVANCED_FACE ( 'NONE', ( #103428 ), #73779, .T. ) ;
#11148 = VECTOR ( 'NONE', #4432, 1000.000000000000000 ) ;
#11149 = CIRCLE ( 'NONE', #40427, 0.06509327318403741736 ) ;
#11150 = LINE ( 'NONE', #29520, #125860 ) ;
#11151 = AXIS2_PLACEMENT_3D ( 'NONE', #16404, #55713, #95644 ) ;
#11152 = DIRECTION ( 'NONE',  ( -0.000000000000000000, 1.000000000000000000, -0.000000000000000000 ) ) ;
#11153 =( NAMED_UNIT ( * ) PLANE_ANGLE_UNIT ( ) SI_UNIT ( $, .RADIAN. ) );
#11154 = ADVANCED_FACE ( 'NONE', ( #5848 ), #34087, .T. ) ;
#11155 = DIRECTION ( 'NONE',  ( 0.000000000000000000, -0.000000000000000000, 1.000000000000000000 ) ) ;
#11156 = PLANE ( 'NONE',  #22953 ) ;
#11157 = CARTESIAN_POINT ( 'NONE',  ( 9.349999999999916156, 12.50000000000000000, 6.148780366869520009 ) ) ;
#11158 = CARTESIAN_POINT ( 'NONE',  ( -6.900000000000015454, 2.500000000000000000, 4.676537180435972552 ) ) ;
#11159 = FACE_OUTER_BOUND ( 'NONE', #24777, .T. ) ;
#11160 = AXIS2_PLACEMENT_3D ( 'NONE', #24713, #104556, #14853 ) ;
#11162 = ADVANCED_FACE ( 'NONE', ( #122430 ), #2663, .T. ) ;
#11161 = CARTESIAN_POINT ( 'NONE',  ( -6.250000000000021316, 12.50000000000000000, -1.407149913249512663 ) ) ;
#11163 = CIRCLE ( 'NONE', #98998, 0.06509327318403745899 ) ;
#11164 = ORIENTED_EDGE ( 'NONE', *, *, #100403, .F. ) ;
#11165 = AXIS2_PLACEMENT_3D ( 'NONE', #48912, #35379, #114563 ) ;
#11166 = PLANE ( 'NONE',  #84141 ) ;
#11167 = ORIENTED_EDGE ( 'NONE', *, *, #64785, .T. ) ;
#11168 = VERTEX_POINT ( 'NONE', #72683 ) ;
#11169 = DIRECTION ( 'NONE',  ( -0.000000000000000000, 1.000000000000000000, -0.000000000000000000 ) ) ;
#11170 = CIRCLE ( 'NONE', #34466, 0.06509327318403745899 ) ;
#11171 = DIRECTION ( 'NONE',  ( 0.000000000000000000, -0.9999939076577903929, 0.003490651415223739937 ) ) ;
#11172 = CARTESIAN_POINT ( 'NONE',  ( -2.700000000000031264, 2.500000000000000000, 4.676537180435972552 ) ) ;
#11173 = DIRECTION ( 'NONE',  ( 0.000000000000000000, 0.000000000000000000, 1.000000000000000000 ) ) ;
#11174 = AXIS2_PLACEMENT_3D ( 'NONE', #101730, #41538, #4141 ) ;
#11175 = CARTESIAN_POINT ( 'NONE',  ( 187.2500000000000000, 9.429780353434619030E-16, -7.700000000000000178 ) ) ;
#11176 = AXIS2_PLACEMENT_3D ( 'NONE', #124691, #65752, #116784 ) ;
#11177 = AXIS2_PLACEMENT_3D ( 'NONE', #24685, #63312, #103246 ) ;
#11178 = DIRECTION ( 'NONE',  ( 0.000000000000000000, 1.000000000000000000, 0.000000000000000000 ) ) ;
#11179 = VERTEX_POINT ( 'NONE', #94243 ) ;
#11180 = AXIS2_PLACEMENT_3D ( 'NONE', #1611, #21923, #2924 ) ;
#11181 = ORIENTED_EDGE ( 'NONE', *, *, #35411, .F. ) ;
#11182 = CARTESIAN_POINT ( 'NONE',  ( 7.299999999999926104, 12.50000000000000000, -0.3464101615137782364 ) ) ;
#11183 = ORIENTED_EDGE ( 'NONE', *, *, #115411, .F. ) ;
#11184 = CARTESIAN_POINT ( 'NONE',  ( -14.14999999999998614, 2.500000000000000000, 1.472243186433549456 ) ) ;
#11185 = EDGE_LOOP ( 'NONE', ( #13242, #101655, #80265, #129482 ) ) ;
#11186 = VERTEX_POINT ( 'NONE', #124359 ) ;
#11187 = FACE_OUTER_BOUND ( 'NONE', #83128, .T. ) ;
#11188 = DIRECTION ( 'NONE',  ( -0.000000000000000000, 1.000000000000000000, -0.000000000000000000 ) ) ;
#11189 = DIRECTION ( 'NONE',  ( -0.000000000000000000, -1.000000000000000000, -0.000000000000000000 ) ) ;
#11190 = EDGE_CURVE ( 'NONE', #21419, #85535, #74609, .T. ) ;
#11191 = FACE_OUTER_BOUND ( 'NONE', #14004, .T. ) ;
#11192 = PLANE ( 'NONE',  #105695 ) ;
#11193 = ORIENTED_EDGE ( 'NONE', *, *, #55792, .F. ) ;
#11194 = CARTESIAN_POINT ( 'NONE',  ( -6.700000000000019718, 12.50000000000000000, -4.395220292106239768 ) ) ;
#11196 = CIRCLE ( 'NONE', #86405, 0.06509327318403745899 ) ;
#11195 = DIRECTION ( 'NONE',  ( 0.000000000000000000, 0.000000000000000000, 1.000000000000000000 ) ) ;
#11197 = VECTOR ( 'NONE', #59541, 1000.000000000000000 ) ;
#11198 = CARTESIAN_POINT ( 'NONE',  ( 14.79999999999989413, 2.500000000000000000, -0.3464101615137782364 ) ) ;
#11199 = CARTESIAN_POINT ( 'NONE',  ( -13.54999999999998828, 2.500000000000000000, -2.411473670974875638 ) ) ;
#11201 = EDGE_CURVE ( 'NONE', #30841, #91689, #42408, .T. ) ;
#11200 = PLANE ( 'NONE',  #14329 ) ;
#11202 = EDGE_LOOP ( 'NONE', ( #124036, #68654 ) ) ;
#11203 = AXIS2_PLACEMENT_3D ( 'NONE', #99788, #121346, #270 ) ;
#11204 = AXIS2_PLACEMENT_3D ( 'NONE', #60319, #19738, #59680 ) ;
#11205 = VECTOR ( 'NONE', #100613, 1000.000000000000000 ) ;
#11206 = ORIENTED_EDGE ( 'NONE', *, *, #108351, .F. ) ;
#11207 = AXIS2_PLACEMENT_3D ( 'NONE', #128037, #78309, #48186 ) ;
#11208 = EDGE_LOOP ( 'NONE', ( #44989, #6325, #121739, #15666 ) ) ;
#11209 = CARTESIAN_POINT ( 'NONE',  ( -14.14999999999998792, 12.50000000000000000, 2.857883832488652853 ) ) ;
#11210 = ORIENTED_EDGE ( 'NONE', *, *, #704, .T. ) ;
#11211 = CARTESIAN_POINT ( 'NONE',  ( 17.49101023696819368, -2.144674160806593566, 4.220798295113220355 ) ) ;
#11212 = DIRECTION ( 'NONE',  ( -0.000000000000000000, -1.000000000000000000, -0.000000000000000000 ) ) ;
#11213 = AXIS2_PLACEMENT_3D ( 'NONE', #111326, #22346, #122475 ) ;
#11214 = AXIS2_PLACEMENT_3D ( 'NONE', #112961, #1069, #23283 ) ;
#11215 = AXIS2_PLACEMENT_3D ( 'NONE', #44103, #84020, #123946 ) ;
#11216 = AXIS2_PLACEMENT_3D ( 'NONE', #56883, #117741, #77200 ) ;
#11217 = ORIENTED_EDGE ( 'NONE', *, *, #37332, .F. ) ;
#11218 = DIRECTION ( 'NONE',  ( 0.000000000000000000, 1.000000000000000000, 0.000000000000000000 ) ) ;
#11219 = DIRECTION ( 'NONE',  ( 0.000000000000000000, 0.000000000000000000, -1.000000000000000000 ) ) ;
#11220 = CARTESIAN_POINT ( 'NONE',  ( 12.29999999999990123, 2.500000000000000000, 0.2464101615137735679 ) ) ;
#11221 = DIRECTION ( 'NONE',  ( 0.000000000000000000, 1.000000000000000000, 0.000000000000000000 ) ) ;
#11222 = VERTEX_POINT ( 'NONE', #96169 ) ;
#11223 = VERTEX_POINT ( 'NONE', #86999 ) ;
#11224 = FACE_OUTER_BOUND ( 'NONE', #117702, .T. ) ;
#11225 = LINE ( 'NONE', #51181, #35191 ) ;
#11226 = DIRECTION ( 'NONE',  ( 0.000000000000000000, 1.000000000000000000, 0.000000000000000000 ) ) ;
#11227 = DIRECTION ( 'NONE',  ( 0.000000000000000000, 0.000000000000000000, 1.000000000000000000 ) ) ;
#11228 = ADVANCED_FACE ( 'NONE', ( #68003 ), #76545, .T. ) ;
#11229 = ORIENTED_EDGE ( 'NONE', *, *, #76511, .T. ) ;
#11230 = VERTEX_POINT ( 'NONE', #107285 ) ;
#11231 = DIRECTION ( 'NONE',  ( -0.000000000000000000, 1.000000000000000000, -0.000000000000000000 ) ) ;
#11232 = CARTESIAN_POINT ( 'NONE',  ( -8.350000000000013856, 12.50000000000000000, -2.230156782645139391 ) ) ;
#11233 = LINE ( 'NONE', #1420, #83177 ) ;
#11234 = AXIS2_PLACEMENT_3D ( 'NONE', #42982, #103156, #33143 ) ;
#11235 = ORIENTED_EDGE ( 'NONE', *, *, #81186, .T. ) ;
#11236 = AXIS2_PLACEMENT_3D ( 'NONE', #89193, #127201, #97719 ) ;
#11237 = EDGE_CURVE ( 'NONE', #740, #128936, #61281, .T. ) ;
#11238 = AXIS2_PLACEMENT_3D ( 'NONE', #77561, #121197, #31538 ) ;
#11239 = DIRECTION ( 'NONE',  ( 0.000000000000000000, 1.000000000000000000, 0.000000000000000000 ) ) ;
#11240 = DIRECTION ( 'NONE',  ( 0.000000000000000000, 1.000000000000000000, 0.000000000000000000 ) ) ;
#11241 = VERTEX_POINT ( 'NONE', #97469 ) ;
#11242 = ADVANCED_FACE ( 'NONE', ( #46425 ), #126940, .T. ) ;
#11243 = CARTESIAN_POINT ( 'NONE',  ( 11.84999999999990727, 2.500000000000000000, 6.941600689897073018 ) ) ;
#11244 = VECTOR ( 'NONE', #51522, 1000.000000000000000 ) ;
#11245 = EDGE_CURVE ( 'NONE', #65955, #103176, #16933, .T. ) ;
#11246 = ORIENTED_EDGE ( 'NONE', *, *, #86637, .T. ) ;
#11247 = LINE ( 'NONE', #120571, #83028 ) ;
#11248 = VECTOR ( 'NONE', #93265, 1000.000000000000000 ) ;
#11249 = ORIENTED_EDGE ( 'NONE', *, *, #101917, .T. ) ;
#11250 = AXIS2_PLACEMENT_3D ( 'NONE', #106368, #118770, #16037 ) ;
#11251 = ORIENTED_EDGE ( 'NONE', *, *, #14084, .T. ) ;
#11252 = CARTESIAN_POINT ( 'NONE',  ( 12.89999999999989910, 12.50000000000000000, 0.6928203230275494784 ) ) ;
#11253 = DIRECTION ( 'NONE',  ( 0.000000000000000000, 0.000000000000000000, -1.000000000000000000 ) ) ;
#11254 = ADVANCED_FACE ( 'NONE', ( #17608 ), #77186, .T. ) ;
#11255 = ORIENTED_EDGE ( 'NONE', *, *, #57398, .T. ) ;
#11256 = ORIENTED_EDGE ( 'NONE', *, *, #6340, .T. ) ;
#11257 = ADVANCED_FACE ( 'NONE', ( #67327 ), #75830, .T. ) ;
#11258 = AXIS2_PLACEMENT_3D ( 'NONE', #39027, #88058, #38365 ) ;
#11259 = CARTESIAN_POINT ( 'NONE',  ( -6.850000000000013856, 2.500000000000000000, 6.148780366869520897 ) ) ;
#11260 = CARTESIAN_POINT ( 'NONE',  ( -9.800000000000006040, 12.50000000000000000, 0.2813168883297361700 ) ) ;
#11261 = EDGE_LOOP ( 'NONE', ( #84158, #81235, #83157, #38821 ) ) ;
#11262 = CARTESIAN_POINT ( 'NONE',  ( -0.2000000000000339284, 12.50000000000000000, -0.2813168883297385570 ) ) ;
#11263 = CARTESIAN_POINT ( 'NONE',  ( 185.4427083336747160, -6.551208109652278289, 3.782341765624995134 ) ) ;
#11264 = VECTOR ( 'NONE', #57786, 1000.000000000000000 ) ;
#11266 = VECTOR ( 'NONE', #29483, 1000.000000000000000 ) ;
#11265 = CARTESIAN_POINT ( 'NONE',  ( 0.3999999999999563904, 12.50000000000000000, 5.022947341949748790 ) ) ;
#11267 = AXIS2_PLACEMENT_3D ( 'NONE', #31147, #81521, #90689 ) ;
#11268 = LINE ( 'NONE', #21089, #103664 ) ;
#11269 = CARTESIAN_POINT ( 'NONE',  ( 1.449999999999952660, 12.50000000000000000, -6.841600689897078702 ) ) ;
#11270 = CARTESIAN_POINT ( 'NONE',  ( -8.550000000000009592, 2.500000000000000000, 6.741600689897071952 ) ) ;
#11271 = CONICAL_SURFACE ( 'NONE', #809, 0.09999999999999982514, 0.003490658503988666988 ) ;
#11272 = CARTESIAN_POINT ( 'NONE',  ( -9.800000000000007816, 2.500000000000000000, -3.883716857408422207 ) ) ;
#11273 = AXIS2_PLACEMENT_3D ( 'NONE', #57145, #29614, #48620 ) ;
#11274 = ORIENTED_EDGE ( 'NONE', *, *, #64235, .F. ) ;
#11275 = ORIENTED_EDGE ( 'NONE', *, *, #103759, .T. ) ;
#11276 = DIRECTION ( 'NONE',  ( 0.000000000000000000, 1.000000000000000000, 0.000000000000000000 ) ) ;
#11277 = ORIENTED_EDGE ( 'NONE', *, *, #118917, .F. ) ;
#11278 = CARTESIAN_POINT ( 'NONE',  ( 6.649999999999930189, 2.500000000000000000, 5.702370205355745014 ) ) ;
#11279 = DIRECTION ( 'NONE',  ( 0.000000000000000000, 0.000000000000000000, -1.000000000000000000 ) ) ;
#11280 = DIRECTION ( 'NONE',  ( 0.000000000000000000, 0.000000000000000000, -1.000000000000000000 ) ) ;
#11282 = ORIENTED_EDGE ( 'NONE', *, *, #121633, .T. ) ;
#11281 = ORIENTED_EDGE ( 'NONE', *, *, #113984, .F. ) ;
#11283 = FACE_BOUND ( 'NONE', #118572, .T. ) ;
#11284 = ORIENTED_EDGE ( 'NONE', *, *, #92391, .F. ) ;
#11285 = DIRECTION ( 'NONE',  ( 0.000000000000000000, 0.000000000000000000, -1.000000000000000000 ) ) ;
#11286 = CARTESIAN_POINT ( 'NONE',  ( 14.19999999999989626, 2.500000000000000000, -2.276824562219559311E-15 ) ) ;
#11287 = DIRECTION ( 'NONE',  ( 0.000000000000000000, 1.000000000000000000, 0.000000000000000000 ) ) ;
#11288 = DIRECTION ( 'NONE',  ( 0.000000000000000000, 0.000000000000000000, 1.000000000000000000 ) ) ;
#11289 = CARTESIAN_POINT ( 'NONE',  ( 6.649999999999930189, 2.500000000000000000, -2.757883832488654097 ) ) ;
#11290 = DIRECTION ( 'NONE',  ( -0.000000000000000000, 1.000000000000000000, -0.000000000000000000 ) ) ;
#11291 = CIRCLE ( 'NONE', #59643, 0.06509327318403745899 ) ;
#11292 = FACE_OUTER_BOUND ( 'NONE', #10043, .T. ) ;
#11293 = CARTESIAN_POINT ( 'NONE',  ( 10.39999999999991509, 12.50000000000000000, -0.6928203230275542523 ) ) ;
#11294 = AXIS2_PLACEMENT_3D ( 'NONE', #5690, #56710, #46266 ) ;
#11295 = CIRCLE ( 'NONE', #7071, 0.09999999999999982514 ) ;
#11296 = DIRECTION ( 'NONE',  ( -0.000000000000000000, 1.000000000000000000, -0.000000000000000000 ) ) ;
#11297 = LINE ( 'NONE', #91157, #77793 ) ;
#11298 = DIRECTION ( 'NONE',  ( -0.000000000000000000, 1.000000000000000000, -0.000000000000000000 ) ) ;
#11299 = ADVANCED_FACE ( 'NONE', ( #56873 ), #113489, .T. ) ;
#11300 = AXIS2_PLACEMENT_3D ( 'NONE', #25084, #33623, #53906 ) ;
#11302 = ORIENTED_EDGE ( 'NONE', *, *, #10504, .F. ) ;
#11301 = CIRCLE ( 'NONE', #84470, 0.06509327318403745899 ) ;
#11303 = VERTEX_POINT ( 'NONE', #56249 ) ;
#11304 = VERTEX_POINT ( 'NONE', #86345 ) ;
#11305 = ORIENTED_EDGE ( 'NONE', *, *, #67516, .F. ) ;
#11307 = CIRCLE ( 'NONE', #103256, 0.06509327318403745899 ) ;
#11306 = DIRECTION ( 'NONE',  ( 0.000000000000000000, 0.000000000000000000, 1.000000000000000000 ) ) ;
#11308 = EDGE_CURVE ( 'NONE', #5250, #9738, #87636, .T. ) ;
#11309 = LINE ( 'NONE', #79426, #54953 ) ;
#11310 = EDGE_CURVE ( 'NONE', #121502, #107629, #63321, .T. ) ;
#11312 = EDGE_LOOP ( 'NONE', ( #83722, #109539, #125198, #20072 ) ) ;
#11311 = VERTEX_POINT ( 'NONE', #37902 ) ;
#11313 = ORIENTED_EDGE ( 'NONE', *, *, #20040, .T. ) ;
#11314 = EDGE_CURVE ( 'NONE', #6379, #101677, #8429, .T. ) ;
#11315 = CARTESIAN_POINT ( 'NONE',  ( -8.300000000000011369, 2.500000000000000000, 0.09999999999999772959 ) ) ;
#11316 = EDGE_CURVE ( 'NONE', #45963, #14446, #92566, .T. ) ;
#11317 = AXIS2_PLACEMENT_3D ( 'NONE', #5733, #26045, #33925 ) ;
#11318 = AXIS2_PLACEMENT_3D ( 'NONE', #9186, #49779, #89040 ) ;
#11319 = DIRECTION ( 'NONE',  ( -0.000000000000000000, -1.000000000000000000, -0.000000000000000000 ) ) ;
#11320 = DIRECTION ( 'NONE',  ( 0.000000000000000000, 1.000000000000000000, 0.000000000000000000 ) ) ;
#11321 = FACE_OUTER_BOUND ( 'NONE', #56669, .T. ) ;
#11322 = EDGE_CURVE ( 'NONE', #85535, #116043, #80053, .T. ) ;
#11323 = CARTESIAN_POINT ( 'NONE',  ( 9.399999999999915090, 12.50000000000000000, -4.676537180435977881 ) ) ;
#11324 = CARTESIAN_POINT ( 'NONE',  ( 13.09999999999990195, 12.50000000000000000, 3.983716857408420076 ) ) ;
#11325 = CONICAL_SURFACE ( 'NONE', #15512, 0.09999999999999982514, 0.003490658503988666988 ) ;
#11326 = DIRECTION ( 'NONE',  ( -0.000000000000000000, -1.000000000000000000, -0.000000000000000000 ) ) ;
#11327 = ORIENTED_EDGE ( 'NONE', *, *, #28612, .T. ) ;
#11329 = EDGE_CURVE ( 'NONE', #119031, #47664, #38577, .T. ) ;
#11328 = DIRECTION ( 'NONE',  ( 0.000000000000000000, 0.000000000000000000, 1.000000000000000000 ) ) ;
#11330 = EDGE_LOOP ( 'NONE', ( #42515, #105357, #107392, #75808 ) ) ;
#11331 = EDGE_CURVE ( 'NONE', #27897, #24765, #84240, .T. ) ;
#11332 = VERTEX_POINT ( 'NONE', #35973 ) ;
#11333 = ORIENTED_EDGE ( 'NONE', *, *, #46921, .F. ) ;
#11334 = AXIS2_PLACEMENT_3D ( 'NONE', #43383, #11326, #121926 ) ;
#11335 = CARTESIAN_POINT ( 'NONE',  ( -3.749999999999991562, 2.500000000000000000, 6.395190528383296602 ) ) ;
#11336 = ORIENTED_EDGE ( 'NONE', *, *, #37041, .T. ) ;
#11337 = ORIENTED_EDGE ( 'NONE', *, *, #69954, .F. ) ;
#11338 = ORIENTED_EDGE ( 'NONE', *, *, #82769, .F. ) ;
#11339 = AXIS2_PLACEMENT_3D ( 'NONE', #37973, #30114, #100127 ) ;
#11340 = DIRECTION ( 'NONE',  ( 0.000000000000000000, 1.000000000000000000, 0.000000000000000000 ) ) ;
#11341 = DIRECTION ( 'NONE',  ( 0.000000000000000000, 1.000000000000000000, 0.000000000000000000 ) ) ;
#11342 = DIRECTION ( 'NONE',  ( 0.000000000000000000, 1.000000000000000000, 0.000000000000000000 ) ) ;
#11343 = FACE_OUTER_BOUND ( 'NONE', #31713, .T. ) ;
#11344 = DIRECTION ( 'NONE',  ( 0.000000000000000000, 0.000000000000000000, 1.000000000000000000 ) ) ;
#11345 = CARTESIAN_POINT ( 'NONE',  ( -14.14999999999998792, 2.500000000000000000, -1.472243186433547901 ) ) ;
#11346 = CARTESIAN_POINT ( 'NONE',  ( -2.500000000000030642, 2.500000000000000000, -4.922947341949753586 ) ) ;
#11347 = AXIS2_PLACEMENT_3D ( 'NONE', #17030, #56980, #96915 ) ;
#11348 = CONICAL_SURFACE ( 'NONE', #9191, 0.1000000000000002554, 0.003490658503988666988 ) ;
#11349 = ORIENTED_EDGE ( 'NONE', *, *, #24118, .F. ) ;
#11350 = CARTESIAN_POINT ( 'NONE',  ( 127.5000000000000000, 5.000000000000000000, -4.999999999999998224 ) ) ;
#11351 = ORIENTED_EDGE ( 'NONE', *, *, #107308, .F. ) ;
#11352 = CARTESIAN_POINT ( 'NONE',  ( 10.44999999999991047, 2.500000000000000000, -6.495190528383302464 ) ) ;
#11353 = DIRECTION ( 'NONE',  ( -0.000000000000000000, -1.000000000000000000, -0.000000000000000000 ) ) ;
#11354 = ORIENTED_EDGE ( 'NONE', *, *, #112253, .F. ) ;
#11355 = DIRECTION ( 'NONE',  ( 0.000000000000000000, 0.000000000000000000, 1.000000000000000000 ) ) ;
#11356 = LINE ( 'NONE', #91208, #77052 ) ;
#11357 = EDGE_LOOP ( 'NONE', ( #81779, #83728 ) ) ;
#11358 = AXIS2_PLACEMENT_3D ( 'NONE', #76912, #96528, #16673 ) ;
#11359 = DIRECTION ( 'NONE',  ( 0.000000000000000000, 1.000000000000000000, 0.000000000000000000 ) ) ;
#11360 = ORIENTED_EDGE ( 'NONE', *, *, #12512, .F. ) ;
#11361 = ORIENTED_EDGE ( 'NONE', *, *, #6494, .F. ) ;
#11362 = DIRECTION ( 'NONE',  ( 0.000000000000000000, 1.000000000000000000, 0.000000000000000000 ) ) ;
#11363 = DIRECTION ( 'NONE',  ( 0.000000000000000000, -0.9999939076577903929, 0.003490651415223739937 ) ) ;
#11364 = DIRECTION ( 'NONE',  ( 0.000000000000000000, 1.000000000000000000, 0.000000000000000000 ) ) ;
#11365 = DIRECTION ( 'NONE',  ( 0.000000000000000000, 1.000000000000000000, 0.000000000000000000 ) ) ;
#11367 = EDGE_CURVE ( 'NONE', #41239, #128359, #11074, .T. ) ;
#11366 = CARTESIAN_POINT ( 'NONE',  ( 162.5000000000000000, 0.5000000000000000000, -7.500000000000005329 ) ) ;
#11368 = VERTEX_POINT ( 'NONE', #52087 ) ;
#11369 = CIRCLE ( 'NONE', #92857, 0.1000000000000000472 ) ;
#11370 = LINE ( 'NONE', #72246, #61316 ) ;
#11371 = AXIS2_PLACEMENT_3D ( 'NONE', #95647, #104800, #85812 ) ;
#11372 = VERTEX_POINT ( 'NONE', #83487 ) ;
#11373 = PLANE ( 'NONE',  #75820 ) ;
#11374 = DIRECTION ( 'NONE',  ( 0.000000000000000000, 0.000000000000000000, 1.000000000000000000 ) ) ;
#11375 = CARTESIAN_POINT ( 'NONE',  ( 186.5052083336747444, -6.551208109652278289, 3.782341765624995134 ) ) ;
#11376 = DIRECTION ( 'NONE',  ( 0.000000000000000000, -0.9999939076577903929, 0.003490651415223739937 ) ) ;
#11377 = CARTESIAN_POINT ( 'NONE',  ( 6.049999999999934097, 2.500000000000000000, -2.411473670974877859 ) ) ;
#11378 = CARTESIAN_POINT ( 'NONE',  ( -8.750000000000005329, 2.500000000000000000, 5.802370205355744659 ) ) ;
#11379 = CARTESIAN_POINT ( 'NONE',  ( -6.450000000000019718, 12.50000000000000000, -1.818653347947326138 ) ) ;
#11380 = ORIENTED_EDGE ( 'NONE', *, *, #21604, .T. ) ;
#11381 = CARTESIAN_POINT ( 'NONE',  ( 184.2500000000000000, 9.429780353434619030E-16, -7.700000000000000178 ) ) ;
#11383 = DIRECTION ( 'NONE',  ( -0.000000000000000000, 1.000000000000000000, -0.000000000000000000 ) ) ;
#11382 = CIRCLE ( 'NONE', #44851, 0.06509327318403745899 ) ;
#11384 = DIRECTION ( 'NONE',  ( 0.000000000000000000, 1.000000000000000000, 0.000000000000000000 ) ) ;
#11385 = CONICAL_SURFACE ( 'NONE', #61490, 0.1000000000000002554, 0.003490658503988666988 ) ;
#11386 = AXIS2_PLACEMENT_3D ( 'NONE', #42931, #90711, #72375 ) ;
#11387 = AXIS2_PLACEMENT_3D ( 'NONE', #81011, #69903, #60730 ) ;
#11388 = ORIENTED_EDGE ( 'NONE', *, *, #125283, .F. ) ;
#11389 = DIRECTION ( 'NONE',  ( 0.000000000000000000, 0.000000000000000000, -1.000000000000000000 ) ) ;
#11390 = VECTOR ( 'NONE', #49671, 1000.000000000000000 ) ;
#11391 = AXIS2_PLACEMENT_3D ( 'NONE', #39339, #38020, #19676 ) ;
#11392 = EDGE_LOOP ( 'NONE', ( #76262, #36804 ) ) ;
#11393 = CIRCLE ( 'NONE', #80369, 0.09999999999999982514 ) ;
#11394 = EDGE_LOOP ( 'NONE', ( #54022, #22723, #25974, #80907 ) ) ;
#11395 = LINE ( 'NONE', #51350, #55132 ) ;
#11396 = ORIENTED_EDGE ( 'NONE', *, *, #79481, .F. ) ;
#11397 = CARTESIAN_POINT ( 'NONE',  ( -4.350000000000023626, 12.50000000000000000, 6.906693963081109722 ) ) ;
#11398 = CARTESIAN_POINT ( 'NONE',  ( 3.949999999999938893, 2.500000000000000000, 6.148780366869520009 ) ) ;
#11399 = CARTESIAN_POINT ( 'NONE',  ( 8.549999999999918998, 2.500000000000000000, 6.841600689897072485 ) ) ;
#11400 = ORIENTED_EDGE ( 'NONE', *, *, #47219, .T. ) ;
#11401 = AXIS2_PLACEMENT_3D ( 'NONE', #48376, #37280, #26803 ) ;
#11403 = EDGE_CURVE ( 'NONE', #125479, #15328, #63838, .T. ) ;
#11402 = VECTOR ( 'NONE', #11759, 1000.000000000000000 ) ;
#11404 = DIRECTION ( 'NONE',  ( -0.000000000000000000, -1.000000000000000000, -0.000000000000000000 ) ) ;
#11405 = CARTESIAN_POINT ( 'NONE',  ( 1.649999999999949729, 12.50000000000000000, 5.737276932171707422 ) ) ;
#11406 = EDGE_CURVE ( 'NONE', #75500, #124247, #111427, .T. ) ;
#11407 = EDGE_CURVE ( 'NONE', #74772, #59434, #36145, .T. ) ;
#11408 = VERTEX_POINT ( 'NONE', #2309 ) ;
#11409 = ORIENTED_EDGE ( 'NONE', *, *, #3712, .F. ) ;
#11410 = EDGE_LOOP ( 'NONE', ( #122507, #33811 ) ) ;
#11411 = DIRECTION ( 'NONE',  ( -0.000000000000000000, -1.000000000000000000, -0.000000000000000000 ) ) ;
#11412 = CARTESIAN_POINT ( 'NONE',  ( 183.9895833340160607, -4.445597072760187451, -7.699999999999876721 ) ) ;
#11413 = ADVANCED_FACE ( 'NONE', ( #82845 ), #72376, .T. ) ;
#11414 = EDGE_CURVE ( 'NONE', #28130, #91712, #59134, .T. ) ;
#11415 = DIRECTION ( 'NONE',  ( -0.000000000000000000, -1.000000000000000000, -0.000000000000000000 ) ) ;
#11416 = EDGE_CURVE ( 'NONE', #16149, #29869, #23247, .T. ) ;
#11417 = FACE_BOUND ( 'NONE', #27345, .T. ) ;
#11419 = EDGE_CURVE ( 'NONE', #78711, #75943, #41641, .T. ) ;
#11418 = ORIENTED_EDGE ( 'NONE', *, *, #13818, .T. ) ;
#11420 = EDGE_CURVE ( 'NONE', #52365, #119493, #12776, .T. ) ;
#11421 = DIRECTION ( 'NONE',  ( 0.000000000000000000, 0.000000000000000000, -1.000000000000000000 ) ) ;
#11422 = CARTESIAN_POINT ( 'NONE',  ( 14.14999999999989733, 2.500000000000000000, 2.857883832488649301 ) ) ;
#11423 = AXIS2_PLACEMENT_3D ( 'NONE', #80911, #53228, #58689 ) ;
#11424 = ORIENTED_EDGE ( 'NONE', *, *, #50622, .F. ) ;
#11425 = PLANE ( 'NONE',  #57197 ) ;
#11426 = DIRECTION ( 'NONE',  ( 0.000000000000000000, 1.000000000000000000, 0.000000000000000000 ) ) ;
#11427 = CARTESIAN_POINT ( 'NONE',  ( -11.69999999999999929, 12.50000000000000000, 1.734723475976807094E-15 ) ) ;
#11428 = DIRECTION ( 'NONE',  ( 0.000000000000000000, 0.000000000000000000, -1.000000000000000000 ) ) ;
#11429 = DIRECTION ( 'NONE',  ( -4.274815082592931898E-19, -0.9999939076577903929, -0.003490651415223739937 ) ) ;
#11430 = EDGE_CURVE ( 'NONE', #126385, #119822, #71740, .T. ) ;
#11431 = DIRECTION ( 'NONE',  ( 0.000000000000000000, -0.9999939076577903929, 0.003490651415223739937 ) ) ;
#11432 = DIRECTION ( 'NONE',  ( -0.000000000000000000, -1.000000000000000000, -0.000000000000000000 ) ) ;
#11433 = AXIS2_PLACEMENT_3D ( 'NONE', #121546, #122853, #51550 ) ;
#11434 = CONICAL_SURFACE ( 'NONE', #84603, 0.1000000000000000056, 0.003490658503988666988 ) ;
#11435 = ORIENTED_EDGE ( 'NONE', *, *, #120967, .F. ) ;
#11436 = ORIENTED_EDGE ( 'NONE', *, *, #109832, .T. ) ;
#11437 = VERTEX_POINT ( 'NONE', #113577 ) ;
#11438 = EDGE_LOOP ( 'NONE', ( #100150, #46702 ) ) ;
#11439 = DIRECTION ( 'NONE',  ( 0.000000000000000000, -0.000000000000000000, 1.000000000000000000 ) ) ;
#11440 = DIRECTION ( 'NONE',  ( 0.000000000000000000, -0.9999939076577903929, 0.003490651415223739937 ) ) ;
#11441 = ORIENTED_EDGE ( 'NONE', *, *, #54994, .F. ) ;
#11442 = FACE_BOUND ( 'NONE', #84999, .T. ) ;
#11443 = DIRECTION ( 'NONE',  ( 0.000000000000000000, -0.000000000000000000, 1.000000000000000000 ) ) ;
#11444 = DIRECTION ( 'NONE',  ( 0.000000000000000000, 0.000000000000000000, 1.000000000000000000 ) ) ;
#11445 = CIRCLE ( 'NONE', #44906, 0.06509327318403745899 ) ;
#11446 = DIRECTION ( 'NONE',  ( -0.000000000000000000, -1.000000000000000000, -0.000000000000000000 ) ) ;
#11447 = DIRECTION ( 'NONE',  ( 0.000000000000000000, 0.000000000000000000, 1.000000000000000000 ) ) ;
#11448 = AXIS2_PLACEMENT_3D ( 'NONE', #47840, #49135, #10467 ) ;
#11449 = CARTESIAN_POINT ( 'NONE',  ( -4.150000000000027889, 12.50000000000000000, -7.122917578226816815 ) ) ;
#11450 = DIRECTION ( 'NONE',  ( 0.000000000000000000, -0.000000000000000000, 1.000000000000000000 ) ) ;
#11451 = LINE ( 'NONE', #120766, #53829 ) ;
#11452 = CARTESIAN_POINT ( 'NONE',  ( -1.450000000000035927, 2.500000000000000000, -6.048780366869526581 ) ) ;
#11453 = DIRECTION ( 'NONE',  ( -4.274815082592931898E-19, -0.9999939076577903929, -0.003490651415223739937 ) ) ;
#11454 = ORIENTED_EDGE ( 'NONE', *, *, #121383, .T. ) ;
#11455 = EDGE_LOOP ( 'NONE', ( #35355, #87114 ) ) ;
#11456 = AXIS2_PLACEMENT_3D ( 'NONE', #28820, #68078, #108650 ) ;
#11457 = ORIENTED_EDGE ( 'NONE', *, *, #110973, .T. ) ;
#11458 = VERTEX_POINT ( 'NONE', #88945 ) ;
#11459 = AXIS2_PLACEMENT_3D ( 'NONE', #88044, #39652, #68430 ) ;
#11460 = VERTEX_POINT ( 'NONE', #53377 ) ;
#11461 = EDGE_LOOP ( 'NONE', ( #65054, #48773, #28101, #102716 ) ) ;
#11462 = CARTESIAN_POINT ( 'NONE',  ( -7.700000000000012612, 2.500000000000000000, 4.576537180435972019 ) ) ;
#11463 = EDGE_CURVE ( 'NONE', #65404, #126067, #71638, .T. ) ;
#11464 = VERTEX_POINT ( 'NONE', #49038 ) ;
#11465 = EDGE_CURVE ( 'NONE', #10941, #44142, #93291, .T. ) ;
#11466 = CONICAL_SURFACE ( 'NONE', #88742, 0.09999999999999999167, 0.003490658503988666988 ) ;
#11467 = ADVANCED_FACE ( 'NONE', ( #2982 ), #43565, .T. ) ;
#11468 = CARTESIAN_POINT ( 'NONE',  ( 16.70850060796067993, 0.4765610498145415042, 5.930927070179838445 ) ) ;
#11469 = PLANE ( 'NONE',  #122789 ) ;
#11470 = DIRECTION ( 'NONE',  ( -0.000000000000000000, -1.000000000000000000, -0.000000000000000000 ) ) ;
#11471 = DIRECTION ( 'NONE',  ( 0.000000000000000000, 0.000000000000000000, 1.000000000000000000 ) ) ;
#11472 = ADVANCED_FACE ( 'NONE', ( #62555 ), #82103, .T. ) ;
#11473 = ORIENTED_EDGE ( 'NONE', *, *, #68314, .F. ) ;
#11474 = LINE ( 'NONE', #112268, #8783 ) ;
#11475 = ADVANCED_FACE ( 'NONE', ( #23916 ), #13127, .T. ) ;
#11476 = EDGE_CURVE ( 'NONE', #67419, #82776, #89588, .T. ) ;
#11477 = ORIENTED_EDGE ( 'NONE', *, *, #24456, .F. ) ;
#11478 = EDGE_CURVE ( 'NONE', #80386, #99444, #109288, .T. ) ;
#11480 = ORIENTED_EDGE ( 'NONE', *, *, #108097, .F. ) ;
#11479 = CONICAL_SURFACE ( 'NONE', #99227, 0.1000000000000002554, 0.003490658503988666988 ) ;
#11481 = CARTESIAN_POINT ( 'NONE',  ( 108.0000000000000142, 9.000000000000001776, 4.500000000000003553 ) ) ;
#11482 = AXIS2_PLACEMENT_3D ( 'NONE', #102480, #71086, #121459 ) ;
#11483 = DIRECTION ( 'NONE',  ( 0.000000000000000000, 1.000000000000000000, 0.000000000000000000 ) ) ;
#11484 = AXIS2_PLACEMENT_3D ( 'NONE', #99862, #102900, #9544 ) ;
#11485 = DIRECTION ( 'NONE',  ( -0.000000000000000000, -1.000000000000000000, -0.000000000000000000 ) ) ;
#11486 = ORIENTED_EDGE ( 'NONE', *, *, #44884, .T. ) ;
#11487 = EDGE_CURVE ( 'NONE', #24791, #45310, #126001, .T. ) ;
#11488 = ORIENTED_EDGE ( 'NONE', *, *, #17164, .F. ) ;
#11489 = CARTESIAN_POINT ( 'NONE',  ( -1.050000000000037348, 2.500000000000000000, -2.511473670974877948 ) ) ;
#11490 = CIRCLE ( 'NONE', #59639, 0.06509327318403745899 ) ;
#11491 = AXIS2_PLACEMENT_3D ( 'NONE', #47053, #86963, #24185 ) ;
#11492 = CONICAL_SURFACE ( 'NONE', #128600, 0.1000000000000002554, 0.003490658503988666988 ) ;
#11493 = LINE ( 'NONE', #51438, #118509 ) ;
#11494 = DIRECTION ( 'NONE',  ( 0.000000000000000000, -0.000000000000000000, -1.000000000000000000 ) ) ;
#11495 = DIRECTION ( 'NONE',  ( -0.000000000000000000, -1.000000000000000000, -0.000000000000000000 ) ) ;
#11496 = EDGE_LOOP ( 'NONE', ( #112391, #101191, #55332, #68630 ) ) ;
#11497 = CIRCLE ( 'NONE', #36654, 0.1000000000000002554 ) ;
#11498 = CARTESIAN_POINT ( 'NONE',  ( -10.85000000000000142, 2.500000000000000000, 6.595190528383296780 ) ) ;
#11499 = ORIENTED_EDGE ( 'NONE', *, *, #94951, .T. ) ;
#11500 = LINE ( 'NONE', #22629, #59452 ) ;
#11501 = AXIS2_PLACEMENT_3D ( 'NONE', #42209, #82787, #103707 ) ;
#11502 = EDGE_LOOP ( 'NONE', ( #87579, #70359, #27440, #63042 ) ) ;
#11503 = FACE_OUTER_BOUND ( 'NONE', #5142, .T. ) ;
#11504 = LINE ( 'NONE', #110970, #10794 ) ;
#11505 = CARTESIAN_POINT ( 'NONE',  ( -10.40000000000000213, 2.500000000000000000, 4.922947341949748257 ) ) ;
#11506 = AXIS2_PLACEMENT_3D ( 'NONE', #20707, #41016, #98592 ) ;
#11507 = EDGE_CURVE ( 'NONE', #37844, #93665, #65459, .T. ) ;
#11508 = DIRECTION ( 'NONE',  ( 0.000000000000000000, 0.000000000000000000, -1.000000000000000000 ) ) ;
#11509 = VERTEX_POINT ( 'NONE', #46779 ) ;
#11510 = CARTESIAN_POINT ( 'NONE',  ( -3.950000000000026379, 2.500000000000000000, 6.741600689897071952 ) ) ;
#11511 = DIRECTION ( 'NONE',  ( 0.000000000000000000, 1.000000000000000000, 0.000000000000000000 ) ) ;
#11512 = VERTEX_POINT ( 'NONE', #27133 ) ;
#11513 = VERTEX_POINT ( 'NONE', #75573 ) ;
#11514 = EDGE_LOOP ( 'NONE', ( #73506, #37314, #64802, #114939 ) ) ;
#11515 = CARTESIAN_POINT ( 'NONE',  ( 17.50000000000000000, 2.750000000000000000, 2.864912725862981624 ) ) ;
#11516 = DIRECTION ( 'NONE',  ( -0.000000000000000000, -1.000000000000000000, -0.000000000000000000 ) ) ;
#11517 = SURFACE_STYLE_FILL_AREA ( #60003 ) ;
#11518 = AXIS2_PLACEMENT_3D ( 'NONE', #119956, #51235, #121241 ) ;
#11519 = CARTESIAN_POINT ( 'NONE',  ( 12.89999999999990266, 12.50000000000000000, 3.572213422710607489 ) ) ;
#11520 = DIRECTION ( 'NONE',  ( -0.000000000000000000, 1.000000000000000000, -0.000000000000000000 ) ) ;
#11522 = EDGE_CURVE ( 'NONE', #59844, #74070, #103127, .T. ) ;
#11521 = DIRECTION ( 'NONE',  ( 0.000000000000000000, 0.000000000000000000, -1.000000000000000000 ) ) ;
#11523 = DIRECTION ( 'NONE',  ( -0.000000000000000000, 1.000000000000000000, -0.000000000000000000 ) ) ;
#11524 = DIRECTION ( 'NONE',  ( 0.000000000000000000, -0.000000000000000000, 1.000000000000000000 ) ) ;
#11525 = CONICAL_SURFACE ( 'NONE', #24057, 0.1000000000000000472, 0.003490658503988666988 ) ;
#11526 = CIRCLE ( 'NONE', #9475, 0.06509327318403745899 ) ;
#11527 = VERTEX_POINT ( 'NONE', #34393 ) ;
#11528 = CARTESIAN_POINT ( 'NONE',  ( -7.950000000000016165, 2.500000000000000000, -6.495190528383297135 ) ) ;
#11529 = ADVANCED_FACE ( 'NONE', ( #104401 ), #116144, .T. ) ;
#11530 = DIRECTION ( 'NONE',  ( -0.000000000000000000, -1.000000000000000000, -0.000000000000000000 ) ) ;
#11531 = LINE ( 'NONE', #61289, #33861 ) ;
#11532 = CARTESIAN_POINT ( 'NONE',  ( -7.900000000000011013, 2.500000000000000000, 3.737306695894644371 ) ) ;
#11533 = VERTEX_POINT ( 'NONE', #15349 ) ;
#11534 = CARTESIAN_POINT ( 'NONE',  ( 5.599999999999934808, 2.500000000000000000, -3.983716857408426293 ) ) ;
#11535 = CIRCLE ( 'NONE', #47143, 0.1000000000000000056 ) ;
#11536 = AXIS2_PLACEMENT_3D ( 'NONE', #29477, #9829, #102705 ) ;
#11537 = CARTESIAN_POINT ( 'NONE',  ( 8.549999999999920774, 2.500000000000000000, -2.511473670974877948 ) ) ;
#11539 = ORIENTED_EDGE ( 'NONE', *, *, #10998, .T. ) ;
#11538 = DIRECTION ( 'NONE',  ( -0.000000000000000000, 1.000000000000000000, -0.000000000000000000 ) ) ;
#11540 = ORIENTED_EDGE ( 'NONE', *, *, #62244, .F. ) ;
#11541 = DIRECTION ( 'NONE',  ( -0.000000000000000000, 1.000000000000000000, -0.000000000000000000 ) ) ;
#11542 = AXIS2_PLACEMENT_3D ( 'NONE', #28501, #88702, #129299 ) ;
#11543 = ORIENTED_EDGE ( 'NONE', *, *, #55131, .F. ) ;
#11544 = EDGE_LOOP ( 'NONE', ( #124246, #124825, #113784, #3602 ) ) ;
#11545 = DIRECTION ( 'NONE',  ( 0.000000000000000000, 0.000000000000000000, -1.000000000000000000 ) ) ;
#11546 = CARTESIAN_POINT ( 'NONE',  ( 3.149999999999946176, 2.500000000000000000, -6.148780366869526226 ) ) ;
#11547 = DIRECTION ( 'NONE',  ( -0.000000000000000000, -1.000000000000000000, -0.000000000000000000 ) ) ;
#11548 = CARTESIAN_POINT ( 'NONE',  ( 15.83209681635555022, 2.500000000000000000, -5.404881881984143099 ) ) ;
#11549 = ORIENTED_EDGE ( 'NONE', *, *, #37870, .T. ) ;
#11550 = ADVANCED_FACE ( 'NONE', ( #6181 ), #67602, .T. ) ;
#11551 = DIRECTION ( 'NONE',  ( -0.000000000000000000, 1.000000000000000000, -0.000000000000000000 ) ) ;
#11552 = ORIENTED_EDGE ( 'NONE', *, *, #107469, .T. ) ;
#11553 = CARTESIAN_POINT ( 'NONE',  ( 17.50000000000010658, 2.362777783882526350, 3.757134105503078469 ) ) ;
#11554 = DIRECTION ( 'NONE',  ( -0.000000000000000000, -1.000000000000000000, -0.000000000000000000 ) ) ;
#11555 = AXIS2_PLACEMENT_3D ( 'NONE', #1341, #111278, #30184 ) ;
#11556 = ADVANCED_FACE ( 'NONE', ( #125330 ), #25756, .T. ) ;
#11557 = ORIENTED_EDGE ( 'NONE', *, *, #21654, .T. ) ;
#11558 = CIRCLE ( 'NONE', #93057, 0.06509327318403745899 ) ;
#11559 = EDGE_LOOP ( 'NONE', ( #4061, #6503 ) ) ;
#11560 = CIRCLE ( 'NONE', #26157, 0.09999999999999982514 ) ;
#11561 = ORIENTED_EDGE ( 'NONE', *, *, #51653, .T. ) ;
#11562 = ORIENTED_EDGE ( 'NONE', *, *, #128317, .T. ) ;
#11563 = CARTESIAN_POINT ( 'NONE',  ( -13.09999999999999254, 2.500000000000000000, -4.676537180435975216 ) ) ;
#11564 = DIRECTION ( 'NONE',  ( 0.000000000000000000, 0.000000000000000000, 1.000000000000000000 ) ) ;
#11565 = EDGE_CURVE ( 'NONE', #18996, #102121, #95233, .T. ) ;
#11566 = CIRCLE ( 'NONE', #26159, 0.09999999999999999167 ) ;
#11567 = EDGE_CURVE ( 'NONE', #70253, #113534, #36237, .T. ) ;
#11568 = DIRECTION ( 'NONE',  ( 0.000000000000000000, 1.000000000000000000, 0.000000000000000000 ) ) ;
#11569 = EDGE_CURVE ( 'NONE', #63649, #13514, #82205, .T. ) ;
#11570 = FACE_BOUND ( 'NONE', #24913, .T. ) ;
#11571 = ADVANCED_FACE ( 'NONE', ( #4243 ), #44182, .T. ) ;
#11572 = CARTESIAN_POINT ( 'NONE',  ( 1.249999999999988898, 12.50000000000000000, -6.495190528383302464 ) ) ;
#11573 = CARTESIAN_POINT ( 'NONE',  ( 184.0312500006828031, 9.429780353434619030E-16, -7.700000000000000178 ) ) ;
#11574 = DIRECTION ( 'NONE',  ( 0.000000000000000000, 0.000000000000000000, 1.000000000000000000 ) ) ;
#11575 = CARTESIAN_POINT ( 'NONE',  ( -5.800000000000022027, 12.50000000000000000, -4.395220292106239768 ) ) ;
#11576 = CONICAL_SURFACE ( 'NONE', #84739, 0.09999999999999982514, 0.003490658503988666988 ) ;
#11577 = CIRCLE ( 'NONE', #95214, 0.06509327318403745899 ) ;
#11578 = CARTESIAN_POINT ( 'NONE',  ( 12.69999999999990337, 2.500000000000000000, 4.083716857408420609 ) ) ;
#11579 = CIRCLE ( 'NONE', #45054, 0.09999999999999982514 ) ;
#11580 = DIRECTION ( 'NONE',  ( 0.000000000000000000, 1.000000000000000000, 0.000000000000000000 ) ) ;
#11581 = ADVANCED_FACE ( 'NONE', ( #24548 ), #46692, .T. ) ;
#11582 = CARTESIAN_POINT ( 'NONE',  ( 1.249999999999952038, 2.500000000000000000, 5.802370205355744659 ) ) ;
#11583 = EDGE_CURVE ( 'NONE', #19309, #65281, #88445, .T. ) ;
#11584 = CIRCLE ( 'NONE', #128701, 0.06509327318403745899 ) ;
#11585 = AXIS2_PLACEMENT_3D ( 'NONE', #72802, #13861, #43993 ) ;
#11586 = EDGE_CURVE ( 'NONE', #54506, #102089, #48759, .T. ) ;
#11587 = CARTESIAN_POINT ( 'NONE',  ( 14.14999999999989377, 2.500000000000000000, -1.472243186433550122 ) ) ;
#11588 = CIRCLE ( 'NONE', #47195, 0.1000000000000002554 ) ;
#11589 = ORIENTED_EDGE ( 'NONE', *, *, #80662, .T. ) ;
#11590 = ORIENTED_EDGE ( 'NONE', *, *, #50560, .T. ) ;
#11591 = ORIENTED_EDGE ( 'NONE', *, *, #123570, .F. ) ;
#11592 = VERTEX_POINT ( 'NONE', #45496 ) ;
#11593 = VECTOR ( 'NONE', #94923, 1000.000000000000000 ) ;
#11594 = ORIENTED_EDGE ( 'NONE', *, *, #13690, .F. ) ;
#11595 = DIRECTION ( 'NONE',  ( 0.000000000000000000, 0.000000000000000000, -1.000000000000000000 ) ) ;
#11596 = DIRECTION ( 'NONE',  ( -0.000000000000000000, -1.000000000000000000, -0.000000000000000000 ) ) ;
#11597 = ORIENTED_EDGE ( 'NONE', *, *, #65200, .F. ) ;
#11598 = FACE_BOUND ( 'NONE', #58262, .T. ) ;
#11599 = CARTESIAN_POINT ( 'NONE',  ( 0.3999999999999559464, 2.500000000000000000, -4.330127018922201643 ) ) ;
#11600 = VERTEX_POINT ( 'NONE', #86023 ) ;
#11601 = CARTESIAN_POINT ( 'NONE',  ( 8.749999999999921840, 2.500000000000000000, 2.857883832488649301 ) ) ;
#11602 = DIRECTION ( 'NONE',  ( -0.000000000000000000, 1.000000000000000000, -0.000000000000000000 ) ) ;
#11603 = DIRECTION ( 'NONE',  ( 0.000000000000000000, 0.000000000000000000, -1.000000000000000000 ) ) ;
#11604 = DIRECTION ( 'NONE',  ( 0.000000000000000000, 1.000000000000000000, 0.000000000000000000 ) ) ;
#11606 = ORIENTED_EDGE ( 'NONE', *, *, #90779, .T. ) ;
#11605 = CIRCLE ( 'NONE', #49285, 0.1000000000000002554 ) ;
#11607 = DIRECTION ( 'NONE',  ( 0.000000000000000000, 0.000000000000000000, -1.000000000000000000 ) ) ;
#11608 = EDGE_LOOP ( 'NONE', ( #32035, #59023, #125745, #24689 ) ) ;
#11609 = EDGE_LOOP ( 'NONE', ( #62790, #72339, #104159, #19984 ) ) ;
#11610 = DIRECTION ( 'NONE',  ( 0.000000000000000000, 1.000000000000000000, 0.000000000000000000 ) ) ;
#11611 = LINE ( 'NONE', #112404, #74814 ) ;
#11612 = AXIS2_PLACEMENT_3D ( 'NONE', #62970, #82627, #21107 ) ;
#11613 = EDGE_LOOP ( 'NONE', ( #112554, #88040 ) ) ;
#11614 = DIRECTION ( 'NONE',  ( 0.000000000000000000, 1.000000000000000000, 0.000000000000000000 ) ) ;
#11615 = AXIS2_PLACEMENT_3D ( 'NONE', #12069, #82771, #4167 ) ;
#11616 = AXIS2_PLACEMENT_3D ( 'NONE', #88706, #99179, #38331 ) ;
#11617 = DIRECTION ( 'NONE',  ( 0.000000000000000000, 0.000000000000000000, -1.000000000000000000 ) ) ;
#11618 = CARTESIAN_POINT ( 'NONE',  ( 3.949999999999938893, 2.500000000000000000, 6.148780366869520009 ) ) ;
#11619 = DIRECTION ( 'NONE',  ( 0.000000000000000000, 1.000000000000000000, 0.000000000000000000 ) ) ;
#11620 = DIRECTION ( 'NONE',  ( -4.274815082592931898E-19, -0.9999939076577903929, -0.003490651415223739937 ) ) ;
#11621 = EDGE_LOOP ( 'NONE', ( #95465, #12397, #28165, #85984 ) ) ;
#11622 = FACE_OUTER_BOUND ( 'NONE', #121884, .T. ) ;
#11623 = EDGE_CURVE ( 'NONE', #88605, #56169, #128277, .T. ) ;
#11624 = VERTEX_POINT ( 'NONE', #76238 ) ;
#11625 = DIRECTION ( 'NONE',  ( 0.000000000000000000, 1.000000000000000000, 0.000000000000000000 ) ) ;
#11626 = AXIS2_PLACEMENT_3D ( 'NONE', #13651, #14295, #102679 ) ;
#11627 = EDGE_CURVE ( 'NONE', #26724, #113868, #113596, .T. ) ;
#11628 = ORIENTED_EDGE ( 'NONE', *, *, #90273, .F. ) ;
#11631 = EDGE_CURVE ( 'NONE', #8603, #93230, #80145, .T. ) ;
#11630 = LINE ( 'NONE', #50926, #39296 ) ;
#11629 = CIRCLE ( 'NONE', #15831, 0.09999999999999999167 ) ;
#11632 = ORIENTED_EDGE ( 'NONE', *, *, #24080, .F. ) ;
#11633 = CARTESIAN_POINT ( 'NONE',  ( -8.300000000000011369, 2.500000000000000000, -2.276824562219559311E-15 ) ) ;
#11634 = DIRECTION ( 'NONE',  ( -0.000000000000000000, 1.000000000000000000, -0.000000000000000000 ) ) ;
#11635 = DIRECTION ( 'NONE',  ( 0.000000000000000000, 1.000000000000000000, 0.000000000000000000 ) ) ;
#11636 = DIRECTION ( 'NONE',  ( 0.000000000000000000, 0.000000000000000000, 1.000000000000000000 ) ) ;
#11637 = DIRECTION ( 'NONE',  ( 0.000000000000000000, 1.000000000000000000, 0.000000000000000000 ) ) ;
#11638 = EDGE_LOOP ( 'NONE', ( #65945, #88227 ) ) ;
#11639 = EDGE_CURVE ( 'NONE', #26161, #102161, #15266, .T. ) ;
#11640 = VERTEX_POINT ( 'NONE', #54638 ) ;
#11641 = ORIENTED_EDGE ( 'NONE', *, *, #7715, .T. ) ;
#11642 = PLANE ( 'NONE',  #80958 ) ;
#11643 = AXIS2_PLACEMENT_3D ( 'NONE', #89827, #57805, #90460 ) ;
#11644 = CARTESIAN_POINT ( 'NONE',  ( -7.500000000000011546, 2.500000000000000000, 3.737306695894644371 ) ) ;
#11645 = CARTESIAN_POINT ( 'NONE',  ( 2.099999999999950351, 2.500000000000000000, -5.022947341949754119 ) ) ;
#11647 = ORIENTED_EDGE ( 'NONE', *, *, #35434, .T. ) ;
#11646 = ORIENTED_EDGE ( 'NONE', *, *, #40896, .T. ) ;
#11648 = ORIENTED_EDGE ( 'NONE', *, *, #70288, .T. ) ;
#11649 = PLANE ( 'NONE',  #85451 ) ;
#11650 = ORIENTED_EDGE ( 'NONE', *, *, #80000, .T. ) ;
#11651 = CARTESIAN_POINT ( 'NONE',  ( 6.649999999999930189, 2.500000000000000000, -1.472243186433550122 ) ) ;
#11652 = FACE_OUTER_BOUND ( 'NONE', #103116, .T. ) ;
#11653 = CARTESIAN_POINT ( 'NONE',  ( -10.85000000000000142, 2.500000000000000000, -5.902370205355746968 ) ) ;
#11654 = DIRECTION ( 'NONE',  ( 0.000000000000000000, 0.000000000000000000, -1.000000000000000000 ) ) ;
#11655 = CARTESIAN_POINT ( 'NONE',  ( 127.5000000000000000, 2.000000000000000000, 5.000000000000001776 ) ) ;
#11656 = CARTESIAN_POINT ( 'NONE',  ( 7.299999999999924327, 2.500000000000000000, 0.3464101615137735735 ) ) ;
#11657 = FACE_OUTER_BOUND ( 'NONE', #23066, .T. ) ;
#11658 = EDGE_CURVE ( 'NONE', #108389, #96060, #87955, .T. ) ;
#11659 = CARTESIAN_POINT ( 'NONE',  ( 3.949999999999938005, 2.500000000000000000, 6.841600689897072485 ) ) ;
#11660 = ORIENTED_EDGE ( 'NONE', *, *, #98655, .F. ) ;
#11661 = DIRECTION ( 'NONE',  ( -0.000000000000000000, 1.000000000000000000, -0.000000000000000000 ) ) ;
#11662 = AXIS2_PLACEMENT_3D ( 'NONE', #114798, #74243, #112881 ) ;
#11663 = AXIS2_PLACEMENT_3D ( 'NONE', #32966, #100399, #10693 ) ;
#11664 = DIRECTION ( 'NONE',  ( 0.000000000000000000, -0.9999939076577903929, 0.003490651415223739937 ) ) ;
#11665 = ORIENTED_EDGE ( 'NONE', *, *, #93777, .T. ) ;
#11666 = ORIENTED_EDGE ( 'NONE', *, *, #11420, .F. ) ;
#11667 = CARTESIAN_POINT ( 'NONE',  ( 187.3385416670080872, 6.551208109652274736, 3.782341765625001351 ) ) ;
#11668 = DIRECTION ( 'NONE',  ( 0.000000000000000000, 0.000000000000000000, -1.000000000000000000 ) ) ;
#11669 = DIRECTION ( 'NONE',  ( 0.000000000000000000, -0.9999939076577903929, 0.003490651415223739937 ) ) ;
#11670 = CARTESIAN_POINT ( 'NONE',  ( 1.699999999999951994, 12.50000000000000000, -4.330127018922201643 ) ) ;
#11671 = CARTESIAN_POINT ( 'NONE',  ( 13.74999999999989697, 12.50000000000000000, 2.857883832488649301 ) ) ;
#11672 = DIRECTION ( 'NONE',  ( 0.000000000000000000, 0.000000000000000000, 1.000000000000000000 ) ) ;
#11673 = ADVANCED_FACE ( 'NONE', ( #127275 ), #21659, .T. ) ;
#11674 = CARTESIAN_POINT ( 'NONE',  ( 9.599999999999917932, 12.50000000000000000, 0.6277270498435120194 ) ) ;
#11675 = CARTESIAN_POINT ( 'NONE',  ( 4.549999999999939426, 2.500000000000000000, -6.395190528383301931 ) ) ;
#11676 = AXIS2_PLACEMENT_3D ( 'NONE', #46812, #7513, #47453 ) ;
#11677 = CARTESIAN_POINT ( 'NONE',  ( -12.89999999999999147, 2.500000000000000000, -4.922947341949750921 ) ) ;
#11678 = AXIS2_PLACEMENT_3D ( 'NONE', #95884, #18605, #68348 ) ;
#11679 = AXIS2_PLACEMENT_3D ( 'NONE', #98220, #8537, #48487 ) ;
#11680 = ORIENTED_EDGE ( 'NONE', *, *, #35929, .F. ) ;
#11681 = VERTEX_POINT ( 'NONE', #79465 ) ;
#11682 = AXIS2_PLACEMENT_3D ( 'NONE', #50441, #71357, #49185 ) ;
#11683 = EDGE_LOOP ( 'NONE', ( #110846, #107101 ) ) ;
#11684 = CIRCLE ( 'NONE', #128503, 0.06509327318403743123 ) ;
#11685 = EDGE_LOOP ( 'NONE', ( #127081, #66376, #81529, #44408 ) ) ;
#11686 = EDGE_CURVE ( 'NONE', #73744, #115596, #108260, .T. ) ;
#11687 = CARTESIAN_POINT ( 'NONE',  ( -0.8500000000000382805, 2.500000000000000000, -5.802370205355749988 ) ) ;
#11688 = CARTESIAN_POINT ( 'NONE',  ( 7.499999999999961808, 12.50000000000000000, 4.330127018922196314 ) ) ;
#11689 = ORIENTED_EDGE ( 'NONE', *, *, #13497, .F. ) ;
#11690 = DIRECTION ( 'NONE',  ( -0.000000000000000000, -1.000000000000000000, -0.000000000000000000 ) ) ;
#11691 = DIRECTION ( 'NONE',  ( -0.000000000000000000, -1.000000000000000000, -0.000000000000000000 ) ) ;
#11692 = CARTESIAN_POINT ( 'NONE',  ( -3.644143946350442628E-14, 2.500000000000000000, 0.5928203230275517210 ) ) ;
#11694 = ORIENTED_EDGE ( 'NONE', *, *, #126365, .T. ) ;
#11693 = CYLINDRICAL_SURFACE ( 'NONE', #74639, 2.749999999999997335 ) ;
#11695 = EDGE_CURVE ( 'NONE', #17926, #90702, #124052, .T. ) ;
#11696 = CARTESIAN_POINT ( 'NONE',  ( 6.649999999999930189, 12.50000000000000000, 7.188010851410848723 ) ) ;
#11697 = VECTOR ( 'NONE', #57509, 1000.000000000000000 ) ;
#11698 = DIRECTION ( 'NONE',  ( -0.000000000000000000, 1.000000000000000000, -0.000000000000000000 ) ) ;
#11699 = VERTEX_POINT ( 'NONE', #229 ) ;
#11700 = ORIENTED_EDGE ( 'NONE', *, *, #40467, .F. ) ;
#11701 = VERTEX_POINT ( 'NONE', #17275 ) ;
#11702 = VERTEX_POINT ( 'NONE', #48068 ) ;
#11703 = LINE ( 'NONE', #100098, #65598 ) ;
#11704 = CIRCLE ( 'NONE', #74406, 0.1000000000000000056 ) ;
#11705 = VECTOR ( 'NONE', #72777, 1000.000000000000000 ) ;
#11706 = FACE_OUTER_BOUND ( 'NONE', #31501, .T. ) ;
#11707 = CARTESIAN_POINT ( 'NONE',  ( 2.500000000000002220, -2.500000000000000000, -8.999999999999998224 ) ) ;
#11708 = AXIS2_PLACEMENT_3D ( 'NONE', #84025, #85324, #93861 ) ;
#11709 = VERTEX_POINT ( 'NONE', #87321 ) ;
#11710 = CIRCLE ( 'NONE', #68141, 0.09999999999999999167 ) ;
#11711 = EDGE_CURVE ( 'NONE', #24007, #127312, #101068, .T. ) ;
#11712 = DIRECTION ( 'NONE',  ( 0.000000000000000000, -0.000000000000000000, 1.000000000000000000 ) ) ;
#11713 = ORIENTED_EDGE ( 'NONE', *, *, #34242, .F. ) ;
#11714 = DIRECTION ( 'NONE',  ( 0.000000000000000000, 0.000000000000000000, 1.000000000000000000 ) ) ;
#11715 = DIRECTION ( 'NONE',  ( 0.000000000000000000, -0.9999939076577903929, 0.003490651415223739937 ) ) ;
#11716 = DIRECTION ( 'NONE',  ( -0.000000000000000000, -1.000000000000000000, -0.000000000000000000 ) ) ;
#11717 = CARTESIAN_POINT ( 'NONE',  ( 0.3999999999999628852, 2.500000000000000000, 0.6928203230275518099 ) ) ;
#11718 = AXIS2_PLACEMENT_3D ( 'NONE', #32041, #73236, #116999 ) ;
#11719 = EDGE_CURVE ( 'NONE', #73752, #114231, #4909, .T. ) ;
#11720 = ORIENTED_EDGE ( 'NONE', *, *, #50620, .F. ) ;
#11721 = CONICAL_SURFACE ( 'NONE', #84880, 0.1000000000000002554, 0.003490658503988666988 ) ;
#11722 = ORIENTED_EDGE ( 'NONE', *, *, #24321, .F. ) ;
#11723 = ORIENTED_EDGE ( 'NONE', *, *, #8159, .F. ) ;
#11724 = CARTESIAN_POINT ( 'NONE',  ( -13.14999999999999147, 12.50000000000000000, -2.511473670974875727 ) ) ;
#11725 = ADVANCED_FACE ( 'NONE', ( #117409 ), #59232, .T. ) ;
#11726 = EDGE_CURVE ( 'NONE', #101017, #97372, #126103, .T. ) ;
#11727 = DIRECTION ( 'NONE',  ( 0.000000000000000000, 0.000000000000000000, -1.000000000000000000 ) ) ;
#11728 = ADVANCED_FACE ( 'NONE', ( #29081, #57229, #39562 ), #19222, .T. ) ;
#11729 = FACE_BOUND ( 'NONE', #6724, .T. ) ;
#11730 = ADVANCED_FACE ( 'NONE', ( #120025 ), #61367, .T. ) ;
#11731 = FACE_OUTER_BOUND ( 'NONE', #15787, .T. ) ;
#11732 = CARTESIAN_POINT ( 'NONE',  ( -10.40000000000000213, 2.500000000000000000, -4.922947341949749145 ) ) ;
#11733 = DIRECTION ( 'NONE',  ( 0.000000000000000000, 1.000000000000000000, 0.000000000000000000 ) ) ;
#11734 = EDGE_CURVE ( 'NONE', #56626, #40907, #92665, .T. ) ;
#11735 = PLANE ( 'NONE',  #96504 ) ;
#11736 = ADVANCED_FACE ( 'NONE', ( #109561 ), #38398, .T. ) ;
#11737 = DIRECTION ( 'NONE',  ( -0.000000000000000000, 1.000000000000000000, -0.000000000000000000 ) ) ;
#11738 = EDGE_CURVE ( 'NONE', #93976, #91980, #15367, .T. ) ;
#11739 = CARTESIAN_POINT ( 'NONE',  ( 3.149999999999946176, 2.500000000000000000, -2.511473670974877948 ) ) ;
#11740 = VERTEX_POINT ( 'NONE', #106961 ) ;
#11741 = CARTESIAN_POINT ( 'NONE',  ( -7.300000000000013145, 2.500000000000000000, 3.883716857408420431 ) ) ;
#11742 = EDGE_CURVE ( 'NONE', #64939, #28650, #32046, .T. ) ;
#11743 = EDGE_CURVE ( 'NONE', #68741, #81973, #97798, .T. ) ;
#11744 = DIRECTION ( 'NONE',  ( 0.000000000000000000, 0.000000000000000000, 1.000000000000000000 ) ) ;
#11745 = ORIENTED_EDGE ( 'NONE', *, *, #22526, .F. ) ;
#11746 = EDGE_LOOP ( 'NONE', ( #106242, #93809 ) ) ;
#11747 = CARTESIAN_POINT ( 'NONE',  ( 5.599999999999931255, 2.500000000000000000, 4.676537180435972552 ) ) ;
#11748 = ADVANCED_FACE ( 'NONE', ( #99748 ), #65562, .T. ) ;
#11749 = DIRECTION ( 'NONE',  ( -0.000000000000000000, 1.000000000000000000, -0.000000000000000000 ) ) ;
#11750 = FACE_BOUND ( 'NONE', #28613, .T. ) ;
#11751 = ADVANCED_FACE ( 'NONE', ( #59184 ), #40549, .T. ) ;
#11752 = LINE ( 'NONE', #89672, #53493 ) ;
#11753 = AXIS2_PLACEMENT_3D ( 'NONE', #74099, #94364, #15801 ) ;
#11754 = CONICAL_SURFACE ( 'NONE', #84915, 0.1000000000000002554, 0.003490658503988666988 ) ;
#11755 = ORIENTED_EDGE ( 'NONE', *, *, #35621, .F. ) ;
#11756 = DIRECTION ( 'NONE',  ( 0.000000000000000000, 1.000000000000000000, 0.000000000000000000 ) ) ;
#11757 = DIRECTION ( 'NONE',  ( -0.000000000000000000, 1.000000000000000000, -0.000000000000000000 ) ) ;
#11758 = EDGE_LOOP ( 'NONE', ( #121048, #75033, #84519, #81080, #106240, #113742, #89082, #11246, #100895, #84403, #75375, #87595 ) ) ;
#11759 = DIRECTION ( 'NONE',  ( 0.000000000000000000, -0.9999939076577903929, 0.003490651415223739937 ) ) ;
#11760 = DIRECTION ( 'NONE',  ( 0.000000000000000000, -0.000000000000000000, 1.000000000000000000 ) ) ;
#11761 = CIRCLE ( 'NONE', #84923, 0.1000000000000002554 ) ;
#11762 = CARTESIAN_POINT ( 'NONE',  ( 8.749999999999918288, 12.50000000000000000, 7.188010851410848723 ) ) ;
#11763 = DIRECTION ( 'NONE',  ( 0.000000000000000000, 0.000000000000000000, -1.000000000000000000 ) ) ;
#11765 = CONICAL_SURFACE ( 'NONE', #95404, 0.1000000000000002554, 0.003490658503988666988 ) ;
#11764 = VECTOR ( 'NONE', #53236, 1000.000000000000000 ) ;
#11766 = EDGE_LOOP ( 'NONE', ( #60812, #85043 ) ) ;
#11767 = CIRCLE ( 'NONE', #20190, 0.06509327318403745899 ) ;
#11768 = CARTESIAN_POINT ( 'NONE',  ( 5.849999999999931255, 2.500000000000000000, 2.757883832488649656 ) ) ;
#11769 = FACE_OUTER_BOUND ( 'NONE', #57869, .T. ) ;
#11770 = DIRECTION ( 'NONE',  ( 0.000000000000000000, 0.000000000000000000, 1.000000000000000000 ) ) ;
#11771 = ORIENTED_EDGE ( 'NONE', *, *, #119343, .F. ) ;
#11772 = VERTEX_POINT ( 'NONE', #80753 ) ;
#11773 = DIRECTION ( 'NONE',  ( 0.000000000000000000, -0.000000000000000000, 1.000000000000000000 ) ) ;
#11774 = ORIENTED_EDGE ( 'NONE', *, *, #39714, .T. ) ;
#11775 = FACE_OUTER_BOUND ( 'NONE', #95722, .T. ) ;
#11776 = CARTESIAN_POINT ( 'NONE',  ( -0.8500000000000390576, 2.500000000000000000, -6.595190528383302109 ) ) ;
#11777 = ADVANCED_FACE ( 'NONE', ( #42110 ), #121959, .T. ) ;
#11778 = DIRECTION ( 'NONE',  ( -0.000000000000000000, 1.000000000000000000, -0.000000000000000000 ) ) ;
#11779 = EDGE_LOOP ( 'NONE', ( #68961, #44780 ) ) ;
#11781 = ADVANCED_FACE ( 'NONE', ( #32954 ), #70925, .T. ) ;
#11780 = CARTESIAN_POINT ( 'NONE',  ( -3.350000000000028955, 2.500000000000000000, 7.188010851410848723 ) ) ;
#11782 = DIRECTION ( 'NONE',  ( -0.000000000000000000, -1.000000000000000000, -0.000000000000000000 ) ) ;
#11783 = CARTESIAN_POINT ( 'NONE',  ( 107.5000000000000142, 0.000000000000000000, 0.000000000000000000 ) ) ;
#11784 = CARTESIAN_POINT ( 'NONE',  ( -12.89999999999999147, 2.500000000000000000, 3.737306695894644371 ) ) ;
#11785 = CARTESIAN_POINT ( 'NONE',  ( 1.249999999999952038, 2.500000000000000000, 2.857883832488649301 ) ) ;
#11786 = AXIS2_PLACEMENT_3D ( 'NONE', #122876, #91469, #1786 ) ;
#11787 = CARTESIAN_POINT ( 'NONE',  ( 15.19999999999989271, 2.500000000000000000, -0.3464101615137783474 ) ) ;
#11788 = EDGE_CURVE ( 'NONE', #79738, #31609, #112142, .T. ) ;
#11789 = ORIENTED_EDGE ( 'NONE', *, *, #39111, .T. ) ;
#11790 = ORIENTED_EDGE ( 'NONE', *, *, #86360, .F. ) ;
#11791 = DIRECTION ( 'NONE',  ( 0.000000000000000000, 1.000000000000000000, 0.000000000000000000 ) ) ;
#11792 = ORIENTED_EDGE ( 'NONE', *, *, #42174, .F. ) ;
#11793 = AXIS2_PLACEMENT_3D ( 'NONE', #98481, #88681, #79514 ) ;
#11794 = AXIS2_PLACEMENT_3D ( 'NONE', #125957, #7473, #116780 ) ;
#11795 = CARTESIAN_POINT ( 'NONE',  ( -3.750000000000029310, 2.500000000000000000, -7.088010851410853519 ) ) ;
#11797 = ORIENTED_EDGE ( 'NONE', *, *, #65518, .F. ) ;
#11796 = EDGE_LOOP ( 'NONE', ( #104407, #26612 ) ) ;
#11798 = ORIENTED_EDGE ( 'NONE', *, *, #8272, .T. ) ;
#11799 = CARTESIAN_POINT ( 'NONE',  ( -15.39999999999998082, 2.500000000000000000, 0.5928203230275517210 ) ) ;
#11800 = CIRCLE ( 'NONE', #34809, 0.06509327318403745899 ) ;
#11801 = FACE_OUTER_BOUND ( 'NONE', #35238, .T. ) ;
#11802 = CARTESIAN_POINT ( 'NONE',  ( -3.150000000000029221, 2.500000000000000000, 2.511473670974873507 ) ) ;
#11803 = VECTOR ( 'NONE', #66278, 1000.000000000000000 ) ;
#11804 = CARTESIAN_POINT ( 'NONE',  ( -12.04999999999999538, 2.500000000000000000, 2.065063509461097624 ) ) ;
#11805 = DIRECTION ( 'NONE',  ( -0.000000000000000000, -1.000000000000000000, -0.000000000000000000 ) ) ;
#11806 = CARTESIAN_POINT ( 'NONE',  ( -10.60000000000000142, 2.500000000000000000, 3.883716857408421319 ) ) ;
#11807 = DIRECTION ( 'NONE',  ( 0.000000000000000000, 0.000000000000000000, -1.000000000000000000 ) ) ;
#11808 = CARTESIAN_POINT ( 'NONE',  ( -8.750000000000007105, 2.500000000000000000, 7.288010851410849256 ) ) ;
#11809 = FACE_OUTER_BOUND ( 'NONE', #50382, .T. ) ;
#11810 = CONICAL_SURFACE ( 'NONE', #55725, 0.09999999999999982514, 0.003490658503988666988 ) ;
#11811 = ORIENTED_EDGE ( 'NONE', *, *, #64171, .F. ) ;
#11813 = AXIS2_PLACEMENT_3D ( 'NONE', #123650, #101459, #71333 ) ;
#11812 = CONICAL_SURFACE ( 'NONE', #95446, 0.09999999999999982514, 0.003490658503988666988 ) ;
#11814 = CARTESIAN_POINT ( 'NONE',  ( 12.29999999999990656, 2.500000000000000000, 3.983716857408420964 ) ) ;
#11815 = VERTEX_POINT ( 'NONE', #102322 ) ;
#11816 = ORIENTED_EDGE ( 'NONE', *, *, #4207, .F. ) ;
#11817 = FACE_OUTER_BOUND ( 'NONE', #42637, .T. ) ;
#11818 = CYLINDRICAL_SURFACE ( 'NONE', #110333, 7.700000000000000178 ) ;
#11819 = DIRECTION ( 'NONE',  ( -0.000000000000000000, 1.000000000000000000, -0.000000000000000000 ) ) ;
#11820 = ADVANCED_FACE ( 'NONE', ( #100384 ), #128378, .T. ) ;
#11821 = CARTESIAN_POINT ( 'NONE',  ( 11.24999999999991118, 2.500000000000000000, -2.857883832488653741 ) ) ;
#11822 = CARTESIAN_POINT ( 'NONE',  ( -11.05000000000000071, 12.50000000000000000, 2.511473670974873507 ) ) ;
#11823 = FACE_OUTER_BOUND ( 'NONE', #53396, .T. ) ;
#11824 = DIRECTION ( 'NONE',  ( 0.000000000000000000, 1.000000000000000000, 0.000000000000000000 ) ) ;
#11825 = ORIENTED_EDGE ( 'NONE', *, *, #96079, .T. ) ;
#11826 = EDGE_LOOP ( 'NONE', ( #126598, #96316 ) ) ;
#11827 = ORIENTED_EDGE ( 'NONE', *, *, #52198, .F. ) ;
#11828 = VERTEX_POINT ( 'NONE', #70285 ) ;
#11829 = EDGE_CURVE ( 'NONE', #61230, #14447, #117874, .T. ) ;
#11831 = EDGE_LOOP ( 'NONE', ( #9628, #70937, #65606, #50521 ) ) ;
#11830 = EDGE_CURVE ( 'NONE', #116790, #111264, #21167, .T. ) ;
#11832 = DIRECTION ( 'NONE',  ( 0.000000000000000000, 0.000000000000000000, -1.000000000000000000 ) ) ;
#11833 = CARTESIAN_POINT ( 'NONE',  ( 0.1999999999999627909, 2.500000000000000000, 0.2464101615137758439 ) ) ;
#11834 = AXIS2_PLACEMENT_3D ( 'NONE', #32098, #31446, #121101 ) ;
#11835 = CARTESIAN_POINT ( 'NONE',  ( 139.9358549477330200, 2.500000000000000000, -3.576063159858998475 ) ) ;
#11837 = DIRECTION ( 'NONE',  ( 0.000000000000000000, 1.000000000000000000, 0.000000000000000000 ) ) ;
#11836 = CONICAL_SURFACE ( 'NONE', #66126, 0.1000000000000002554, 0.003490658503988666988 ) ;
#11838 = DIRECTION ( 'NONE',  ( 0.000000000000000000, -0.9999939076577903929, 0.003490651415223739937 ) ) ;
#11839 = ORIENTED_EDGE ( 'NONE', *, *, #102423, .T. ) ;
#11840 = DIRECTION ( 'NONE',  ( 0.000000000000000000, 0.000000000000000000, -1.000000000000000000 ) ) ;
#11841 = DIRECTION ( 'NONE',  ( -0.000000000000000000, -1.000000000000000000, -0.000000000000000000 ) ) ;
#11842 = EDGE_CURVE ( 'NONE', #55864, #47422, #52563, .T. ) ;
#11843 = CARTESIAN_POINT ( 'NONE',  ( -8.350000000000012079, 2.500000000000000000, 1.372243186433545370 ) ) ;
#11844 = DIRECTION ( 'NONE',  ( 0.000000000000000000, 1.000000000000000000, 0.000000000000000000 ) ) ;
#11846 = AXIS2_PLACEMENT_3D ( 'NONE', #35117, #75025, #65175 ) ;
#11845 = AXIS2_PLACEMENT_3D ( 'NONE', #59712, #756, #129099 ) ;
#11847 = CARTESIAN_POINT ( 'NONE',  ( 187.2395833340161460, 4.445597072760117285, 7.700000000000001066 ) ) ;
#11848 = VERTEX_POINT ( 'NONE', #91855 ) ;
#11849 = ORIENTED_EDGE ( 'NONE', *, *, #63749, .T. ) ;
#11850 = ORIENTED_EDGE ( 'NONE', *, *, #56555, .T. ) ;
#11851 = DIRECTION ( 'NONE',  ( 0.000000000000000000, -0.9999939076577903929, 0.003490651415223739937 ) ) ;
#11852 = VERTEX_POINT ( 'NONE', #81401 ) ;
#11854 = VECTOR ( 'NONE', #87714, 1000.000000000000000 ) ;
#11853 = AXIS2_PLACEMENT_3D ( 'NONE', #102172, #34742, #41967 ) ;
#11855 = DIRECTION ( 'NONE',  ( 0.000000000000000000, 0.000000000000000000, -1.000000000000000000 ) ) ;
#11856 = FACE_OUTER_BOUND ( 'NONE', #92836, .T. ) ;
#11857 = AXIS2_PLACEMENT_3D ( 'NONE', #80192, #102408, #91939 ) ;
#11858 = EDGE_LOOP ( 'NONE', ( #96103, #6259 ) ) ;
#11859 = DIRECTION ( 'NONE',  ( -4.274815082592931898E-19, -0.9999939076577903929, -0.003490651415223739937 ) ) ;
#11860 = CARTESIAN_POINT ( 'NONE',  ( -10.80000000000000249, 2.500000000000000000, -4.330127018922197202 ) ) ;
#11861 = CARTESIAN_POINT ( 'NONE',  ( 6.849999999999929479, 12.50000000000000000, 6.213873640053558134 ) ) ;
#11862 = DIRECTION ( 'NONE',  ( 0.000000000000000000, 1.000000000000000000, 0.000000000000000000 ) ) ;
#11863 = ADVANCED_FACE ( 'NONE', ( #82691 ), #38493, .T. ) ;
#11864 = CARTESIAN_POINT ( 'NONE',  ( -5.850000000000021849, 2.500000000000000000, -1.472243186433550122 ) ) ;
#11865 = ORIENTED_EDGE ( 'NONE', *, *, #84264, .T. ) ;
#11866 = EDGE_LOOP ( 'NONE', ( #71046, #65402 ) ) ;
#11867 = ADVANCED_FACE ( 'NONE', ( #42780 ), #57252, .T. ) ;
#11868 = CARTESIAN_POINT ( 'NONE',  ( -7.700000000000016165, 12.50000000000000000, -4.048810130592463530 ) ) ;
#11869 = AXIS2_PLACEMENT_3D ( 'NONE', #15476, #96606, #94687 ) ;
#11870 = DIRECTION ( 'NONE',  ( 0.000000000000000000, -0.000000000000000000, 1.000000000000000000 ) ) ;
#11871 = CIRCLE ( 'NONE', #127112, 0.1000000000000000472 ) ;
#11872 = ADVANCED_FACE ( 'NONE', ( #120669 ), #4999, .T. ) ;
#11873 = DIRECTION ( 'NONE',  ( -0.000000000000000000, 1.000000000000000000, -0.000000000000000000 ) ) ;
#11874 = CIRCLE ( 'NONE', #60224, 0.06509327318403745899 ) ;
#11875 = DIRECTION ( 'NONE',  ( -4.274815082592931898E-19, -0.9999939076577903929, -0.003490651415223739937 ) ) ;
#11876 = ORIENTED_EDGE ( 'NONE', *, *, #21955, .F. ) ;
#11877 = VECTOR ( 'NONE', #89810, 1000.000000000000000 ) ;
#11878 = EDGE_CURVE ( 'NONE', #78632, #122009, #99013, .T. ) ;
#11879 = EDGE_CURVE ( 'NONE', #68006, #3892, #111483, .T. ) ;
#11880 = ORIENTED_EDGE ( 'NONE', *, *, #45133, .T. ) ;
#11881 = CARTESIAN_POINT ( 'NONE',  ( -1.650000000000034328, 2.500000000000000000, -2.857883832488653741 ) ) ;
#11882 = PLANE ( 'NONE',  #124106 ) ;
#11883 = EDGE_CURVE ( 'NONE', #68389, #124065, #111632, .T. ) ;
#11884 = VECTOR ( 'NONE', #16091, 1000.000000000000000 ) ;
#11885 = DIRECTION ( 'NONE',  ( 0.000000000000000000, -0.9999939076577903929, 0.003490651415223739937 ) ) ;
#11887 = DIRECTION ( 'NONE',  ( -0.000000000000000000, -1.000000000000000000, -0.000000000000000000 ) ) ;
#11886 = AXIS2_PLACEMENT_3D ( 'NONE', #99357, #9675, #78441 ) ;
#11888 = VERTEX_POINT ( 'NONE', #58946 ) ;
#11889 = DIRECTION ( 'NONE',  ( 0.000000000000000000, 0.000000000000000000, -1.000000000000000000 ) ) ;
#11890 = AXIS2_PLACEMENT_3D ( 'NONE', #49885, #119896, #81264 ) ;
#11891 = ADVANCED_FACE ( 'NONE', ( #49139 ), #126204, .T. ) ;
#11892 = LINE ( 'NONE', #52459, #59920 ) ;
#11893 = VERTEX_POINT ( 'NONE', #47843 ) ;
#11894 = CARTESIAN_POINT ( 'NONE',  ( -5.850000000000021849, 12.50000000000000000, -5.737276932171712751 ) ) ;
#11895 = CIRCLE ( 'NONE', #43232, 0.06509327318403745899 ) ;
#11896 = EDGE_LOOP ( 'NONE', ( #115960, #32524, #128395, #93765 ) ) ;
#11897 = EDGE_CURVE ( 'NONE', #102161, #7340, #87736, .T. ) ;
#11898 = DIRECTION ( 'NONE',  ( 0.000000000000000000, 0.000000000000000000, 1.000000000000000000 ) ) ;
#11899 = EDGE_LOOP ( 'NONE', ( #12782, #25185, #58671, #109468 ) ) ;
#11901 = AXIS2_PLACEMENT_3D ( 'NONE', #26762, #125588, #75846 ) ;
#11900 = AXIS2_PLACEMENT_3D ( 'NONE', #117547, #47562, #87459 ) ;
#11902 = EDGE_LOOP ( 'NONE', ( #62032, #17411 ) ) ;
#11903 = CARTESIAN_POINT ( 'NONE',  ( -3.350000000000028955, 2.500000000000000000, 2.065063509461097624 ) ) ;
#11904 = DIRECTION ( 'NONE',  ( -0.000000000000000000, 1.000000000000000000, -0.000000000000000000 ) ) ;
#11905 = ORIENTED_EDGE ( 'NONE', *, *, #110981, .T. ) ;
#11906 = VERTEX_POINT ( 'NONE', #8525 ) ;
#11907 = DIRECTION ( 'NONE',  ( 0.000000000000000000, 0.000000000000000000, 1.000000000000000000 ) ) ;
#11908 = DIRECTION ( 'NONE',  ( -0.000000000000000000, 1.000000000000000000, -0.000000000000000000 ) ) ;
#11909 = CARTESIAN_POINT ( 'NONE',  ( 187.1302083336747444, -4.367472073101514418, -7.564683531250002702 ) ) ;
#11910 = CARTESIAN_POINT ( 'NONE',  ( 185.7343750003414016, 8.734944146203032389, 5.348610694689227483E-16 ) ) ;
#11911 = DIRECTION ( 'NONE',  ( 0.000000000000000000, 0.000000000000000000, 1.000000000000000000 ) ) ;
#11912 = CARTESIAN_POINT ( 'NONE',  ( -9.400000000000009237, 2.500000000000000000, -4.676537180435974328 ) ) ;
#11913 = LINE ( 'NONE', #72778, #115699 ) ;
#11914 = DIRECTION ( 'NONE',  ( 0.000000000000000000, 1.000000000000000000, 0.000000000000000000 ) ) ;
#11915 = DIRECTION ( 'NONE',  ( 0.000000000000000000, -0.000000000000000000, 1.000000000000000000 ) ) ;
#11916 = VECTOR ( 'NONE', #47542, 1000.000000000000000 ) ;
#11917 = ORIENTED_EDGE ( 'NONE', *, *, #4292, .F. ) ;
#11918 = ORIENTED_EDGE ( 'NONE', *, *, #93928, .F. ) ;
#11919 = DIRECTION ( 'NONE',  ( 0.000000000000000000, 0.000000000000000000, 1.000000000000000000 ) ) ;
#11920 = ORIENTED_EDGE ( 'NONE', *, *, #112984, .T. ) ;
#11921 = DIRECTION ( 'NONE',  ( 0.000000000000000000, 0.000000000000000000, -1.000000000000000000 ) ) ;
#11922 = CARTESIAN_POINT ( 'NONE',  ( -5.600000000000020073, 2.500000000000000000, 4.676537180435972552 ) ) ;
#11923 = DIRECTION ( 'NONE',  ( 0.000000000000000000, -0.9999939076577903929, 0.003490651415223739937 ) ) ;
#11925 = ORIENTED_EDGE ( 'NONE', *, *, #129080, .F. ) ;
#11924 = ORIENTED_EDGE ( 'NONE', *, *, #9965, .F. ) ;
#11926 = FACE_BOUND ( 'NONE', #37732, .T. ) ;
#11927 = VERTEX_POINT ( 'NONE', #88372 ) ;
#11928 = FACE_OUTER_BOUND ( 'NONE', #84453, .T. ) ;
#11929 = CARTESIAN_POINT ( 'NONE',  ( -13.34999999999999076, 2.500000000000000000, 1.372243186433549367 ) ) ;
#11930 = CARTESIAN_POINT ( 'NONE',  ( 3.949999999999942446, 2.500000000000000000, -6.841600689897078702 ) ) ;
#11931 = DIRECTION ( 'NONE',  ( 0.000000000000000000, 1.000000000000000000, 0.000000000000000000 ) ) ;
#11932 = CONICAL_SURFACE ( 'NONE', #43352, 0.09999999999999999167, 0.003490658503988666988 ) ;
#11933 = EDGE_CURVE ( 'NONE', #117447, #56076, #127670, .T. ) ;
#11934 = DIRECTION ( 'NONE',  ( -4.274815082592931898E-19, -0.9999939076577903929, -0.003490651415223739937 ) ) ;
#11935 = CIRCLE ( 'NONE', #91356, 0.06509327318403745899 ) ;
#11936 = DIRECTION ( 'NONE',  ( 0.000000000000000000, 0.000000000000000000, 1.000000000000000000 ) ) ;
#11937 = FACE_OUTER_BOUND ( 'NONE', #70291, .T. ) ;
#11938 = CARTESIAN_POINT ( 'NONE',  ( 187.5000000000000000, 0.000000000000000000, 0.000000000000000000 ) ) ;
#11939 = FACE_OUTER_BOUND ( 'NONE', #125683, .T. ) ;
#11940 = DIRECTION ( 'NONE',  ( 0.000000000000000000, 0.000000000000000000, -1.000000000000000000 ) ) ;
#11941 = DIRECTION ( 'NONE',  ( 0.000000000000000000, 0.000000000000000000, -1.000000000000000000 ) ) ;
#11943 = CIRCLE ( 'NONE', #53711, 0.06509327318403741736 ) ;
#11942 = AXIS2_PLACEMENT_3D ( 'NONE', #117133, #89638, #129587 ) ;
#11944 = EDGE_CURVE ( 'NONE', #108909, #122396, #46795, .T. ) ;
#11945 = ORIENTED_EDGE ( 'NONE', *, *, #116953, .T. ) ;
#11946 = EDGE_LOOP ( 'NONE', ( #28845, #109274 ) ) ;
#11947 = VERTEX_POINT ( 'NONE', #79865 ) ;
#11948 = DIRECTION ( 'NONE',  ( 0.000000000000000000, 0.000000000000000000, 1.000000000000000000 ) ) ;
#11949 = EDGE_LOOP ( 'NONE', ( #63197, #90478, #103, #83746 ) ) ;
#11950 = CARTESIAN_POINT ( 'NONE',  ( -3.550000000000027356, 2.500000000000000000, 1.718653347947321386 ) ) ;
#11951 = FACE_OUTER_BOUND ( 'NONE', #76478, .T. ) ;
#11953 = ORIENTED_EDGE ( 'NONE', *, *, #96476, .F. ) ;
#11952 = ORIENTED_EDGE ( 'NONE', *, *, #48469, .F. ) ;
#11954 = VERTEX_POINT ( 'NONE', #58310 ) ;
#11955 = FACE_OUTER_BOUND ( 'NONE', #11033, .T. ) ;
#11957 = AXIS2_PLACEMENT_3D ( 'NONE', #122360, #51047, #90956 ) ;
#11956 = CIRCLE ( 'NONE', #53720, 5.200000000000000178 ) ;
#11958 = DIRECTION ( 'NONE',  ( 0.000000000000000000, -0.000000000000000000, 1.000000000000000000 ) ) ;
#11959 = DIRECTION ( 'NONE',  ( -0.000000000000000000, -1.000000000000000000, -0.000000000000000000 ) ) ;
#11960 = CARTESIAN_POINT ( 'NONE',  ( -11.24999999999996447, 2.500000000000000000, -2.065063509461098068 ) ) ;
#11961 = DIRECTION ( 'NONE',  ( 0.000000000000000000, -0.9999939076577903929, 0.003490651415223739937 ) ) ;
#11962 = DIRECTION ( 'NONE',  ( 0.000000000000000000, 0.000000000000000000, -1.000000000000000000 ) ) ;
#11963 = VERTEX_POINT ( 'NONE', #68100 ) ;
#11964 = DIRECTION ( 'NONE',  ( 0.000000000000000000, 0.000000000000000000, -1.000000000000000000 ) ) ;
#11965 = EDGE_LOOP ( 'NONE', ( #85121, #33684, #95495, #121589 ) ) ;
#11966 = VERTEX_POINT ( 'NONE', #109976 ) ;
#11967 = VERTEX_POINT ( 'NONE', #99520 ) ;
#11968 = CARTESIAN_POINT ( 'NONE',  ( 185.1979166673494603, 6.668395609140176816, 3.850000000000000977 ) ) ;
#11969 = EDGE_LOOP ( 'NONE', ( #108849, #122761, #40969, #31708 ) ) ;
#11970 = ORIENTED_EDGE ( 'NONE', *, *, #23707, .T. ) ;
#11971 = ORIENTED_EDGE ( 'NONE', *, *, #62139, .F. ) ;
#11972 = CONICAL_SURFACE ( 'NONE', #85125, 0.1000000000000002554, 0.003490658503988666988 ) ;
#11974 = DIRECTION ( 'NONE',  ( 0.000000000000000000, 0.000000000000000000, -1.000000000000000000 ) ) ;
#11973 = AXIS2_PLACEMENT_3D ( 'NONE', #117201, #27543, #108055 ) ;
#11975 = EDGE_CURVE ( 'NONE', #59442, #12555, #128997, .T. ) ;
#11976 =( LENGTH_UNIT ( ) NAMED_UNIT ( * ) SI_UNIT ( .MILLI., .METRE. ) );
#11978 = AXIS2_PLACEMENT_3D ( 'NONE', #6848, #84791, #24582 ) ;
#11977 = DIRECTION ( 'NONE',  ( -0.000000000000000000, 1.000000000000000000, -0.000000000000000000 ) ) ;
#11979 = CARTESIAN_POINT ( 'NONE',  ( 7.049999999999928768, 2.500000000000000000, 6.495190528383297135 ) ) ;
#11980 = DIRECTION ( 'NONE',  ( 0.000000000000000000, 0.000000000000000000, 1.000000000000000000 ) ) ;
#11981 = DIRECTION ( 'NONE',  ( 0.000000000000000000, 0.000000000000000000, 1.000000000000000000 ) ) ;
#11982 = CIRCLE ( 'NONE', #122799, 0.06509327318403745899 ) ;
#11984 = AXIS2_PLACEMENT_3D ( 'NONE', #1772, #2405, #23341 ) ;
#11983 = DIRECTION ( 'NONE',  ( 0.000000000000000000, 0.000000000000000000, 1.000000000000000000 ) ) ;
#11985 = ADVANCED_FACE ( 'NONE', ( #89045 ), #128343, .T. ) ;
#11986 = EDGE_LOOP ( 'NONE', ( #22574, #100256, #80191, #62413 ) ) ;
#11987 = AXIS2_PLACEMENT_3D ( 'NONE', #115156, #63524, #94256 ) ;
#11988 = CIRCLE ( 'NONE', #22485, 0.1000000000000002554 ) ;
#11989 = DIRECTION ( 'NONE',  ( 0.000000000000000000, 0.000000000000000000, -1.000000000000000000 ) ) ;
#11990 = VERTEX_POINT ( 'NONE', #40618 ) ;
#11991 = DIRECTION ( 'NONE',  ( -0.000000000000000000, -1.000000000000000000, -0.000000000000000000 ) ) ;
#11992 = VERTEX_POINT ( 'NONE', #69392 ) ;
#11994 = ADVANCED_FACE ( 'NONE', ( #49782 ), #15464, .T. ) ;
#11993 = DIRECTION ( 'NONE',  ( -4.274815082592931898E-19, -0.9999939076577903929, -0.003490651415223739937 ) ) ;
#11995 = CONICAL_SURFACE ( 'NONE', #78918, 0.09999999999999982514, 0.003490658503988666988 ) ;
#11996 = EDGE_CURVE ( 'NONE', #15907, #78758, #98207, .T. ) ;
#11997 = ORIENTED_EDGE ( 'NONE', *, *, #52602, .T. ) ;
#11998 = LINE ( 'NONE', #53865, #15059 ) ;
#11999 = ADVANCED_FACE ( 'NONE', ( #30140 ), #70051, .T. ) ;
#12000 = CARTESIAN_POINT ( 'NONE',  ( -11.24999999999999822, 2.500000000000000000, 1.372243186433545370 ) ) ;
#12001 = ORIENTED_EDGE ( 'NONE', *, *, #76302, .F. ) ;
#12002 = ORIENTED_EDGE ( 'NONE', *, *, #66404, .T. ) ;
#12003 = CARTESIAN_POINT ( 'NONE',  ( 2.499999999999945377, 12.50000000000000000, 4.957854068765711553 ) ) ;
#12004 = DIRECTION ( 'NONE',  ( 0.000000000000000000, 0.000000000000000000, 1.000000000000000000 ) ) ;
#12005 = ADVANCED_FACE ( 'NONE', ( #70689 ), #110610, .T. ) ;
#12006 = DIRECTION ( 'NONE',  ( 0.000000000000000000, 0.000000000000000000, 1.000000000000000000 ) ) ;
#12007 = FACE_OUTER_BOUND ( 'NONE', #111756, .T. ) ;
#12008 = DIRECTION ( 'NONE',  ( -0.000000000000000000, -1.000000000000000000, -0.000000000000000000 ) ) ;
#12009 = ORIENTED_EDGE ( 'NONE', *, *, #1542, .F. ) ;
#12010 = DIRECTION ( 'NONE',  ( -0.000000000000000000, 1.000000000000000000, -0.000000000000000000 ) ) ;
#12011 = CONICAL_SURFACE ( 'NONE', #72668, 0.1000000000000000472, 0.003490658503988666988 ) ;
#12012 = EDGE_LOOP ( 'NONE', ( #70755, #58312 ) ) ;
#12013 = DIRECTION ( 'NONE',  ( 0.000000000000000000, 1.000000000000000000, 0.000000000000000000 ) ) ;
#12014 = DIRECTION ( 'NONE',  ( 0.000000000000000000, 1.000000000000000000, 0.000000000000000000 ) ) ;
#12015 = DIRECTION ( 'NONE',  ( -0.000000000000000000, -1.000000000000000000, -0.000000000000000000 ) ) ;
#12016 = DIRECTION ( 'NONE',  ( 0.000000000000000000, 1.000000000000000000, 0.000000000000000000 ) ) ;
#12017 = DIRECTION ( 'NONE',  ( -0.000000000000000000, -1.000000000000000000, -0.000000000000000000 ) ) ;
#12018 = DIRECTION ( 'NONE',  ( -0.000000000000000000, -1.000000000000000000, -0.000000000000000000 ) ) ;
#12019 = ORIENTED_EDGE ( 'NONE', *, *, #20201, .F. ) ;
#12020 = CIRCLE ( 'NONE', #24647, 0.06509327318403745899 ) ;
#12021 = CARTESIAN_POINT ( 'NONE',  ( -7.300000000000018474, 12.50000000000000000, 0.2813168883297361700 ) ) ;
#12022 = ADVANCED_FACE ( 'NONE', ( #100159 ), #115728, .T. ) ;
#12023 = VECTOR ( 'NONE', #24427, 1000.000000000000000 ) ;
#12024 = CARTESIAN_POINT ( 'NONE',  ( 1.049999999999954525, 12.50000000000000000, -2.576566944158915184 ) ) ;
#12025 = DIRECTION ( 'NONE',  ( 0.000000000000000000, 1.000000000000000000, 0.000000000000000000 ) ) ;
#12026 = ORIENTED_EDGE ( 'NONE', *, *, #92064, .T. ) ;
#12027 = ORIENTED_EDGE ( 'NONE', *, *, #34644, .F. ) ;
#12029 = ADVANCED_FACE ( 'NONE', ( #30786 ), #30078, .T. ) ;
#12028 = CIRCLE ( 'NONE', #28779, 0.09999999999999982514 ) ;
#12030 = CARTESIAN_POINT ( 'NONE',  ( -10.65000000000000391, 12.50000000000000000, -1.883746621131359600 ) ) ;
#12031 = AXIS2_PLACEMENT_3D ( 'NONE', #85847, #126445, #104843 ) ;
#12032 = ORIENTED_EDGE ( 'NONE', *, *, #92905, .T. ) ;
#12033 = EDGE_LOOP ( 'NONE', ( #66861, #5052, #33704, #126099 ) ) ;
#12034 = CARTESIAN_POINT ( 'NONE',  ( 11.44999999999990870, 2.500000000000000000, 6.841600689897072485 ) ) ;
#12035 = ADVANCED_FACE ( 'NONE', ( #90309 ), #80526, .T. ) ;
#12036 = EDGE_LOOP ( 'NONE', ( #19805, #64911, #84298, #48166 ) ) ;
#12037 = CARTESIAN_POINT ( 'NONE',  ( 0.8499999999999553468, 2.500000000000000000, -2.857883832488653741 ) ) ;
#12038 = DIRECTION ( 'NONE',  ( -0.000000000000000000, 1.000000000000000000, -0.000000000000000000 ) ) ;
#12039 = EDGE_CURVE ( 'NONE', #89331, #55129, #122004, .T. ) ;
#12040 = CARTESIAN_POINT ( 'NONE',  ( 16.72050902516894411, 2.552201582241256705, 5.918448581777647988 ) ) ;
#12042 = EDGE_CURVE ( 'NONE', #72591, #47419, #23805, .T. ) ;
#12041 = CONICAL_SURFACE ( 'NONE', #63998, 0.1000000000000000472, 0.003490658503988666988 ) ;
#12043 = ORIENTED_EDGE ( 'NONE', *, *, #71907, .T. ) ;
#12044 = CIRCLE ( 'NONE', #129061, 0.06509327318403745899 ) ;
#12045 = DIRECTION ( 'NONE',  ( 0.000000000000000000, -0.000000000000000000, 1.000000000000000000 ) ) ;
#12046 = EDGE_CURVE ( 'NONE', #100514, #11992, #34282, .T. ) ;
#12047 = DIRECTION ( 'NONE',  ( 0.000000000000000000, 1.000000000000000000, 0.000000000000000000 ) ) ;
#12048 = AXIS2_PLACEMENT_3D ( 'NONE', #10844, #91364, #33734 ) ;
#12049 = EDGE_LOOP ( 'NONE', ( #89291, #69615 ) ) ;
#12050 = ADVANCED_FACE ( 'NONE', ( #113180 ), #107422, .T. ) ;
#12051 = VECTOR ( 'NONE', #10777, 1000.000000000000000 ) ;
#12052 = EDGE_CURVE ( 'NONE', #27361, #51042, #51006, .T. ) ;
#12053 = ORIENTED_EDGE ( 'NONE', *, *, #23131, .F. ) ;
#12054 = EDGE_LOOP ( 'NONE', ( #67971, #85457, #48828, #3473 ) ) ;
#12055 = DIRECTION ( 'NONE',  ( 0.000000000000000000, 0.000000000000000000, 1.000000000000000000 ) ) ;
#12056 = DIRECTION ( 'NONE',  ( 0.000000000000000000, -0.9999939076577903929, 0.003490651415223739937 ) ) ;
#12057 = DIRECTION ( 'NONE',  ( -0.000000000000000000, -1.000000000000000000, -0.000000000000000000 ) ) ;
#12058 = FACE_BOUND ( 'NONE', #55141, .T. ) ;
#12059 = EDGE_LOOP ( 'NONE', ( #94720, #80895 ) ) ;
#12060 = VECTOR ( 'NONE', #81657, 1000.000000000000000 ) ;
#12061 = DIRECTION ( 'NONE',  ( 0.000000000000000000, 0.000000000000000000, 1.000000000000000000 ) ) ;
#12062 = FACE_OUTER_BOUND ( 'NONE', #50018, .T. ) ;
#12063 = VECTOR ( 'NONE', #8335, 1000.000000000000000 ) ;
#12064 = ORIENTED_EDGE ( 'NONE', *, *, #2256, .T. ) ;
#12065 = DIRECTION ( 'NONE',  ( 0.000000000000000000, 0.000000000000000000, -1.000000000000000000 ) ) ;
#12066 = DIRECTION ( 'NONE',  ( -0.000000000000000000, -1.000000000000000000, -0.000000000000000000 ) ) ;
#12067 = CONICAL_SURFACE ( 'NONE', #127107, 0.09999999999999982514, 0.003490658503988666988 ) ;
#12068 = CARTESIAN_POINT ( 'NONE',  ( -14.39999999999998614, 2.500000000000000000, -0.4464101615137760493 ) ) ;
#12069 = CARTESIAN_POINT ( 'NONE',  ( -3.350000000000032507, 12.50000000000000000, -6.495190528383302464 ) ) ;
#12070 = FACE_OUTER_BOUND ( 'NONE', #60476, .T. ) ;
#12071 = CARTESIAN_POINT ( 'NONE',  ( 8.949999999999919353, 2.500000000000000000, 2.611473670974873151 ) ) ;
#12072 = AXIS2_PLACEMENT_3D ( 'NONE', #55253, #46714, #27705 ) ;
#12073 = DIRECTION ( 'NONE',  ( -4.274815082592931898E-19, -0.9999939076577903929, -0.003490651415223739937 ) ) ;
#12074 = CONICAL_SURFACE ( 'NONE', #89445, 0.1000000000000002554, 0.003490658503988666988 ) ;
#12075 = CONICAL_SURFACE ( 'NONE', #116628, 0.1000000000000000472, 0.003490658503988666988 ) ;
#12076 = ORIENTED_EDGE ( 'NONE', *, *, #9630, .F. ) ;
#12077 = VERTEX_POINT ( 'NONE', #51070 ) ;
#12078 = ORIENTED_EDGE ( 'NONE', *, *, #86, .T. ) ;
#12079 = ORIENTED_EDGE ( 'NONE', *, *, #56090, .T. ) ;
#12080 = CARTESIAN_POINT ( 'NONE',  ( -3.150000000000029221, 2.500000000000000000, -1.918653347947326004 ) ) ;
#12081 = CARTESIAN_POINT ( 'NONE',  ( -5.400000000000024336, 12.50000000000000000, -3.637306695894650055 ) ) ;
#12082 = CONICAL_SURFACE ( 'NONE', #20512, 0.1000000000000000472, 0.003490658503988666988 ) ;
#12083 = ORIENTED_EDGE ( 'NONE', *, *, #51055, .T. ) ;
#12084 = FACE_BOUND ( 'NONE', #51681, .T. ) ;
#12085 = DIRECTION ( 'NONE',  ( 0.000000000000000000, 1.000000000000000000, 0.000000000000000000 ) ) ;
#12086 = CARTESIAN_POINT ( 'NONE',  ( -3.100000000000028955, 2.500000000000000000, 4.083716857408421497 ) ) ;
#12087 = DIRECTION ( 'NONE',  ( -4.274815082592931898E-19, -0.9999939076577903929, -0.003490651415223739937 ) ) ;
#12089 = VECTOR ( 'NONE', #127788, 1000.000000000000000 ) ;
#12088 = CIRCLE ( 'NONE', #93572, 0.1000000000000002554 ) ;
#12090 = DIRECTION ( 'NONE',  ( 0.000000000000000000, 1.000000000000000000, 0.000000000000000000 ) ) ;
#12091 = DIRECTION ( 'NONE',  ( 0.000000000000000000, 1.000000000000000000, 0.000000000000000000 ) ) ;
#12092 = DIRECTION ( 'NONE',  ( 0.000000000000000000, 0.000000000000000000, 1.000000000000000000 ) ) ;
#12093 = LINE ( 'NONE', #102419, #78887 ) ;
#12094 = CARTESIAN_POINT ( 'NONE',  ( -9.400000000000007461, 12.50000000000000000, 0.2813168883297361700 ) ) ;
#12095 = PLANE ( 'NONE',  #68507 ) ;
#12096 = ORIENTED_EDGE ( 'NONE', *, *, #44391, .T. ) ;
#12097 = VERTEX_POINT ( 'NONE', #61531 ) ;
#12098 = EDGE_CURVE ( 'NONE', #46427, #4150, #55196, .T. ) ;
#12099 = ORIENTED_EDGE ( 'NONE', *, *, #94787, .T. ) ;
#12100 = VERTEX_POINT ( 'NONE', #43833 ) ;
#12101 = VERTEX_POINT ( 'NONE', #13689 ) ;
#12102 = EDGE_LOOP ( 'NONE', ( #80291, #14379 ) ) ;
#12103 = EDGE_LOOP ( 'NONE', ( #81593, #41132 ) ) ;
#12104 = CARTESIAN_POINT ( 'NONE',  ( 1.449999999999950440, 2.500000000000000000, 6.248780366869520542 ) ) ;
#12105 = ORIENTED_EDGE ( 'NONE', *, *, #53001, .F. ) ;
#12106 = ORIENTED_EDGE ( 'NONE', *, *, #47238, .F. ) ;
#12107 = CARTESIAN_POINT ( 'NONE',  ( -5.650000000000023448, 12.50000000000000000, -6.906693963081115939 ) ) ;
#12108 = DIRECTION ( 'NONE',  ( 0.000000000000000000, -0.000000000000000000, 1.000000000000000000 ) ) ;
#12109 = CARTESIAN_POINT ( 'NONE',  ( -11.04999999999999893, 2.500000000000000000, 6.148780366869520009 ) ) ;
#12110 = DIRECTION ( 'NONE',  ( -0.000000000000000000, 1.000000000000000000, -0.000000000000000000 ) ) ;
#12111 = AXIS2_PLACEMENT_3D ( 'NONE', #69900, #9684, #127528 ) ;
#12112 = ORIENTED_EDGE ( 'NONE', *, *, #31675, .T. ) ;
#12113 = CARTESIAN_POINT ( 'NONE',  ( 5.399999999999934630, 12.50000000000000000, -0.7579135962115917113 ) ) ;
#12114 = AXIS2_PLACEMENT_3D ( 'NONE', #32288, #110181, #40813 ) ;
#12115 = ORIENTED_EDGE ( 'NONE', *, *, #98332, .T. ) ;
#12116 = AXIS2_PLACEMENT_3D ( 'NONE', #109435, #39434, #107501 ) ;
#12117 = ORIENTED_EDGE ( 'NONE', *, *, #7478, .F. ) ;
#12118 = DIRECTION ( 'NONE',  ( 0.000000000000000000, 1.846105847067148022E-16, -1.000000000000000000 ) ) ;
#12119 = DIRECTION ( 'NONE',  ( 0.000000000000000000, 1.000000000000000000, 0.000000000000000000 ) ) ;
#12120 = EDGE_LOOP ( 'NONE', ( #34585, #111945, #32100, #1480 ) ) ;
#12121 = ORIENTED_EDGE ( 'NONE', *, *, #6829, .F. ) ;
#12122 = DIRECTION ( 'NONE',  ( 0.000000000000000000, 0.000000000000000000, -1.000000000000000000 ) ) ;
#12123 = DIRECTION ( 'NONE',  ( -0.000000000000000000, 1.000000000000000000, -0.000000000000000000 ) ) ;
#12124 = CARTESIAN_POINT ( 'NONE',  ( 0.3999999999999568345, 2.500000000000000000, -3.637306695894650055 ) ) ;
#12125 = CARTESIAN_POINT ( 'NONE',  ( 0.1999999999999567124, 12.50000000000000000, -4.048810130592463530 ) ) ;
#12126 = DIRECTION ( 'NONE',  ( 0.000000000000000000, -0.000000000000000000, 1.000000000000000000 ) ) ;
#12127 = EDGE_LOOP ( 'NONE', ( #5410, #40025 ) ) ;
#12128 = DIRECTION ( 'NONE',  ( 0.000000000000000000, -0.9999939076577903929, 0.003490651415223739937 ) ) ;
#12130 = ADVANCED_FACE ( 'NONE', ( #1936 ), #1299, .T. ) ;
#12129 = CONICAL_SURFACE ( 'NONE', #78969, 0.09999999999999982514, 0.003490658503988666988 ) ;
#12131 = ORIENTED_EDGE ( 'NONE', *, *, #109422, .F. ) ;
#12132 = CARTESIAN_POINT ( 'NONE',  ( 17.50000000000000000, 2.499999999999999556, -2.333333333333329485 ) ) ;
#12133 = PLANE ( 'NONE',  #106958 ) ;
#12134 = DIRECTION ( 'NONE',  ( 0.000000000000000000, 1.000000000000000000, 0.000000000000000000 ) ) ;
#12136 = EDGE_CURVE ( 'NONE', #71261, #30351, #25951, .T. ) ;
#12135 = DIRECTION ( 'NONE',  ( 0.000000000000000000, 1.000000000000000000, 0.000000000000000000 ) ) ;
#12137 = CARTESIAN_POINT ( 'NONE',  ( 8.099999999999923261, 2.500000000000000000, -4.676537180435978769 ) ) ;
#12138 = ADVANCED_FACE ( 'NONE', ( #83737 ), #9224, .T. ) ;
#12139 = ORIENTED_EDGE ( 'NONE', *, *, #98916, .T. ) ;
#12140 = CARTESIAN_POINT ( 'NONE',  ( -3.550000000000027356, 2.500000000000000000, 1.818653347947321475 ) ) ;
#12141 = EDGE_CURVE ( 'NONE', #4440, #55939, #53140, .T. ) ;
#12142 = LINE ( 'NONE', #72386, #21503 ) ;
#12143 = ORIENTED_EDGE ( 'NONE', *, *, #101548, .T. ) ;
#12144 = EDGE_CURVE ( 'NONE', #103611, #63897, #41250, .T. ) ;
#12145 = ORIENTED_EDGE ( 'NONE', *, *, #67235, .F. ) ;
#12146 = VERTEX_POINT ( 'NONE', #71991 ) ;
#12147 = DIRECTION ( 'NONE',  ( -4.274815082592931898E-19, -0.9999939076577903929, -0.003490651415223739937 ) ) ;
#12148 = FACE_OUTER_BOUND ( 'NONE', #27107, .T. ) ;
#12149 = ADVANCED_FACE ( 'NONE', ( #81161 ), #92250, .T. ) ;
#12150 = FILL_AREA_STYLE_COLOUR ( '', #52176 ) ;
#12151 = AXIS2_PLACEMENT_3D ( 'NONE', #80067, #19864, #119995 ) ;
#12153 = CIRCLE ( 'NONE', #47680, 0.1000000000000002554 ) ;
#12152 = DIRECTION ( 'NONE',  ( 0.000000000000000000, -0.9999939076577903929, 0.003490651415223739937 ) ) ;
#12154 = FACE_OUTER_BOUND ( 'NONE', #116426, .T. ) ;
#12155 = VECTOR ( 'NONE', #36842, 1000.000000000000000 ) ;
#12156 = DIRECTION ( 'NONE',  ( -0.000000000000000000, -1.000000000000000000, -0.000000000000000000 ) ) ;
#12157 = DIRECTION ( 'NONE',  ( 0.000000000000000000, -0.9999939076577903929, 0.003490651415223739937 ) ) ;
#12158 = CARTESIAN_POINT ( 'NONE',  ( 12.04999999999990834, 2.500000000000000000, -2.065063509461102065 ) ) ;
#12159 = EDGE_LOOP ( 'NONE', ( #32953, #61186, #119767, #84581 ) ) ;
#12160 = DIRECTION ( 'NONE',  ( -0.000000000000000000, -1.000000000000000000, -0.000000000000000000 ) ) ;
#12161 = DIRECTION ( 'NONE',  ( 0.000000000000000000, 1.000000000000000000, 0.000000000000000000 ) ) ;
#12162 = FACE_OUTER_BOUND ( 'NONE', #58442, .T. ) ;
#12163 = DIRECTION ( 'NONE',  ( 0.000000000000000000, -0.000000000000000000, 1.000000000000000000 ) ) ;
#12164 = EDGE_LOOP ( 'NONE', ( #58186, #120938, #47158, #39150 ) ) ;
#12165 = DIRECTION ( 'NONE',  ( 0.000000000000000000, 0.000000000000000000, -1.000000000000000000 ) ) ;
#12167 = VECTOR ( 'NONE', #64195, 1000.000000000000000 ) ;
#12166 = AXIS2_PLACEMENT_3D ( 'NONE', #126458, #8580, #101346 ) ;
#12168 = DIRECTION ( 'NONE',  ( 0.000000000000000000, 0.000000000000000000, 1.000000000000000000 ) ) ;
#12170 = EDGE_LOOP ( 'NONE', ( #45047, #81907 ) ) ;
#12169 = FACE_OUTER_BOUND ( 'NONE', #98085, .T. ) ;
#12171 = ORIENTED_EDGE ( 'NONE', *, *, #72429, .F. ) ;
#12172 = LINE ( 'NONE', #49557, #107407 ) ;
#12173 = VERTEX_POINT ( 'NONE', #62176 ) ;
#12174 = ORIENTED_EDGE ( 'NONE', *, *, #7889, .T. ) ;
#12175 = CARTESIAN_POINT ( 'NONE',  ( -1.850000000000033396, 12.50000000000000000, -2.511473670974877948 ) ) ;
#12176 = EDGE_CURVE ( 'NONE', #22314, #47889, #115827, .T. ) ;
#12177 = CIRCLE ( 'NONE', #112558, 0.06509327318403745899 ) ;
#12178 = ADVANCED_FACE ( 'NONE', ( #22256 ), #109579, .T. ) ;
#12179 = CARTESIAN_POINT ( 'NONE',  ( 8.949999999999915801, 2.500000000000000000, -1.918653347947326004 ) ) ;
#12181 = ADVANCED_FACE ( 'NONE', ( #122380 ), #42698, .T. ) ;
#12180 = DIRECTION ( 'NONE',  ( 0.000000000000000000, 0.000000000000000000, -1.000000000000000000 ) ) ;
#12182 = CARTESIAN_POINT ( 'NONE',  ( 10.64999999999990976, 12.50000000000000000, -6.148780366869526226 ) ) ;
#12183 = EDGE_LOOP ( 'NONE', ( #19317, #78519, #128891, #67258 ) ) ;
#12184 = VECTOR ( 'NONE', #86386, 1000.000000000000000 ) ;
#12185 = VECTOR ( 'NONE', #57894, 1000.000000000000000 ) ;
#12186 = AXIS2_PLACEMENT_3D ( 'NONE', #25453, #45773, #95503 ) ;
#12187 = AXIS2_PLACEMENT_3D ( 'NONE', #117073, #126275, #75872 ) ;
#12188 = PLANE ( 'NONE',  #37807 ) ;
#12189 = VERTEX_POINT ( 'NONE', #3876 ) ;
#12190 = EDGE_CURVE ( 'NONE', #36385, #240, #102708, .T. ) ;
#12191 = CARTESIAN_POINT ( 'NONE',  ( 17.28959186693766981, 1.567451025700696610, 5.035561754028593739 ) ) ;
#12192 = EDGE_CURVE ( 'NONE', #129191, #46687, #122102, .T. ) ;
#12193 = CARTESIAN_POINT ( 'NONE',  ( -10.45000000000000462, 2.500000000000000000, -2.265063509461097802 ) ) ;
#12195 = EDGE_CURVE ( 'NONE', #101934, #106042, #2968, .T. ) ;
#12194 = CIRCLE ( 'NONE', #56115, 0.06509327318403745899 ) ;
#12196 = ORIENTED_EDGE ( 'NONE', *, *, #3778, .F. ) ;
#12198 = ADVANCED_FACE ( 'NONE', ( #98611 ), #39744, .T. ) ;
#12197 = AXIS2_PLACEMENT_3D ( 'NONE', #110657, #70739, #81833 ) ;
#12199 = AXIS2_PLACEMENT_3D ( 'NONE', #125676, #41138, #72523 ) ;
#12200 = EDGE_CURVE ( 'NONE', #87361, #3965, #49550, .T. ) ;
#12201 = ORIENTED_EDGE ( 'NONE', *, *, #102493, .T. ) ;
#12202 = ORIENTED_EDGE ( 'NONE', *, *, #9839, .T. ) ;
#12203 = ORIENTED_EDGE ( 'NONE', *, *, #28756, .F. ) ;
#12204 = CARTESIAN_POINT ( 'NONE',  ( 108.0000000000000142, 9.000000000000001776, 5.000000000000004441 ) ) ;
#12205 = CARTESIAN_POINT ( 'NONE',  ( 9.399999999999915090, 12.50000000000000000, 4.741630453620009789 ) ) ;
#12206 = CARTESIAN_POINT ( 'NONE',  ( 8.349999999999923261, 2.500000000000000000, -5.702370205355749455 ) ) ;
#12207 = FACE_BOUND ( 'NONE', #48689, .T. ) ;
#12208 = VERTEX_POINT ( 'NONE', #79017 ) ;
#12209 = LINE ( 'NONE', #53918, #41183 ) ;
#12210 = CARTESIAN_POINT ( 'NONE',  ( 185.9895833340161460, -4.445597072760115509, -7.700000000000001954 ) ) ;
#12211 = EDGE_CURVE ( 'NONE', #115574, #98477, #119550, .T. ) ;
#12212 = CIRCLE ( 'NONE', #3814, 0.1000000000000000472 ) ;
#12213 = CARTESIAN_POINT ( 'NONE',  ( -6.249999999999981348, 2.500000000000000000, 6.595190528383296780 ) ) ;
#12214 = DIRECTION ( 'NONE',  ( 0.000000000000000000, 0.000000000000000000, -1.000000000000000000 ) ) ;
#12215 = AXIS2_PLACEMENT_3D ( 'NONE', #31491, #51144, #111307 ) ;
#12216 = CARTESIAN_POINT ( 'NONE',  ( 108.0000000000000142, 5.000000000000000000, 0.000000000000000000 ) ) ;
#12217 = DIRECTION ( 'NONE',  ( 0.000000000000000000, 0.000000000000000000, 1.000000000000000000 ) ) ;
#12218 = PLANE ( 'NONE',  #34542 ) ;
#12219 = AXIS2_PLACEMENT_3D ( 'NONE', #94202, #104028, #43838 ) ;
#12220 = CARTESIAN_POINT ( 'NONE',  ( 7.699999999999922018, 2.500000000000000000, 0.4464101615137735513 ) ) ;
#12221 = VERTEX_POINT ( 'NONE', #80294 ) ;
#12222 = ORIENTED_EDGE ( 'NONE', *, *, #83713, .F. ) ;
#12223 = ORIENTED_EDGE ( 'NONE', *, *, #65859, .F. ) ;
#12224 = CLOSED_SHELL ( 'NONE', ( #21549, #64318, #22970, #9433, #68328, #7736, #72582, #51956, #31701, #107579, #84007, #1136, #95844, #112044, #31528 ) ) ;
#12225 = EDGE_LOOP ( 'NONE', ( #96686, #57614, #127402, #42411 ) ) ;
#12226 = ORIENTED_EDGE ( 'NONE', *, *, #22663, .F. ) ;
#12227 = AXIS2_PLACEMENT_3D ( 'NONE', #67525, #106815, #66895 ) ;
#12228 = DIRECTION ( 'NONE',  ( -0.000000000000000000, 1.000000000000000000, -0.000000000000000000 ) ) ;
#12229 = DIRECTION ( 'NONE',  ( 0.000000000000000000, -0.000000000000000000, 1.000000000000000000 ) ) ;
#12230 = ORIENTED_EDGE ( 'NONE', *, *, #40144, .F. ) ;
#12231 = FACE_BOUND ( 'NONE', #78305, .T. ) ;
#12232 = CARTESIAN_POINT ( 'NONE',  ( 10.19999999999991225, 2.500000000000000000, -4.676537180435978769 ) ) ;
#12233 = AXIS2_PLACEMENT_3D ( 'NONE', #118406, #98118, #119061 ) ;
#12234 = VERTEX_POINT ( 'NONE', #58713 ) ;
#12235 = DIRECTION ( 'NONE',  ( 0.000000000000000000, 0.000000000000000000, -1.000000000000000000 ) ) ;
#12236 = DIRECTION ( 'NONE',  ( 0.000000000000000000, -0.9999939076577903929, 0.003490651415223739937 ) ) ;
#12237 = DIRECTION ( 'NONE',  ( 0.000000000000000000, -0.000000000000000000, 1.000000000000000000 ) ) ;
#12238 = ORIENTED_EDGE ( 'NONE', *, *, #25147, .T. ) ;
#12239 = AXIS2_PLACEMENT_3D ( 'NONE', #60614, #70415, #61245 ) ;
#12240 = LINE ( 'NONE', #101285, #95267 ) ;
#12242 = ORIENTED_EDGE ( 'NONE', *, *, #40430, .T. ) ;
#12241 = AXIS2_PLACEMENT_3D ( 'NONE', #32190, #59718, #72738 ) ;
#12243 = EDGE_CURVE ( 'NONE', #118050, #102673, #29265, .T. ) ;
#12244 = EDGE_LOOP ( 'NONE', ( #43384, #45348, #55426, #88169 ) ) ;
#12245 = VERTEX_POINT ( 'NONE', #57430 ) ;
#12246 = DIRECTION ( 'NONE',  ( 0.000000000000000000, 0.000000000000000000, 1.000000000000000000 ) ) ;
#12247 = CARTESIAN_POINT ( 'NONE',  ( -11.24999999999996447, 2.500000000000000000, -6.495190528383298911 ) ) ;
#12248 = VECTOR ( 'NONE', #70221, 1000.000000000000000 ) ;
#12249 = EDGE_LOOP ( 'NONE', ( #5801, #6411, #118499, #111658 ) ) ;
#12250 = CARTESIAN_POINT ( 'NONE',  ( -5.650000000000023448, 2.500000000000000000, -1.718653347947326049 ) ) ;
#12251 = DIRECTION ( 'NONE',  ( -0.000000000000000000, 1.000000000000000000, -0.000000000000000000 ) ) ;
#12252 = CARTESIAN_POINT ( 'NONE',  ( 12.49999999999990408, 2.500000000000000000, 5.022947341949748790 ) ) ;
#12254 = AXIS2_PLACEMENT_3D ( 'NONE', #103495, #34770, #64842 ) ;
#12253 = CARTESIAN_POINT ( 'NONE',  ( -12.49999999999995737, 2.500000000000000000, 4.330127018922196314 ) ) ;
#12255 = CARTESIAN_POINT ( 'NONE',  ( 186.9062500006828316, -8.891194145520236347, -1.633285867636356693E-15 ) ) ;
#12256 = ORIENTED_EDGE ( 'NONE', *, *, #6353, .F. ) ;
#12257 = AXIS2_PLACEMENT_3D ( 'NONE', #3707, #85497, #72464 ) ;
#12258 = EDGE_CURVE ( 'NONE', #109879, #32296, #38447, .T. ) ;
#12259 = LINE ( 'NONE', #92110, #62114 ) ;
#12260 = ORIENTED_EDGE ( 'NONE', *, *, #91246, .F. ) ;
#12261 = CARTESIAN_POINT ( 'NONE',  ( 1.649999999999949729, 2.500000000000000000, 7.188010851410848723 ) ) ;
#12262 = AXIS2_PLACEMENT_3D ( 'NONE', #88156, #38460, #57443 ) ;
#12263 = VERTEX_POINT ( 'NONE', #70464 ) ;
#12264 = CARTESIAN_POINT ( 'NONE',  ( -11.24999999999999822, 2.500000000000000000, 1.572243186433545548 ) ) ;
#12265 = ORIENTED_EDGE ( 'NONE', *, *, #39128, .T. ) ;
#12266 = DIRECTION ( 'NONE',  ( -0.000000000000000000, -1.000000000000000000, -0.000000000000000000 ) ) ;
#12267 = CARTESIAN_POINT ( 'NONE',  ( -2.100000000000034284, 2.500000000000000000, -4.330127018922201643 ) ) ;
#12268 = DIRECTION ( 'NONE',  ( -0.000000000000000000, -1.000000000000000000, -0.000000000000000000 ) ) ;
#12269 = DIRECTION ( 'NONE',  ( 0.000000000000000000, 0.000000000000000000, 1.000000000000000000 ) ) ;
#12270 = CARTESIAN_POINT ( 'NONE',  ( -6.900000000000019007, 12.50000000000000000, 0.2813168883297361700 ) ) ;
#12271 = ORIENTED_EDGE ( 'NONE', *, *, #85320, .F. ) ;
#12272 = ORIENTED_EDGE ( 'NONE', *, *, #82485, .T. ) ;
#12273 = CARTESIAN_POINT ( 'NONE',  ( 0.000000000000000000, 0.000000000000000000, 6.000000000000005329 ) ) ;
#12274 = CARTESIAN_POINT ( 'NONE',  ( 3.149999999999946176, 12.50000000000000000, -2.511473670974877948 ) ) ;
#12275 = CARTESIAN_POINT ( 'NONE',  ( 8.949999999999917577, 2.500000000000000000, -2.511473670974877948 ) ) ;
#12278 = EDGE_LOOP ( 'NONE', ( #77660, #94393 ) ) ;
#12277 = ORIENTED_EDGE ( 'NONE', *, *, #11583, .T. ) ;
#12276 = CONICAL_SURFACE ( 'NONE', #60438, 0.1000000000000000472, 0.003490658503988666988 ) ;
#12279 = ORIENTED_EDGE ( 'NONE', *, *, #97135, .F. ) ;
#12280 = CARTESIAN_POINT ( 'NONE',  ( -10.00000000000000533, 12.50000000000000000, 5.022947341949748790 ) ) ;
#12281 = ORIENTED_EDGE ( 'NONE', *, *, #101009, .T. ) ;
#12282 = DIRECTION ( 'NONE',  ( 0.000000000000000000, 0.000000000000000000, -1.000000000000000000 ) ) ;
#12283 = CARTESIAN_POINT ( 'NONE',  ( 2.699999999999944666, 12.50000000000000000, 4.741630453620009789 ) ) ;
#12284 = CIRCLE ( 'NONE', #66655, 0.06509327318403745899 ) ;
#12285 = EDGE_CURVE ( 'NONE', #331, #91012, #56756, .T. ) ;
#12287 = CARTESIAN_POINT ( 'NONE',  ( -5.850000000000022737, 12.50000000000000000, -2.165063509461101710 ) ) ;
#12286 = AXIS2_PLACEMENT_3D ( 'NONE', #101025, #40183, #49373 ) ;
#12288 = ORIENTED_EDGE ( 'NONE', *, *, #6779, .T. ) ;
#12289 = DIRECTION ( 'NONE',  ( 0.000000000000000000, 1.000000000000000000, 0.000000000000000000 ) ) ;
#12290 = VECTOR ( 'NONE', #26626, 1000.000000000000000 ) ;
#12291 = DIRECTION ( 'NONE',  ( -0.000000000000000000, 1.000000000000000000, -0.000000000000000000 ) ) ;
#12292 = DIRECTION ( 'NONE',  ( -0.000000000000000000, 1.000000000000000000, -0.000000000000000000 ) ) ;
#12293 = CARTESIAN_POINT ( 'NONE',  ( 14.14999999999989733, 12.50000000000000000, 2.857883832488649301 ) ) ;
#12294 = DIRECTION ( 'NONE',  ( 0.000000000000000000, 0.000000000000000000, 1.000000000000000000 ) ) ;
#12295 = EDGE_CURVE ( 'NONE', #48486, #20699, #59385, .T. ) ;
#12296 = CONICAL_SURFACE ( 'NONE', #100144, 0.09999999999999982514, 0.003490658503988666988 ) ;
#12297 = ORIENTED_EDGE ( 'NONE', *, *, #4938, .F. ) ;
#12298 = AXIS2_PLACEMENT_3D ( 'NONE', #30032, #22152, #62069 ) ;
#12299 = DIRECTION ( 'NONE',  ( 0.000000000000000000, -0.9999939076577903929, 0.003490651415223739937 ) ) ;
#12300 = CARTESIAN_POINT ( 'NONE',  ( 43.06166283080823831, -3.066941195843063017, 4.904920240851240010 ) ) ;
#12301 = EDGE_CURVE ( 'NONE', #59954, #59797, #109753, .T. ) ;
#12302 = EDGE_LOOP ( 'NONE', ( #51723, #15027 ) ) ;
#12303 = EDGE_CURVE ( 'NONE', #43630, #54835, #14891, .T. ) ;
#12304 = ORIENTED_EDGE ( 'NONE', *, *, #54398, .T. ) ;
#12305 = EDGE_CURVE ( 'NONE', #35208, #50586, #50515, .T. ) ;
#12306 = CARTESIAN_POINT ( 'NONE',  ( 184.0677083336747160, -4.367472073101514418, -7.564683531250002702 ) ) ;
#12308 = EDGE_CURVE ( 'NONE', #127093, #86483, #94330, .T. ) ;
#12307 = CARTESIAN_POINT ( 'NONE',  ( -12.04999999999999716, 2.500000000000000000, -6.495190528383298911 ) ) ;
#12309 = ADVANCED_FACE ( 'NONE', ( #99290 ), #9609, .T. ) ;
#12310 = CARTESIAN_POINT ( 'NONE',  ( -5.850000000000021849, 12.50000000000000000, -5.802370205355749988 ) ) ;
#12311 = CIRCLE ( 'NONE', #56217, 0.09999999999999982514 ) ;
#12312 = DIRECTION ( 'NONE',  ( 0.000000000000000000, 1.000000000000000000, 0.000000000000000000 ) ) ;
#12313 = CARTESIAN_POINT ( 'NONE',  ( -12.09999999999999609, 2.500000000000000000, 0.6928203230275535862 ) ) ;
#12314 = CONICAL_SURFACE ( 'NONE', #68749, 0.1000000000000002554, 0.003490658503988666988 ) ;
#12315 = CARTESIAN_POINT ( 'NONE',  ( -3.150000000000029221, 2.500000000000000000, -1.918653347947326004 ) ) ;
#12316 = DIRECTION ( 'NONE',  ( 0.000000000000000000, 0.000000000000000000, 1.000000000000000000 ) ) ;
#12317 = CARTESIAN_POINT ( 'NONE',  ( -12.94999999999999218, 2.500000000000000000, 2.065063509461101621 ) ) ;
#12318 = ADVANCED_FACE ( 'NONE', ( #89460 ), #42127, .T. ) ;
#12320 = EDGE_CURVE ( 'NONE', #45894, #11512, #10788, .T. ) ;
#12319 = CARTESIAN_POINT ( 'NONE',  ( 2.499999999999948930, 12.50000000000000000, -0.6928203230275541413 ) ) ;
#12321 = AXIS2_PLACEMENT_3D ( 'NONE', #24511, #125290, #95825 ) ;
#12322 = ORIENTED_EDGE ( 'NONE', *, *, #64793, .F. ) ;
#12323 = EDGE_CURVE ( 'NONE', #124247, #101388, #118268, .T. ) ;
#12324 = ORIENTED_EDGE ( 'NONE', *, *, #43148, .T. ) ;
#12325 = ORIENTED_EDGE ( 'NONE', *, *, #66981, .F. ) ;
#12326 = AXIS2_PLACEMENT_3D ( 'NONE', #102171, #70772, #91057 ) ;
#12327 = VERTEX_POINT ( 'NONE', #48245 ) ;
#12328 = CARTESIAN_POINT ( 'NONE',  ( 15.79999999999989058, 2.500000000000000000, 0.09999999999999761857 ) ) ;
#12329 = DIRECTION ( 'NONE',  ( -1.000000000000000000, -0.000000000000000000, -0.000000000000000000 ) ) ;
#12330 = ORIENTED_EDGE ( 'NONE', *, *, #100279, .F. ) ;
#12331 = CARTESIAN_POINT ( 'NONE',  ( -1.250000000000037526, 2.500000000000000000, -1.572243186433550211 ) ) ;
#12332 = CIRCLE ( 'NONE', #39565, 0.06509327318403745899 ) ;
#12333 = DIRECTION ( 'NONE',  ( 0.000000000000000000, 1.000000000000000000, 0.000000000000000000 ) ) ;
#12335 = EDGE_LOOP ( 'NONE', ( #125447, #104878, #93490, #60054 ) ) ;
#12334 = LINE ( 'NONE', #96678, #7823 ) ;
#12336 = CARTESIAN_POINT ( 'NONE',  ( -12.29999999999999716, 2.500000000000000000, -3.883716857408423984 ) ) ;
#12337 = CIRCLE ( 'NONE', #54113, 0.1000000000000000472 ) ;
#12338 = FACE_OUTER_BOUND ( 'NONE', #44546, .T. ) ;
#12339 = EDGE_LOOP ( 'NONE', ( #126212, #81232, #101910, #13754 ) ) ;
#12340 = VECTOR ( 'NONE', #90264, 1000.000000000000000 ) ;
#12341 = VERTEX_POINT ( 'NONE', #68523 ) ;
#12342 = EDGE_LOOP ( 'NONE', ( #30328, #114813 ) ) ;
#12343 = ORIENTED_EDGE ( 'NONE', *, *, #94660, .T. ) ;
#12344 = CARTESIAN_POINT ( 'NONE',  ( -10.85000000000000142, 2.500000000000000000, 6.495190528383297135 ) ) ;
#12345 = VECTOR ( 'NONE', #12740, 1000.000000000000000 ) ;
#12346 = CARTESIAN_POINT ( 'NONE',  ( 1.699999999999951994, 2.500000000000000000, 0.09999999999999772959 ) ) ;
#12348 = EDGE_CURVE ( 'NONE', #65138, #74205, #17029, .T. ) ;
#12347 = DIRECTION ( 'NONE',  ( 0.000000000000000000, 1.000000000000000000, 0.000000000000000000 ) ) ;
#12349 = CARTESIAN_POINT ( 'NONE',  ( 2.949999999999946887, 12.50000000000000000, -6.430097255199264339 ) ) ;
#12350 = ORIENTED_EDGE ( 'NONE', *, *, #109024, .T. ) ;
#12351 = EDGE_CURVE ( 'NONE', #2207, #65686, #125717, .T. ) ;
#12352 = AXIS2_PLACEMENT_3D ( 'NONE', #16853, #98657, #85627 ) ;
#12353 = PLANE ( 'NONE',  #85731 ) ;
#12354 = ORIENTED_EDGE ( 'NONE', *, *, #66517, .F. ) ;
#12355 = CARTESIAN_POINT ( 'NONE',  ( -2.050000000000033129, 2.500000000000000000, 6.595190528383296780 ) ) ;
#12357 = CIRCLE ( 'NONE', #118971, 0.1000000000000002554 ) ;
#12356 = CARTESIAN_POINT ( 'NONE',  ( -2.700000000000030376, 2.500000000000000000, 3.883716857408421319 ) ) ;
#12358 = CARTESIAN_POINT ( 'NONE',  ( -11.25000000000000000, 12.50000000000000000, -7.188010851410850499 ) ) ;
#12359 = DIRECTION ( 'NONE',  ( 0.000000000000000000, 0.000000000000000000, 1.000000000000000000 ) ) ;
#12360 = EDGE_CURVE ( 'NONE', #48711, #46223, #121518, .T. ) ;
#12361 = ADVANCED_FACE ( 'NONE', ( #12169 ), #102744, .T. ) ;
#12362 = EDGE_LOOP ( 'NONE', ( #77210, #25191 ) ) ;
#12364 = AXIS2_PLACEMENT_3D ( 'NONE', #34439, #93987, #64514 ) ;
#12363 = CIRCLE ( 'NONE', #4041, 0.1000000000000002554 ) ;
#12365 = EDGE_CURVE ( 'NONE', #102047, #128215, #51481, .T. ) ;
#12366 = VERTEX_POINT ( 'NONE', #52749 ) ;
#12367 = ORIENTED_EDGE ( 'NONE', *, *, #82068, .F. ) ;
#12368 = DIRECTION ( 'NONE',  ( -0.000000000000000000, 1.000000000000000000, -0.000000000000000000 ) ) ;
#12369 = DIRECTION ( 'NONE',  ( 0.000000000000000000, 1.000000000000000000, 0.000000000000000000 ) ) ;
#12370 = CARTESIAN_POINT ( 'NONE',  ( -6.650000000000014566, 12.50000000000000000, 2.165063509461097713 ) ) ;
#12371 = FACE_BOUND ( 'NONE', #59041, .T. ) ;
#12372 = DIRECTION ( 'NONE',  ( 0.000000000000000000, 1.000000000000000000, 0.000000000000000000 ) ) ;
#12373 = DIRECTION ( 'NONE',  ( 0.000000000000000000, 0.000000000000000000, 1.000000000000000000 ) ) ;
#12374 = ADVANCED_FACE ( 'NONE', ( #110383 ), #109000, .T. ) ;
#12375 = PLANE ( 'NONE',  #33220 ) ;
#12376 = VECTOR ( 'NONE', #56518, 1000.000000000000000 ) ;
#12377 = DIRECTION ( 'NONE',  ( 0.000000000000000000, 1.000000000000000000, 0.000000000000000000 ) ) ;
#12378 = DIRECTION ( 'NONE',  ( -0.000000000000000000, -1.000000000000000000, -0.000000000000000000 ) ) ;
#12379 = DIRECTION ( 'NONE',  ( -4.274815082592931898E-19, -0.9999939076577903929, -0.003490651415223739937 ) ) ;
#12380 = VERTEX_POINT ( 'NONE', #42300 ) ;
#12381 = CARTESIAN_POINT ( 'NONE',  ( -2.950000000000029932, 2.500000000000000000, 2.165063509461097713 ) ) ;
#12382 = CIRCLE ( 'NONE', #100220, 0.06509327318403745899 ) ;
#12383 = AXIS2_PLACEMENT_3D ( 'NONE', #42448, #41812, #1852 ) ;
#12384 = CARTESIAN_POINT ( 'NONE',  ( 6.449999999999930012, 12.50000000000000000, 6.841600689897072485 ) ) ;
#12385 = ORIENTED_EDGE ( 'NONE', *, *, #65125, .T. ) ;
#12386 = EDGE_LOOP ( 'NONE', ( #49177, #87405, #77813, #75221 ) ) ;
#12387 = DIRECTION ( 'NONE',  ( -0.000000000000000000, 1.000000000000000000, -0.000000000000000000 ) ) ;
#12388 = CARTESIAN_POINT ( 'NONE',  ( 2.099999999999950351, 2.500000000000000000, -4.230127018922201998 ) ) ;
#12389 = EDGE_CURVE ( 'NONE', #112381, #43111, #69293, .T. ) ;
#12390 = FACE_BOUND ( 'NONE', #87461, .T. ) ;
#12391 = DIRECTION ( 'NONE',  ( 0.000000000000000000, 0.000000000000000000, 1.000000000000000000 ) ) ;
#12392 = AXIS2_PLACEMENT_3D ( 'NONE', #21853, #33599, #4109 ) ;
#12393 = AXIS2_PLACEMENT_3D ( 'NONE', #12436, #91013, #51105 ) ;
#12394 = ORIENTED_EDGE ( 'NONE', *, *, #51603, .T. ) ;
#12395 = FACE_OUTER_BOUND ( 'NONE', #39766, .T. ) ;
#12396 = CARTESIAN_POINT ( 'NONE',  ( 185.3333333333333144, 6.668395609140177704, -3.849999999999998312 ) ) ;
#12397 = ORIENTED_EDGE ( 'NONE', *, *, #6340, .F. ) ;
#12398 = DIRECTION ( 'NONE',  ( 0.000000000000000000, 0.000000000000000000, 1.000000000000000000 ) ) ;
#12399 = CARTESIAN_POINT ( 'NONE',  ( -4.200000000000025935, 2.500000000000000000, 4.330127018922196314 ) ) ;
#12400 = AXIS2_PLACEMENT_3D ( 'NONE', #42806, #13943, #93811 ) ;
#12401 = CIRCLE ( 'NONE', #68846, 0.09999999999999982514 ) ;
#12402 = ADVANCED_FACE ( 'NONE', ( #120853 ), #81819, .T. ) ;
#12403 = VERTEX_POINT ( 'NONE', #80939 ) ;
#12404 = DIRECTION ( 'NONE',  ( 0.000000000000000000, 1.000000000000000000, 0.000000000000000000 ) ) ;
#12405 = CARTESIAN_POINT ( 'NONE',  ( -1.050000000000037348, 2.500000000000000000, -6.841600689897078702 ) ) ;
#12406 = ORIENTED_EDGE ( 'NONE', *, *, #65701, .T. ) ;
#12407 = CARTESIAN_POINT ( 'NONE',  ( 108.0000000000000142, 8.500000000000000000, 2.249999999999996891 ) ) ;
#12408 = DIRECTION ( 'NONE',  ( 0.000000000000000000, 0.000000000000000000, -1.000000000000000000 ) ) ;
#12409 = CARTESIAN_POINT ( 'NONE',  ( -3.550000000000027800, 12.50000000000000000, 6.148780366869520009 ) ) ;
#12410 = VECTOR ( 'NONE', #8939, 1000.000000000000000 ) ;
#12411 = ORIENTED_EDGE ( 'NONE', *, *, #62462, .F. ) ;
#12412 = ORIENTED_EDGE ( 'NONE', *, *, #53378, .T. ) ;
#12413 = EDGE_CURVE ( 'NONE', #126865, #76363, #6571, .T. ) ;
#12414 = DIRECTION ( 'NONE',  ( -0.000000000000000000, 1.000000000000000000, -0.000000000000000000 ) ) ;
#12415 = VERTEX_POINT ( 'NONE', #121480 ) ;
#12416 = DIRECTION ( 'NONE',  ( -4.274815082592931898E-19, -0.9999939076577903929, -0.003490651415223739937 ) ) ;
#12417 = DIRECTION ( 'NONE',  ( -0.000000000000000000, -1.000000000000000000, -0.000000000000000000 ) ) ;
#12418 = DIRECTION ( 'NONE',  ( 0.000000000000000000, 0.000000000000000000, 1.000000000000000000 ) ) ;
#12419 = ORIENTED_EDGE ( 'NONE', *, *, #78521, .F. ) ;
#12420 = CARTESIAN_POINT ( 'NONE',  ( 7.499999999999960032, 2.500000000000000000, -2.276824562219559311E-15 ) ) ;
#12421 = CARTESIAN_POINT ( 'NONE',  ( -1.250000000000037526, 2.500000000000000000, -5.802370205355749988 ) ) ;
#12422 = DIRECTION ( 'NONE',  ( -0.000000000000000000, 1.000000000000000000, -0.000000000000000000 ) ) ;
#12423 = CARTESIAN_POINT ( 'NONE',  ( -10.40000000000000213, 2.500000000000000000, 3.637306695894644726 ) ) ;
#12424 = CARTESIAN_POINT ( 'NONE',  ( -6.850000000000013856, 12.50000000000000000, 2.511473670974873507 ) ) ;
#12425 = AXIS2_PLACEMENT_3D ( 'NONE', #102936, #11977, #2156 ) ;
#12426 = DIRECTION ( 'NONE',  ( 0.000000000000000000, 0.000000000000000000, 1.000000000000000000 ) ) ;
#12427 = ORIENTED_EDGE ( 'NONE', *, *, #91682, .F. ) ;
#12428 = VERTEX_POINT ( 'NONE', #82220 ) ;
#12429 = CARTESIAN_POINT ( 'NONE',  ( -9.800000000000004263, 12.50000000000000000, -0.4115034346978157509 ) ) ;
#12430 = ORIENTED_EDGE ( 'NONE', *, *, #90568, .F. ) ;
#12431 = CARTESIAN_POINT ( 'NONE',  ( 103.2703165085177659, 7.526592624639811824, 1.654927987503729492 ) ) ;
#12433 = EDGE_LOOP ( 'NONE', ( #23643, #62641 ) ) ;
#12432 = ORIENTED_EDGE ( 'NONE', *, *, #105907, .F. ) ;
#12434 = ORIENTED_EDGE ( 'NONE', *, *, #41877, .T. ) ;
#12435 = AXIS2_PLACEMENT_3D ( 'NONE', #98396, #86655, #48676 ) ;
#12436 = CARTESIAN_POINT ( 'NONE',  ( 13.34999999999990017, 2.500000000000000000, 2.165063509461097713 ) ) ;
#12437 = DIRECTION ( 'NONE',  ( 0.000000000000000000, -0.000000000000000000, 1.000000000000000000 ) ) ;
#12438 = DIRECTION ( 'NONE',  ( 0.000000000000000000, 0.000000000000000000, -1.000000000000000000 ) ) ;
#12439 = ADVANCED_FACE ( 'NONE', ( #32503 ), #35862, .T. ) ;
#12441 = CIRCLE ( 'NONE', #83482, 0.1000000000000000472 ) ;
#12440 = AXIS2_PLACEMENT_3D ( 'NONE', #81566, #129411, #22662 ) ;
#12442 = DIRECTION ( 'NONE',  ( -0.000000000000000000, -1.000000000000000000, -0.000000000000000000 ) ) ;
#12443 = CARTESIAN_POINT ( 'NONE',  ( 12.49999999999993960, 12.50000000000000000, -4.330127018922201643 ) ) ;
#12444 = DIRECTION ( 'NONE',  ( 0.000000000000000000, -0.000000000000000000, 1.000000000000000000 ) ) ;
#12445 = LINE ( 'NONE', #121759, #53903 ) ;
#12446 = DIRECTION ( 'NONE',  ( -4.274815082592931898E-19, -0.9999939076577903929, -0.003490651415223739937 ) ) ;
#12447 = CIRCLE ( 'NONE', #22935, 0.1000000000000000472 ) ;
#12448 = DIRECTION ( 'NONE',  ( 0.000000000000000000, 1.000000000000000000, 0.000000000000000000 ) ) ;
#12449 = EDGE_CURVE ( 'NONE', #39786, #49438, #111046, .T. ) ;
#12451 = AXIS2_PLACEMENT_3D ( 'NONE', #105743, #125381, #45542 ) ;
#12450 = CIRCLE ( 'NONE', #58444, 0.09999999999999982514 ) ;
#12452 = ORIENTED_EDGE ( 'NONE', *, *, #87307, .F. ) ;
#12453 = CARTESIAN_POINT ( 'NONE',  ( -4.400000000000028777, 2.500000000000000000, -3.983716857408426293 ) ) ;
#12454 = EDGE_CURVE ( 'NONE', #114896, #57762, #12844, .T. ) ;
#12455 = ORIENTED_EDGE ( 'NONE', *, *, #96496, .T. ) ;
#12456 = EDGE_CURVE ( 'NONE', #26773, #40065, #113209, .T. ) ;
#12457 = ORIENTED_EDGE ( 'NONE', *, *, #56393, .T. ) ;
#12458 = EDGE_CURVE ( 'NONE', #44264, #110118, #53410, .T. ) ;
#12459 = DIRECTION ( 'NONE',  ( -0.000000000000000000, -1.000000000000000000, -0.000000000000000000 ) ) ;
#12461 = EDGE_CURVE ( 'NONE', #22628, #42741, #1072, .T. ) ;
#12460 = CARTESIAN_POINT ( 'NONE',  ( -7.900000000000011013, 2.500000000000000000, 5.022947341949748790 ) ) ;
#12462 = DIRECTION ( 'NONE',  ( 0.000000000000000000, 0.000000000000000000, 1.000000000000000000 ) ) ;
#12463 = DIRECTION ( 'NONE',  ( 0.000000000000000000, 0.000000000000000000, 1.000000000000000000 ) ) ;
#12464 = DIRECTION ( 'NONE',  ( 0.000000000000000000, 1.000000000000000000, 0.000000000000000000 ) ) ;
#12465 = CARTESIAN_POINT ( 'NONE',  ( 8.549999999999920774, 12.50000000000000000, -2.511473670974877948 ) ) ;
#12466 = EDGE_CURVE ( 'NONE', #78026, #125196, #101217, .T. ) ;
#12468 = CIRCLE ( 'NONE', #125347, 0.06509327318403741736 ) ;
#12467 = CARTESIAN_POINT ( 'NONE',  ( -9.150000000000009237, 2.500000000000000000, 2.957883832488649389 ) ) ;
#12469 = VERTEX_POINT ( 'NONE', #31203 ) ;
#12470 = EDGE_CURVE ( 'NONE', #3256, #50948, #71106, .T. ) ;
#12471 = EDGE_CURVE ( 'NONE', #2782, #85021, #21360, .T. ) ;
#12472 = EDGE_CURVE ( 'NONE', #126669, #92740, #91386, .T. ) ;
#12473 = ORIENTED_EDGE ( 'NONE', *, *, #105276, .F. ) ;
#12474 = AXIS2_PLACEMENT_3D ( 'NONE', #104283, #42814, #102359 ) ;
#12475 = EDGE_CURVE ( 'NONE', #123277, #56997, #33799, .T. ) ;
#12477 = VERTEX_POINT ( 'NONE', #125362 ) ;
#12476 = VECTOR ( 'NONE', #4405, 1000.000000000000000 ) ;
#12478 = EDGE_LOOP ( 'NONE', ( #62090, #19174 ) ) ;
#12479 = ORIENTED_EDGE ( 'NONE', *, *, #90400, .T. ) ;
#12480 = EDGE_CURVE ( 'NONE', #942, #27571, #106948, .T. ) ;
#12482 = CONICAL_SURFACE ( 'NONE', #85646, 0.1000000000000002554, 0.003490658503988666988 ) ;
#12481 = CARTESIAN_POINT ( 'NONE',  ( 0.3999999999999568345, 2.500000000000000000, -5.122947341949753763 ) ) ;
#12483 = CARTESIAN_POINT ( 'NONE',  ( -2.700000000000030820, 2.500000000000000000, -4.083716857408426826 ) ) ;
#12485 = CIRCLE ( 'NONE', #14530, 0.1000000000000002554 ) ;
#12484 = CONICAL_SURFACE ( 'NONE', #102380, 0.09999999999999999167, 0.003490658503988666988 ) ;
#12486 = DIRECTION ( 'NONE',  ( -4.274815082592931898E-19, -0.9999939076577903929, -0.003490651415223739937 ) ) ;
#12487 = LINE ( 'NONE', #21678, #46826 ) ;
#12488 = PLANE ( 'NONE',  #15784 ) ;
#12489 = VERTEX_POINT ( 'NONE', #73672 ) ;
#12490 = DIRECTION ( 'NONE',  ( 0.000000000000000000, 0.000000000000000000, -1.000000000000000000 ) ) ;
#12491 = DIRECTION ( 'NONE',  ( 0.000000000000000000, 0.000000000000000000, 1.000000000000000000 ) ) ;
#12492 = DIRECTION ( 'NONE',  ( -4.274815082592931898E-19, -0.9999939076577903929, -0.003490651415223739937 ) ) ;
#12493 = CARTESIAN_POINT ( 'NONE',  ( 3.549999999999941203, 2.500000000000000000, 6.148780366869520897 ) ) ;
#12494 = AXIS2_PLACEMENT_3D ( 'NONE', #78742, #36228, #118633 ) ;
#12495 = CARTESIAN_POINT ( 'NONE',  ( 187.2812500006828031, 0.000000000000000000, 7.700000000000000178 ) ) ;
#12496 = AXIS2_PLACEMENT_3D ( 'NONE', #126494, #67541, #16511 ) ;
#12497 = ORIENTED_EDGE ( 'NONE', *, *, #42204, .F. ) ;
#12498 = VERTEX_POINT ( 'NONE', #56601 ) ;
#12499 = ORIENTED_EDGE ( 'NONE', *, *, #104214, .T. ) ;
#12500 = CARTESIAN_POINT ( 'NONE',  ( 7.899999999999924860, 2.500000000000000000, 5.122947341949749323 ) ) ;
#12501 = ORIENTED_EDGE ( 'NONE', *, *, #89431, .F. ) ;
#12502 = DIRECTION ( 'NONE',  ( 0.000000000000000000, 0.000000000000000000, -1.000000000000000000 ) ) ;
#12503 = PLANE ( 'NONE',  #85742 ) ;
#12504 = CONICAL_SURFACE ( 'NONE', #71015, 0.1000000000000002554, 0.003490658503988666988 ) ;
#12505 = ORIENTED_EDGE ( 'NONE', *, *, #46421, .T. ) ;
#12506 = CARTESIAN_POINT ( 'NONE',  ( 7.099999999999925926, 12.50000000000000000, 0.6928203230275494784 ) ) ;
#12507 = CARTESIAN_POINT ( 'NONE',  ( -3.750000000000029310, 2.500000000000000000, -7.088010851410853519 ) ) ;
#12508 = DIRECTION ( 'NONE',  ( 0.000000000000000000, 1.000000000000000000, 0.000000000000000000 ) ) ;
#12509 = DIRECTION ( 'NONE',  ( 0.000000000000000000, 0.000000000000000000, 1.000000000000000000 ) ) ;
#12510 = ADVANCED_FACE ( 'NONE', ( #14734 ), #117396, .T. ) ;
#12511 = DIRECTION ( 'NONE',  ( 0.000000000000000000, -0.9999939076577903929, 0.003490651415223739937 ) ) ;
#12512 = EDGE_CURVE ( 'NONE', #18199, #114810, #74331, .T. ) ;
#12513 = VERTEX_POINT ( 'NONE', #116174 ) ;
#12514 = ORIENTED_EDGE ( 'NONE', *, *, #66318, .T. ) ;
#12515 = CARTESIAN_POINT ( 'NONE',  ( 0.000000000000000000, 0.000000000000000000, 6.000000000000005329 ) ) ;
#12516 = CARTESIAN_POINT ( 'NONE',  ( -9.400000000000007461, 2.500000000000000000, -0.3464101615137783474 ) ) ;
#12517 = CARTESIAN_POINT ( 'NONE',  ( 9.199999999999915801, 2.500000000000000000, -4.430127018922202176 ) ) ;
#12518 = ADVANCED_FACE ( 'NONE', ( #25212 ), #105729, .T. ) ;
#12519 = CARTESIAN_POINT ( 'NONE',  ( 8.749999999999920064, 2.500000000000000000, -2.957883832488653830 ) ) ;
#12520 = VERTEX_POINT ( 'NONE', #35701 ) ;
#12521 = EDGE_CURVE ( 'NONE', #85590, #3309, #75602, .T. ) ;
#12522 = ORIENTED_EDGE ( 'NONE', *, *, #1805, .T. ) ;
#12524 = CIRCLE ( 'NONE', #27197, 0.1000000000000002554 ) ;
#12523 = CARTESIAN_POINT ( 'NONE',  ( -7.900000000000014566, 2.500000000000000000, -3.537306695894649966 ) ) ;
#12525 = CARTESIAN_POINT ( 'NONE',  ( -4.150000000000024336, 12.50000000000000000, 1.472243186433545459 ) ) ;
#12526 = CARTESIAN_POINT ( 'NONE',  ( 8.949999999999915801, 12.50000000000000000, 6.841600689897072485 ) ) ;
#12527 = CARTESIAN_POINT ( 'NONE',  ( 0.4499999999999569344, 12.50000000000000000, 2.165063509461097713 ) ) ;
#12528 = ORIENTED_EDGE ( 'NONE', *, *, #71468, .T. ) ;
#12529 = DIRECTION ( 'NONE',  ( 0.000000000000000000, 0.000000000000000000, 1.000000000000000000 ) ) ;
#12531 = VECTOR ( 'NONE', #83558, 1000.000000000000000 ) ;
#12530 = AXIS2_PLACEMENT_3D ( 'NONE', #26517, #66429, #18623 ) ;
#12532 = DIRECTION ( 'NONE',  ( 0.000000000000000000, 0.000000000000000000, 1.000000000000000000 ) ) ;
#12533 = ORIENTED_EDGE ( 'NONE', *, *, #60509, .F. ) ;
#12534 = LINE ( 'NONE', #80655, #117965 ) ;
#12535 = ORIENTED_EDGE ( 'NONE', *, *, #103438, .T. ) ;
#12536 = CARTESIAN_POINT ( 'NONE',  ( 4.999999999999935163, 12.50000000000000000, 0.7579135962115869374 ) ) ;
#12537 = CIRCLE ( 'NONE', #10483, 0.1000000000000002554 ) ;
#12538 = ORIENTED_EDGE ( 'NONE', *, *, #29185, .T. ) ;
#12539 = CARTESIAN_POINT ( 'NONE',  ( 8.749999999999921840, 2.500000000000000000, -5.902370205355750521 ) ) ;
#12540 = DIRECTION ( 'NONE',  ( 0.000000000000000000, 0.000000000000000000, 1.000000000000000000 ) ) ;
#12541 = ORIENTED_EDGE ( 'NONE', *, *, #11567, .T. ) ;
#12542 = VERTEX_POINT ( 'NONE', #34427 ) ;
#12543 = DIRECTION ( 'NONE',  ( 0.000000000000000000, 0.000000000000000000, -1.000000000000000000 ) ) ;
#12544 = LINE ( 'NONE', #121864, #24709 ) ;
#12546 = EDGE_CURVE ( 'NONE', #4198, #41152, #125993, .T. ) ;
#12545 = CARTESIAN_POINT ( 'NONE',  ( -4.600000000000024514, 2.500000000000000000, 3.637306695894644726 ) ) ;
#12547 = CARTESIAN_POINT ( 'NONE',  ( 185.6927083336747160, 6.551208109652275624, -3.782341765624998686 ) ) ;
#12548 = LINE ( 'NONE', #70839, #95480 ) ;
#12549 = DIRECTION ( 'NONE',  ( -4.274815082592931898E-19, -0.9999939076577903929, -0.003490651415223739937 ) ) ;
#12550 = DIRECTION ( 'NONE',  ( -4.274815082592931898E-19, -0.9999939076577903929, -0.003490651415223739937 ) ) ;
#12551 = CARTESIAN_POINT ( 'NONE',  ( 2.099999999999947686, 12.50000000000000000, 5.088040615133786027 ) ) ;
#12552 = FACE_OUTER_BOUND ( 'NONE', #22893, .T. ) ;
#12553 = AXIS2_PLACEMENT_3D ( 'NONE', #9377, #36910, #17893 ) ;
#12554 = ORIENTED_EDGE ( 'NONE', *, *, #79038, .F. ) ;
#12555 = VERTEX_POINT ( 'NONE', #46152 ) ;
#12556 = DIRECTION ( 'NONE',  ( -0.000000000000000000, -1.000000000000000000, -0.000000000000000000 ) ) ;
#12557 = ORIENTED_EDGE ( 'NONE', *, *, #119905, .F. ) ;
#12558 = DIRECTION ( 'NONE',  ( -0.000000000000000000, -1.000000000000000000, -0.000000000000000000 ) ) ;
#12559 = CARTESIAN_POINT ( 'NONE',  ( -8.350000000000012079, 12.50000000000000000, 2.857883832488649301 ) ) ;
#12560 = EDGE_CURVE ( 'NONE', #48060, #115619, #93550, .T. ) ;
#12561 = DIRECTION ( 'NONE',  ( 0.000000000000000000, -0.000000000000000000, 1.000000000000000000 ) ) ;
#12563 = ORIENTED_EDGE ( 'NONE', *, *, #80438, .T. ) ;
#12562 = VERTEX_POINT ( 'NONE', #45526 ) ;
#12564 = FACE_BOUND ( 'NONE', #64909, .T. ) ;
#12565 = ORIENTED_EDGE ( 'NONE', *, *, #96526, .T. ) ;
#12566 = EDGE_CURVE ( 'NONE', #4284, #52488, #54667, .T. ) ;
#12567 = CARTESIAN_POINT ( 'NONE',  ( -12.89999999999999147, 2.500000000000000000, 3.637306695894644726 ) ) ;
#12568 = DIRECTION ( 'NONE',  ( 0.000000000000000000, 1.000000000000000000, 0.000000000000000000 ) ) ;
#12569 = AXIS2_PLACEMENT_3D ( 'NONE', #20249, #42484, #60191 ) ;
#12570 = DIRECTION ( 'NONE',  ( 0.000000000000000000, 0.000000000000000000, -1.000000000000000000 ) ) ;
#12571 = DIRECTION ( 'NONE',  ( 0.000000000000000000, 0.000000000000000000, 1.000000000000000000 ) ) ;
#12572 = CARTESIAN_POINT ( 'NONE',  ( -7.500000000000016875, 12.50000000000000000, -3.637306695894650055 ) ) ;
#12573 = FACE_OUTER_BOUND ( 'NONE', #35219, .T. ) ;
#12574 = DIRECTION ( 'NONE',  ( -0.000000000000000000, -1.000000000000000000, -0.000000000000000000 ) ) ;
#12575 = CARTESIAN_POINT ( 'NONE',  ( -8.750000000000010658, 2.500000000000000000, -1.472243186433550122 ) ) ;
#12576 = EDGE_CURVE ( 'NONE', #110135, #80892, #47592, .T. ) ;
#12577 = DIRECTION ( 'NONE',  ( 0.000000000000000000, 0.000000000000000000, 1.000000000000000000 ) ) ;
#12578 = CARTESIAN_POINT ( 'NONE',  ( -7.500000000000013323, 2.500000000000000000, 5.122947341949749323 ) ) ;
#12579 = AXIS2_PLACEMENT_3D ( 'NONE', #99344, #39154, #88869 ) ;
#12580 = DIRECTION ( 'NONE',  ( 0.000000000000000000, -0.9999939076577903929, 0.003490651415223739937 ) ) ;
#12581 = AXIS2_PLACEMENT_3D ( 'NONE', #92347, #112011, #62271 ) ;
#12582 = ORIENTED_EDGE ( 'NONE', *, *, #113846, .F. ) ;
#12583 = VERTEX_POINT ( 'NONE', #105061 ) ;
#12584 = VERTEX_POINT ( 'NONE', #115520 ) ;
#12585 = CARTESIAN_POINT ( 'NONE',  ( -6.650000000000019007, 2.500000000000000000, -1.472243186433550122 ) ) ;
#12586 = VERTEX_POINT ( 'NONE', #65787 ) ;
#12587 = FACE_OUTER_BOUND ( 'NONE', #29336, .T. ) ;
#12588 = CARTESIAN_POINT ( 'NONE',  ( -7.499999999999980460, 2.500000000000000000, 0.09999999999999772959 ) ) ;
#12590 = ORIENTED_EDGE ( 'NONE', *, *, #76516, .F. ) ;
#12589 = ORIENTED_EDGE ( 'NONE', *, *, #123710, .T. ) ;
#12591 = EDGE_LOOP ( 'NONE', ( #122077, #90913, #107403, #35625 ) ) ;
#12592 = PLANE ( 'NONE',  #33373 ) ;
#12593 = AXIS2_PLACEMENT_3D ( 'NONE', #3213, #33956, #1902 ) ;
#12594 = DIRECTION ( 'NONE',  ( 0.000000000000000000, -0.9999939076577903929, 0.003490651415223739937 ) ) ;
#12595 = LINE ( 'NONE', #53196, #101488 ) ;
#12596 = CIRCLE ( 'NONE', #73164, 0.06509327318403745899 ) ;
#12597 = CARTESIAN_POINT ( 'NONE',  ( 8.149999999999923972, 12.50000000000000000, 2.511473670974873507 ) ) ;
#12598 = DIRECTION ( 'NONE',  ( -4.274815082592931898E-19, -0.9999939076577903929, -0.003490651415223739937 ) ) ;
#12599 = EDGE_LOOP ( 'NONE', ( #114201, #78716 ) ) ;
#12600 = DIRECTION ( 'NONE',  ( 0.000000000000000000, 0.000000000000000000, 1.000000000000000000 ) ) ;
#12601 = EDGE_LOOP ( 'NONE', ( #17738, #126446, #42075, #104591 ) ) ;
#12602 = ADVANCED_FACE ( 'NONE', ( #16034 ), #66353, .T. ) ;
#12603 = ORIENTED_EDGE ( 'NONE', *, *, #36725, .F. ) ;
#12604 = ORIENTED_EDGE ( 'NONE', *, *, #18645, .F. ) ;
#12605 = FACE_OUTER_BOUND ( 'NONE', #32055, .T. ) ;
#12606 = EDGE_CURVE ( 'NONE', #120101, #31773, #120737, .T. ) ;
#12607 = VERTEX_POINT ( 'NONE', #86726 ) ;
#12608 = EDGE_CURVE ( 'NONE', #109560, #93720, #97749, .T. ) ;
#12609 = ORIENTED_EDGE ( 'NONE', *, *, #21342, .F. ) ;
#12610 = ADVANCED_FACE ( 'NONE', ( #93973 ), #9927, .T. ) ;
#12611 = ORIENTED_EDGE ( 'NONE', *, *, #43262, .T. ) ;
#12612 = ADVANCED_FACE ( 'NONE', ( #64504 ), #18324, .T. ) ;
#12613 = SURFACE_SIDE_STYLE ('',( #121939 ) ) ;
#12614 = PRESENTATION_STYLE_ASSIGNMENT (( #61086 ) ) ;
#12615 = DIRECTION ( 'NONE',  ( -0.000000000000000000, 1.000000000000000000, -0.000000000000000000 ) ) ;
#12616 = DIRECTION ( 'NONE',  ( 0.000000000000000000, 0.000000000000000000, -1.000000000000000000 ) ) ;
#12617 = PLANE ( 'NONE',  #90910 ) ;
#12618 = EDGE_CURVE ( 'NONE', #27779, #81003, #51795, .T. ) ;
#12619 = VECTOR ( 'NONE', #5523, 1000.000000000000000 ) ;
#12620 = DIRECTION ( 'NONE',  ( -0.000000000000000000, -1.000000000000000000, -0.000000000000000000 ) ) ;
#12621 = CONICAL_SURFACE ( 'NONE', #100458, 0.1000000000000000472, 0.003490658503988666988 ) ;
#12622 = EDGE_CURVE ( 'NONE', #123263, #87808, #99821, .T. ) ;
#12623 = LINE ( 'NONE', #11346, #74190 ) ;
#12624 = VERTEX_POINT ( 'NONE', #27798 ) ;
#12625 = CARTESIAN_POINT ( 'NONE',  ( 11.04999999999991189, 12.50000000000000000, 6.148780366869520897 ) ) ;
#12627 = EDGE_CURVE ( 'NONE', #74873, #119487, #30879, .T. ) ;
#12626 = CIRCLE ( 'NONE', #83658, 0.1000000000000002554 ) ;
#12628 = ORIENTED_EDGE ( 'NONE', *, *, #95906, .T. ) ;
#12629 = DIRECTION ( 'NONE',  ( 0.000000000000000000, 0.000000000000000000, 1.000000000000000000 ) ) ;
#12630 = ORIENTED_EDGE ( 'NONE', *, *, #60865, .T. ) ;
#12631 = CARTESIAN_POINT ( 'NONE',  ( -14.54999999999998472, 2.500000000000000000, -2.165063509461099489 ) ) ;
#12632 = EDGE_CURVE ( 'NONE', #24019, #90957, #76833, .T. ) ;
#12633 = VERTEX_POINT ( 'NONE', #78865 ) ;
#12634 = ADVANCED_FACE ( 'NONE', ( #116822 ), #58571, .T. ) ;
#12635 = CARTESIAN_POINT ( 'NONE',  ( 184.1093750003413732, 9.264065473108010111E-16, -7.564683531250000925 ) ) ;
#12636 = FACE_OUTER_BOUND ( 'NONE', #43915, .T. ) ;
#12637 = ORIENTED_EDGE ( 'NONE', *, *, #74034, .F. ) ;
#12638 = ORIENTED_EDGE ( 'NONE', *, *, #81778, .T. ) ;
#12639 = FACE_OUTER_BOUND ( 'NONE', #72557, .T. ) ;
#12640 = CARTESIAN_POINT ( 'NONE',  ( 129.5000000000000000, 0.000000000000000000, 0.000000000000000000 ) ) ;
#12641 = DIRECTION ( 'NONE',  ( -0.000000000000000000, -1.000000000000000000, -0.000000000000000000 ) ) ;
#12642 = DIRECTION ( 'NONE',  ( 0.000000000000000000, 0.000000000000000000, 1.000000000000000000 ) ) ;
#12643 = DIRECTION ( 'NONE',  ( 0.000000000000000000, -0.9999939076577903929, 0.003490651415223739937 ) ) ;
#12644 = VERTEX_POINT ( 'NONE', #48099 ) ;
#12645 = FACE_OUTER_BOUND ( 'NONE', #50166, .T. ) ;
#12646 = EDGE_LOOP ( 'NONE', ( #63428, #126757 ) ) ;
#12647 = PLANE ( 'NONE',  #82087 ) ;
#12648 = AXIS2_PLACEMENT_3D ( 'NONE', #46610, #49217, #38760 ) ;
#12649 = CARTESIAN_POINT ( 'NONE',  ( 16.56576425165007649, 1.499999999999997113, 6.084390597445792359 ) ) ;
#12650 = AXIS2_PLACEMENT_3D ( 'NONE', #92812, #122270, #104549 ) ;
#12651 = CARTESIAN_POINT ( 'NONE',  ( 187.3385416670080872, 6.551208109652274736, 3.782341765625001351 ) ) ;
#12652 = CARTESIAN_POINT ( 'NONE',  ( -12.29999999999999361, 2.500000000000000000, 3.983716857408420076 ) ) ;
#12653 = CARTESIAN_POINT ( 'NONE',  ( 6.649999999999930189, 2.500000000000000000, 7.188010851410848723 ) ) ;
#12654 = LINE ( 'NONE', #53252, #20950 ) ;
#12655 = DIRECTION ( 'NONE',  ( -0.000000000000000000, -1.000000000000000000, -0.000000000000000000 ) ) ;
#12656 = ORIENTED_EDGE ( 'NONE', *, *, #47476, .T. ) ;
#12657 = AXIS2_PLACEMENT_3D ( 'NONE', #107171, #78386, #27979 ) ;
#12659 = EDGE_CURVE ( 'NONE', #45310, #24791, #39203, .T. ) ;
#12658 = CARTESIAN_POINT ( 'NONE',  ( -1.850000000000033396, 2.500000000000000000, -6.841600689897077814 ) ) ;
#12660 = DIRECTION ( 'NONE',  ( -0.000000000000000000, -1.000000000000000000, -0.000000000000000000 ) ) ;
#12661 = DIRECTION ( 'NONE',  ( -0.000000000000000000, -1.000000000000000000, -0.000000000000000000 ) ) ;
#12662 = ADVANCED_FACE ( 'NONE', ( #38284 ), #24592, .T. ) ;
#12663 = ORIENTED_EDGE ( 'NONE', *, *, #115691, .T. ) ;
#12664 = EDGE_LOOP ( 'NONE', ( #124265, #118232, #71065, #28463 ) ) ;
#12665 = DIRECTION ( 'NONE',  ( 0.000000000000000000, 0.000000000000000000, 1.000000000000000000 ) ) ;
#12666 = CIRCLE ( 'NONE', #39896, 0.06509327318403745899 ) ;
#12667 = CONICAL_SURFACE ( 'NONE', #127614, 0.1000000000000000472, 0.003490658503988666988 ) ;
#12668 = EDGE_LOOP ( 'NONE', ( #52401, #60273, #102475, #108856 ) ) ;
#12669 = PRODUCT_DEFINITION_SHAPE ( 'NONE', 'NONE',  #65974 ) ;
#12670 = ORIENTED_EDGE ( 'NONE', *, *, #12766, .T. ) ;
#12671 = CARTESIAN_POINT ( 'NONE',  ( 165.4999999999999716, 6.123233995736768501E-17, 2.500000000000000000 ) ) ;
#12672 = EDGE_LOOP ( 'NONE', ( #117271, #36574, #59509, #77487 ) ) ;
#12673 = CARTESIAN_POINT ( 'NONE',  ( 20.69433222467976208, -2.585316282074205496, -4.139109617397429552 ) ) ;
#12674 = DIRECTION ( 'NONE',  ( 0.000000000000000000, 0.000000000000000000, 1.000000000000000000 ) ) ;
#12675 = CARTESIAN_POINT ( 'NONE',  ( 19.51231976789225797, 0.5900868802304030103, 4.348342248683020550 ) ) ;
#12676 = AXIS2_PLACEMENT_3D ( 'NONE', #58750, #48938, #109110 ) ;
#12677 = ORIENTED_EDGE ( 'NONE', *, *, #99262, .T. ) ;
#12678 = CARTESIAN_POINT ( 'NONE',  ( -10.20000000000000462, 12.50000000000000000, 4.611443907251934426 ) ) ;
#12679 = CARTESIAN_POINT ( 'NONE',  ( 15.79999999999989058, 12.50000000000000000, 0.06509327318403504425 ) ) ;
#12680 = VECTOR ( 'NONE', #8202, 1000.000000000000000 ) ;
#12681 = EDGE_LOOP ( 'NONE', ( #2406, #115928, #39495, #11120 ) ) ;
#12682 = ORIENTED_EDGE ( 'NONE', *, *, #72496, .F. ) ;
#12683 = EDGE_LOOP ( 'NONE', ( #12019, #62559 ) ) ;
#12684 = LINE ( 'NONE', #120725, #56668 ) ;
#12685 = CARTESIAN_POINT ( 'NONE',  ( 3.349999999999941025, 12.50000000000000000, 7.188010851410848723 ) ) ;
#12686 = DIRECTION ( 'NONE',  ( 0.000000000000000000, 1.000000000000000000, 0.000000000000000000 ) ) ;
#12687 = FACE_BOUND ( 'NONE', #5639, .T. ) ;
#12688 = ORIENTED_EDGE ( 'NONE', *, *, #99674, .F. ) ;
#12689 = CARTESIAN_POINT ( 'NONE',  ( 8.949999999999921130, 2.500000000000000000, 1.818653347947321475 ) ) ;
#12690 = DIRECTION ( 'NONE',  ( -0.000000000000000000, 1.000000000000000000, -0.000000000000000000 ) ) ;
#12691 = EDGE_LOOP ( 'NONE', ( #88494, #5179 ) ) ;
#12693 = ADVANCED_FACE ( 'NONE', ( #27161 ), #99135, .T. ) ;
#12692 = DIRECTION ( 'NONE',  ( 0.000000000000000000, -0.9999939076577903929, 0.003490651415223739937 ) ) ;
#12694 = DIRECTION ( 'NONE',  ( 0.000000000000000000, 0.000000000000000000, 1.000000000000000000 ) ) ;
#12695 = MANIFOLD_SOLID_BREP ( 'Cavity1', #56137 ) ;
#12696 = CARTESIAN_POINT ( 'NONE',  ( -3.150000000000029221, 12.50000000000000000, -1.818653347947326138 ) ) ;
#12697 = FACE_OUTER_BOUND ( 'NONE', #51202, .T. ) ;
#12698 = DIRECTION ( 'NONE',  ( 0.000000000000000000, 1.000000000000000000, 0.000000000000000000 ) ) ;
#12699 = AXIS2_PLACEMENT_3D ( 'NONE', #42778, #93145, #81398 ) ;
#12700 = CONICAL_SURFACE ( 'NONE', #48231, 0.1000000000000002554, 0.003490658503988666988 ) ;
#12701 = CARTESIAN_POINT ( 'NONE',  ( -3.300000000000028244, 2.500000000000000000, 4.330127018922196314 ) ) ;
#12702 = DIRECTION ( 'NONE',  ( 0.000000000000000000, 0.000000000000000000, 1.000000000000000000 ) ) ;
#12703 = EDGE_CURVE ( 'NONE', #124476, #84951, #106071, .T. ) ;
#12704 = CONICAL_SURFACE ( 'NONE', #100461, 0.1000000000000000056, 0.003490658503988666988 ) ;
#12705 = EDGE_LOOP ( 'NONE', ( #84564, #71154, #60604 ) ) ;
#12706 = VERTEX_POINT ( 'NONE', #19933 ) ;
#12707 = ORIENTED_EDGE ( 'NONE', *, *, #18228, .F. ) ;
#12708 = VERTEX_POINT ( 'NONE', #127943 ) ;
#12709 = CARTESIAN_POINT ( 'NONE',  ( -13.54999999999999005, 12.50000000000000000, -1.818653347947323917 ) ) ;
#12710 = CARTESIAN_POINT ( 'NONE',  ( -6.450000000000017941, 2.500000000000000000, -6.841600689897077814 ) ) ;
#12712 = EDGE_CURVE ( 'NONE', #25509, #122967, #41343, .T. ) ;
#12711 = CONICAL_SURFACE ( 'NONE', #46177, 0.1000000000000002554, 0.003490658503988666988 ) ;
#12713 = DIRECTION ( 'NONE',  ( -0.000000000000000000, 1.000000000000000000, -0.000000000000000000 ) ) ;
#12714 = EDGE_LOOP ( 'NONE', ( #85743, #107287 ) ) ;
#12715 = FACE_BOUND ( 'NONE', #1588, .T. ) ;
#12716 = EDGE_CURVE ( 'NONE', #105608, #43127, #70560, .T. ) ;
#12717 = CARTESIAN_POINT ( 'NONE',  ( -1.850000000000033396, 12.50000000000000000, -6.148780366869526226 ) ) ;
#12718 = DIRECTION ( 'NONE',  ( 0.000000000000000000, 1.000000000000000000, 0.000000000000000000 ) ) ;
#12719 = LINE ( 'NONE', #112234, #105599 ) ;
#12720 = CARTESIAN_POINT ( 'NONE',  ( 11.64999999999990443, 12.50000000000000000, -7.188010851410854052 ) ) ;
#12721 = CARTESIAN_POINT ( 'NONE',  ( 7.099999999999925926, 12.50000000000000000, 0.6277270498435120194 ) ) ;
#12722 = CARTESIAN_POINT ( 'NONE',  ( 185.4166666666666856, 6.668395609140176816, 3.850000000000000977 ) ) ;
#12723 = CARTESIAN_POINT ( 'NONE',  ( 12.49999999999990408, 2.500000000000000000, -3.537306695894649966 ) ) ;
#12724 = FACE_OUTER_BOUND ( 'NONE', #8167, .T. ) ;
#12725 = EDGE_CURVE ( 'NONE', #119819, #19084, #68370, .T. ) ;
#12726 = CARTESIAN_POINT ( 'NONE',  ( 6.249999999999930722, 2.500000000000000000, 1.472243186433545459 ) ) ;
#12727 = ORIENTED_EDGE ( 'NONE', *, *, #101038, .F. ) ;
#12728 = AXIS2_PLACEMENT_3D ( 'NONE', #56842, #47061, #126255 ) ;
#12729 = ORIENTED_EDGE ( 'NONE', *, *, #24437, .F. ) ;
#12730 = EDGE_LOOP ( 'NONE', ( #55631, #86431, #69249, #56418 ) ) ;
#12731 = ORIENTED_EDGE ( 'NONE', *, *, #124485, .F. ) ;
#12732 = ORIENTED_EDGE ( 'NONE', *, *, #82404, .T. ) ;
#12733 = ORIENTED_EDGE ( 'NONE', *, *, #63430, .F. ) ;
#12734 = LINE ( 'NONE', #40291, #94467 ) ;
#12735 = ORIENTED_EDGE ( 'NONE', *, *, #106988, .F. ) ;
#12736 = VERTEX_POINT ( 'NONE', #57272 ) ;
#12737 = VECTOR ( 'NONE', #111155, 1000.000000000000000 ) ;
#12738 = AXIS2_PLACEMENT_3D ( 'NONE', #52712, #92640, #3616 ) ;
#12739 = FACE_OUTER_BOUND ( 'NONE', #110728, .T. ) ;
#12740 = DIRECTION ( 'NONE',  ( 0.000000000000000000, -0.9999939076577903929, 0.003490651415223739937 ) ) ;
#12741 = DIRECTION ( 'NONE',  ( -4.274815082592931898E-19, -0.9999939076577903929, -0.003490651415223739937 ) ) ;
#12742 = ORIENTED_EDGE ( 'NONE', *, *, #120350, .F. ) ;
#12743 = DIRECTION ( 'NONE',  ( -0.000000000000000000, 1.000000000000000000, -0.000000000000000000 ) ) ;
#12744 = AXIS2_PLACEMENT_3D ( 'NONE', #26849, #96866, #55659 ) ;
#12745 = CIRCLE ( 'NONE', #31551, 0.06509327318403745899 ) ;
#12746 = EDGE_LOOP ( 'NONE', ( #65342, #85770, #82161, #94063 ) ) ;
#12747 = ADVANCED_FACE ( 'NONE', ( #91244 ), #42144, .T. ) ;
#12748 = VERTEX_POINT ( 'NONE', #32985 ) ;
#12749 = CARTESIAN_POINT ( 'NONE',  ( 3.149999999999942624, 2.500000000000000000, 6.841600689897072485 ) ) ;
#12750 = DIRECTION ( 'NONE',  ( 0.000000000000000000, 0.000000000000000000, 1.000000000000000000 ) ) ;
#12751 = EDGE_CURVE ( 'NONE', #121932, #20597, #122794, .T. ) ;
#12752 = VERTEX_POINT ( 'NONE', #40215 ) ;
#12754 = EDGE_CURVE ( 'NONE', #100839, #47341, #43398, .T. ) ;
#12753 = ORIENTED_EDGE ( 'NONE', *, *, #98019, .F. ) ;
#12755 = AXIS2_PLACEMENT_3D ( 'NONE', #37951, #100101, #89633 ) ;
#12756 = DIRECTION ( 'NONE',  ( 0.000000000000000000, 0.000000000000000000, 1.000000000000000000 ) ) ;
#12757 = AXIS2_PLACEMENT_3D ( 'NONE', #43001, #122821, #99961 ) ;
#12758 = DIRECTION ( 'NONE',  ( -0.000000000000000000, -1.000000000000000000, -0.000000000000000000 ) ) ;
#12759 = CARTESIAN_POINT ( 'NONE',  ( 1.699999999999951994, 2.500000000000000000, 0.09999999999999772959 ) ) ;
#12760 = FACE_OUTER_BOUND ( 'NONE', #48640, .T. ) ;
#12761 = EDGE_CURVE ( 'NONE', #89951, #37339, #116524, .T. ) ;
#12762 = EDGE_CURVE ( 'NONE', #55354, #16720, #110863, .T. ) ;
#12763 = FACE_OUTER_BOUND ( 'NONE', #102474, .T. ) ;
#12764 = ADVANCED_FACE ( 'NONE', ( #72894 ), #60514, .T. ) ;
#12766 = EDGE_CURVE ( 'NONE', #17565, #88843, #108213, .T. ) ;
#12765 = CONICAL_SURFACE ( 'NONE', #71353, 0.1000000000000002554, 0.003490658503988666988 ) ;
#12767 = EDGE_LOOP ( 'NONE', ( #26867, #5617, #30942, #60544 ) ) ;
#12768 = CARTESIAN_POINT ( 'NONE',  ( 4.849235612580096166, -2.499999999999999112, 8.943930330244963756 ) ) ;
#12769 = EDGE_LOOP ( 'NONE', ( #108321, #96886 ) ) ;
#12770 = DIRECTION ( 'NONE',  ( -4.274815082592931898E-19, -0.9999939076577903929, -0.003490651415223739937 ) ) ;
#12771 = ADVANCED_FACE ( 'NONE', ( #10718 ), #82731, .T. ) ;
#12772 = CARTESIAN_POINT ( 'NONE',  ( 6.249999999999967137, 2.500000000000000000, -2.165063509461101710 ) ) ;
#12773 = AXIS2_PLACEMENT_3D ( 'NONE', #78262, #99829, #10150 ) ;
#12774 = AXIS2_PLACEMENT_3D ( 'NONE', #68485, #7623, #126120 ) ;
#12775 = FACE_OUTER_BOUND ( 'NONE', #20598, .T. ) ;
#12776 = LINE ( 'NONE', #61913, #38291 ) ;
#12777 = PLANE ( 'NONE',  #123298 ) ;
#12778 = ORIENTED_EDGE ( 'NONE', *, *, #123318, .F. ) ;
#12779 = ADVANCED_FACE ( 'NONE', ( #52598 ), #7954, .T. ) ;
#12780 = PLANE ( 'NONE',  #46783 ) ;
#12781 = FACE_OUTER_BOUND ( 'NONE', #12591, .T. ) ;
#12782 = ORIENTED_EDGE ( 'NONE', *, *, #6397, .F. ) ;
#12783 = EDGE_LOOP ( 'NONE', ( #31804, #120980 ) ) ;
#12784 = ORIENTED_EDGE ( 'NONE', *, *, #11639, .T. ) ;
#12785 = CARTESIAN_POINT ( 'NONE',  ( -13.09999999999999254, 2.500000000000000000, -4.676537180435975216 ) ) ;
#12786 = DIRECTION ( 'NONE',  ( 0.000000000000000000, -0.000000000000000000, 1.000000000000000000 ) ) ;
#12787 = CARTESIAN_POINT ( 'NONE',  ( 186.1927083336747160, 6.551208109652275624, -3.782341765624998686 ) ) ;
#12788 = LINE ( 'NONE', #101837, #107627 ) ;
#12789 = LINE ( 'NONE', #92661, #11032 ) ;
#12790 = CARTESIAN_POINT ( 'NONE',  ( 5.449999999999937117, 2.500000000000000000, -6.495190528383302464 ) ) ;
#12791 = DIRECTION ( 'NONE',  ( 0.000000000000000000, 0.000000000000000000, -1.000000000000000000 ) ) ;
#12792 = AXIS2_PLACEMENT_3D ( 'NONE', #124365, #71369, #53685 ) ;
#12793 = AXIS2_PLACEMENT_3D ( 'NONE', #7964, #49849, #39398 ) ;
#12794 = AXIS2_PLACEMENT_3D ( 'NONE', #72844, #92474, #82010 ) ;
#12795 = CARTESIAN_POINT ( 'NONE',  ( 4.599999999999939249, 2.500000000000000000, -3.737306695894649700 ) ) ;
#12796 = AXIS2_PLACEMENT_3D ( 'NONE', #97278, #7601, #108386 ) ;
#12797 = ORIENTED_EDGE ( 'NONE', *, *, #10165, .T. ) ;
#12798 = PLANE ( 'NONE',  #8817 ) ;
#12799 = CIRCLE ( 'NONE', #75504, 0.1000000000000000472 ) ;
#12800 = DIRECTION ( 'NONE',  ( 0.000000000000000000, 0.000000000000000000, 1.000000000000000000 ) ) ;
#12801 = LINE ( 'NONE', #113603, #67273 ) ;
#12802 = DIRECTION ( 'NONE',  ( -0.000000000000000000, 1.000000000000000000, -0.000000000000000000 ) ) ;
#12803 = ORIENTED_EDGE ( 'NONE', *, *, #47964, .T. ) ;
#12804 = DIRECTION ( 'NONE',  ( 0.000000000000000000, 0.000000000000000000, 1.000000000000000000 ) ) ;
#12805 = EDGE_CURVE ( 'NONE', #72699, #78169, #66441, .T. ) ;
#12806 = FACE_OUTER_BOUND ( 'NONE', #8709, .T. ) ;
#12808 = ORIENTED_EDGE ( 'NONE', *, *, #72062, .T. ) ;
#12807 = DIRECTION ( 'NONE',  ( -4.274815082592931898E-19, -0.9999939076577903929, -0.003490651415223739937 ) ) ;
#12809 = ORIENTED_EDGE ( 'NONE', *, *, #110170, .T. ) ;
#12810 = CARTESIAN_POINT ( 'NONE',  ( -6.050000000000018474, 2.500000000000000000, 2.411473670974873862 ) ) ;
#12811 = EDGE_CURVE ( 'NONE', #71464, #106656, #72718, .T. ) ;
#12812 = EDGE_LOOP ( 'NONE', ( #95821, #61386 ) ) ;
#12813 = EDGE_LOOP ( 'NONE', ( #69645, #114652, #16410, #104519 ) ) ;
#12814 = CARTESIAN_POINT ( 'NONE',  ( -9.350000000000008527, 2.500000000000000000, -6.248780366869521430 ) ) ;
#12815 = CARTESIAN_POINT ( 'NONE',  ( 16.09541403888750821, 2.463474929527661228, -3.723514363709292230 ) ) ;
#12816 = FACE_OUTER_BOUND ( 'NONE', #96765, .T. ) ;
#12817 = DIRECTION ( 'NONE',  ( 0.000000000000000000, 0.000000000000000000, -1.000000000000000000 ) ) ;
#12818 = AXIS2_PLACEMENT_3D ( 'NONE', #44367, #54825, #115031 ) ;
#12819 = ORIENTED_EDGE ( 'NONE', *, *, #71286, .F. ) ;
#12820 = AXIS2_PLACEMENT_3D ( 'NONE', #107617, #86015, #45491 ) ;
#12821 = DIRECTION ( 'NONE',  ( -0.000000000000000000, 1.000000000000000000, -0.000000000000000000 ) ) ;
#12823 = VERTEX_POINT ( 'NONE', #101061 ) ;
#12822 = CARTESIAN_POINT ( 'NONE',  ( -2.500000000000032419, 2.500000000000000000, -3.637306695894650055 ) ) ;
#12824 = DIRECTION ( 'NONE',  ( -4.274815082592931898E-19, -0.9999939076577903929, -0.003490651415223739937 ) ) ;
#12825 = CARTESIAN_POINT ( 'NONE',  ( -15.39999999999997904, 12.50000000000000000, 0.000000000000000000 ) ) ;
#12826 = CONICAL_SURFACE ( 'NONE', #77684, 0.1000000000000002554, 0.003490658503988666988 ) ;
#12827 = EDGE_LOOP ( 'NONE', ( #110677, #52022, #29077, #115494 ) ) ;
#12828 = AXIS2_PLACEMENT_3D ( 'NONE', #77197, #105366, #117737 ) ;
#12829 = ORIENTED_EDGE ( 'NONE', *, *, #111132, .F. ) ;
#12830 = ORIENTED_EDGE ( 'NONE', *, *, #113883, .F. ) ;
#12831 = VERTEX_POINT ( 'NONE', #31678 ) ;
#12832 = DIRECTION ( 'NONE',  ( 0.000000000000000000, 0.000000000000000000, 1.000000000000000000 ) ) ;
#12833 = CARTESIAN_POINT ( 'NONE',  ( 12.65326442544382601, 1.500000000000126121, 8.428886915957018999 ) ) ;
#12834 = DIRECTION ( 'NONE',  ( 0.000000000000000000, 1.000000000000000000, 0.000000000000000000 ) ) ;
#12835 = FACE_BOUND ( 'NONE', #75695, .T. ) ;
#12836 = ORIENTED_EDGE ( 'NONE', *, *, #55600, .F. ) ;
#12837 = CARTESIAN_POINT ( 'NONE',  ( 184.3645833340161175, -6.668395609140180369, 3.849999999999994760 ) ) ;
#12838 = DIRECTION ( 'NONE',  ( -1.000000000000000000, 0.000000000000000000, 0.000000000000000000 ) ) ;
#12839 = DIRECTION ( 'NONE',  ( 0.000000000000000000, 0.000000000000000000, -1.000000000000000000 ) ) ;
#12840 = CIRCLE ( 'NONE', #94326, 0.06509327318403745899 ) ;
#12841 = AXIS2_PLACEMENT_3D ( 'NONE', #53195, #16452, #28730 ) ;
#12842 = CONICAL_SURFACE ( 'NONE', #92277, 0.1000000000000002554, 0.003490658503988666988 ) ;
#12843 = EDGE_CURVE ( 'NONE', #105744, #89132, #83192, .T. ) ;
#12844 = CIRCLE ( 'NONE', #127795, 0.1000000000000000056 ) ;
#12845 = DIRECTION ( 'NONE',  ( 0.000000000000000000, 0.000000000000000000, 1.000000000000000000 ) ) ;
#12846 = CARTESIAN_POINT ( 'NONE',  ( 0.5999999999999612310, 12.50000000000000000, -0.3464101615137760715 ) ) ;
#12847 = CARTESIAN_POINT ( 'NONE',  ( 11.69999999999990870, 2.500000000000000000, -4.230127018922201998 ) ) ;
#12848 = AXIS2_PLACEMENT_3D ( 'NONE', #38986, #38314, #99166 ) ;
#12849 = EDGE_CURVE ( 'NONE', #4351, #91437, #92523, .T. ) ;
#12850 = PLANE ( 'NONE',  #93429 ) ;
#12851 = ORIENTED_EDGE ( 'NONE', *, *, #54688, .F. ) ;
#12852 = VECTOR ( 'NONE', #41404, 1000.000000000000000 ) ;
#12853 = VECTOR ( 'NONE', #105024, 1000.000000000000000 ) ;
#12854 = ORIENTED_EDGE ( 'NONE', *, *, #121851, .T. ) ;
#12855 = EDGE_LOOP ( 'NONE', ( #101725, #13205 ) ) ;
#12856 = ORIENTED_EDGE ( 'NONE', *, *, #74995, .F. ) ;
#12857 = EDGE_LOOP ( 'NONE', ( #80320, #42275, #67492, #84474 ) ) ;
#12858 = DIRECTION ( 'NONE',  ( 0.000000000000000000, -0.000000000000000000, 1.000000000000000000 ) ) ;
#12859 = ADVANCED_FACE ( 'NONE', ( #121338 ), #12067, .T. ) ;
#12860 = DIRECTION ( 'NONE',  ( 0.000000000000000000, 1.000000000000000000, 0.000000000000000000 ) ) ;
#12861 = EDGE_LOOP ( 'NONE', ( #129108, #27964, #53069, #114743 ) ) ;
#12862 = FACE_BOUND ( 'NONE', #26514, .T. ) ;
#12863 = EDGE_CURVE ( 'NONE', #60734, #50580, #3756, .T. ) ;
#12864 = CARTESIAN_POINT ( 'NONE',  ( 12.04999999999990834, 2.500000000000000000, 6.495190528383297135 ) ) ;
#12865 = EDGE_CURVE ( 'NONE', #124, #100363, #14205, .T. ) ;
#12866 = ORIENTED_EDGE ( 'NONE', *, *, #122875, .T. ) ;
#12867 = CARTESIAN_POINT ( 'NONE',  ( -4.200000000000025935, 12.50000000000000000, -0.06509327318403980434 ) ) ;
#12868 = DIRECTION ( 'NONE',  ( 0.000000000000000000, 0.000000000000000000, -1.000000000000000000 ) ) ;
#12869 = EDGE_CURVE ( 'NONE', #7967, #81575, #104108, .T. ) ;
#12870 = DIRECTION ( 'NONE',  ( 0.000000000000000000, 0.000000000000000000, -1.000000000000000000 ) ) ;
#12871 = EDGE_LOOP ( 'NONE', ( #119711, #42935 ) ) ;
#12872 = PLANE ( 'NONE',  #7414 ) ;
#12873 = ORIENTED_EDGE ( 'NONE', *, *, #21395, .F. ) ;
#12874 = ORIENTED_EDGE ( 'NONE', *, *, #58870, .F. ) ;
#12875 = CIRCLE ( 'NONE', #4550, 0.06509327318403745899 ) ;
#12876 = EDGE_LOOP ( 'NONE', ( #64429, #108536, #82258, #95703 ) ) ;
#12877 = AXIS2_PLACEMENT_3D ( 'NONE', #57410, #127444, #117584 ) ;
#12878 = DIRECTION ( 'NONE',  ( -0.000000000000000000, 1.000000000000000000, -0.000000000000000000 ) ) ;
#12879 = DIRECTION ( 'NONE',  ( 0.000000000000000000, 1.000000000000000000, 0.000000000000000000 ) ) ;
#12880 = DIRECTION ( 'NONE',  ( 0.000000000000000000, 0.000000000000000000, -1.000000000000000000 ) ) ;
#12881 = ORIENTED_EDGE ( 'NONE', *, *, #30183, .T. ) ;
#12882 = DIRECTION ( 'NONE',  ( 0.000000000000000000, 0.000000000000000000, 1.000000000000000000 ) ) ;
#12883 = CARTESIAN_POINT ( 'NONE',  ( -1.250000000000001554, 2.500000000000000000, 2.265063509461097357 ) ) ;
#12884 = AXIS2_PLACEMENT_3D ( 'NONE', #25388, #16206, #37176 ) ;
#12885 = AXIS2_PLACEMENT_3D ( 'NONE', #50765, #42239, #62530 ) ;
#12886 = CARTESIAN_POINT ( 'NONE',  ( 3.149999999999944400, 12.50000000000000000, 2.446380397790835826 ) ) ;
#12887 = CARTESIAN_POINT ( 'NONE',  ( 186.7812500006828031, 0.000000000000000000, 7.700000000000000178 ) ) ;
#12888 = ORIENTED_EDGE ( 'NONE', *, *, #52411, .F. ) ;
#12889 = AXIS2_PLACEMENT_3D ( 'NONE', #10183, #50121, #122076 ) ;
#12890 = AXIS2_PLACEMENT_3D ( 'NONE', #73520, #71598, #21872 ) ;
#12891 = DIRECTION ( 'NONE',  ( 0.000000000000000000, 0.000000000000000000, 1.000000000000000000 ) ) ;
#12892 = ORIENTED_EDGE ( 'NONE', *, *, #12042, .F. ) ;
#12893 = DIRECTION ( 'NONE',  ( 0.000000000000000000, 1.000000000000000000, 0.000000000000000000 ) ) ;
#12894 = AXIS2_PLACEMENT_3D ( 'NONE', #33812, #66485, #113665 ) ;
#12895 = EDGE_LOOP ( 'NONE', ( #49454, #17572 ) ) ;
#12896 = EDGE_LOOP ( 'NONE', ( #62833, #995, #126214, #11628 ) ) ;
#12897 = FACE_OUTER_BOUND ( 'NONE', #69951, .T. ) ;
#12898 = DIRECTION ( 'NONE',  ( 0.000000000000000000, 0.000000000000000000, 1.000000000000000000 ) ) ;
#12899 = DIRECTION ( 'NONE',  ( 0.000000000000000000, 1.000000000000000000, 0.000000000000000000 ) ) ;
#12900 = LINE ( 'NONE', #41122, #94755 ) ;
#12901 = DIRECTION ( 'NONE',  ( 0.000000000000000000, -0.9999939076577903929, 0.003490651415223739937 ) ) ;
#12902 = VERTEX_POINT ( 'NONE', #101716 ) ;
#12903 = EDGE_LOOP ( 'NONE', ( #66424, #33366 ) ) ;
#12904 = DIRECTION ( 'NONE',  ( -4.274815082592931898E-19, -0.9999939076577903929, -0.003490651415223739937 ) ) ;
#12905 = CARTESIAN_POINT ( 'NONE',  ( 11.84999999999990372, 2.500000000000000000, 2.511473670974873507 ) ) ;
#12907 = EDGE_CURVE ( 'NONE', #37067, #11332, #75457, .T. ) ;
#12906 = PLANE ( 'NONE',  #87735 ) ;
#12908 = ORIENTED_EDGE ( 'NONE', *, *, #10704, .T. ) ;
#12909 = ORIENTED_EDGE ( 'NONE', *, *, #30355, .F. ) ;
#12910 = EDGE_CURVE ( 'NONE', #6482, #86589, #41437, .T. ) ;
#12911 = FACE_OUTER_BOUND ( 'NONE', #106112, .T. ) ;
#12912 = EDGE_CURVE ( 'NONE', #52516, #99205, #62265, .T. ) ;
#12913 = EDGE_CURVE ( 'NONE', #73015, #83312, #118675, .T. ) ;
#12915 = ORIENTED_EDGE ( 'NONE', *, *, #37051, .T. ) ;
#12914 = CIRCLE ( 'NONE', #115398, 0.1000000000000000472 ) ;
#12916 = DIRECTION ( 'NONE',  ( -0.000000000000000000, 1.000000000000000000, -0.000000000000000000 ) ) ;
#12917 = DIRECTION ( 'NONE',  ( -0.000000000000000000, -1.000000000000000000, -0.000000000000000000 ) ) ;
#12918 = CIRCLE ( 'NONE', #61056, 0.06509327318403745899 ) ;
#12919 = CARTESIAN_POINT ( 'NONE',  ( -1.850000000000033840, 2.500000000000000000, 6.148780366869520897 ) ) ;
#12920 = EDGE_LOOP ( 'NONE', ( #64529, #47148 ) ) ;
#12921 = FACE_OUTER_BOUND ( 'NONE', #770, .T. ) ;
#12923 = ADVANCED_FACE ( 'NONE', ( #85911 ), #43483, .T. ) ;
#12922 = CARTESIAN_POINT ( 'NONE',  ( 8.299999999999922551, 12.50000000000000000, -2.385244779468109755E-15 ) ) ;
#12924 = CARTESIAN_POINT ( 'NONE',  ( 3.149999999999946176, 12.50000000000000000, -6.083687093685488989 ) ) ;
#12925 = DIRECTION ( 'NONE',  ( -0.000000000000000000, 1.000000000000000000, -0.000000000000000000 ) ) ;
#12927 = CIRCLE ( 'NONE', #25442, 0.06509327318403745899 ) ;
#12926 = CARTESIAN_POINT ( 'NONE',  ( 186.5000000000000000, 0.000000000000000000, 7.700000000000000178 ) ) ;
#12928 = ORIENTED_EDGE ( 'NONE', *, *, #33874, .F. ) ;
#12929 = VECTOR ( 'NONE', #9411, 1000.000000000000000 ) ;
#12930 = ADVANCED_FACE ( 'NONE', ( #14594 ), #30973, .T. ) ;
#12931 = VECTOR ( 'NONE', #119865, 1000.000000000000000 ) ;
#12932 = LINE ( 'NONE', #26007, #78065 ) ;
#12933 = EDGE_CURVE ( 'NONE', #67119, #124524, #20493, .T. ) ;
#12934 = AXIS2_PLACEMENT_3D ( 'NONE', #32492, #46630, #33125 ) ;
#12935 = CARTESIAN_POINT ( 'NONE',  ( 48.83465639038744399, -3.619824997313607629, 4.313881469055892204 ) ) ;
#12936 = ORIENTED_EDGE ( 'NONE', *, *, #86951, .T. ) ;
#12937 = EDGE_LOOP ( 'NONE', ( #64563, #74537 ) ) ;
#12938 = CARTESIAN_POINT ( 'NONE',  ( 184.1927083336747160, 6.551208109652275624, -3.782341765624998686 ) ) ;
#12939 = DIRECTION ( 'NONE',  ( 0.000000000000000000, 0.000000000000000000, 1.000000000000000000 ) ) ;
#12940 = CARTESIAN_POINT ( 'NONE',  ( 8.349999999999919709, 2.500000000000000000, 6.495190528383297135 ) ) ;
#12941 = AXIS2_PLACEMENT_3D ( 'NONE', #33767, #14745, #46168 ) ;
#12942 = DIRECTION ( 'NONE',  ( -0.000000000000000000, -1.000000000000000000, -0.000000000000000000 ) ) ;
#12943 = DIRECTION ( 'NONE',  ( -0.000000000000000000, 1.000000000000000000, -0.000000000000000000 ) ) ;
#12944 = CIRCLE ( 'NONE', #25461, 0.06509327318403745899 ) ;
#12945 = DIRECTION ( 'NONE',  ( -0.000000000000000000, 1.000000000000000000, -0.000000000000000000 ) ) ;
#12946 = AXIS2_PLACEMENT_3D ( 'NONE', #61006, #19129, #119282 ) ;
#12947 = FACE_OUTER_BOUND ( 'NONE', #57257, .T. ) ;
#12948 = VECTOR ( 'NONE', #50605, 1000.000000000000000 ) ;
#12949 = LINE ( 'NONE', #112472, #58235 ) ;
#12950 = AXIS2_PLACEMENT_3D ( 'NONE', #106437, #118194, #128014 ) ;
#12951 = FACE_OUTER_BOUND ( 'NONE', #108264, .T. ) ;
#12952 = ORIENTED_EDGE ( 'NONE', *, *, #51164, .F. ) ;
#12953 = ORIENTED_EDGE ( 'NONE', *, *, #96376, .T. ) ;
#12954 = CONICAL_SURFACE ( 'NONE', #86107, 0.1000000000000002554, 0.003490658503988666988 ) ;
#12955 = ORIENTED_EDGE ( 'NONE', *, *, #51806, .T. ) ;
#12956 = ORIENTED_EDGE ( 'NONE', *, *, #83692, .F. ) ;
#12957 = CARTESIAN_POINT ( 'NONE',  ( 4.549999999999937650, 2.500000000000000000, 2.165063509461097713 ) ) ;
#12958 = FACE_OUTER_BOUND ( 'NONE', #29330, .T. ) ;
#12959 = VERTEX_POINT ( 'NONE', #85281 ) ;
#12960 = DIRECTION ( 'NONE',  ( 0.000000000000000000, -0.000000000000000000, 1.000000000000000000 ) ) ;
#12961 = FACE_OUTER_BOUND ( 'NONE', #119278, .T. ) ;
#12963 = VERTEX_POINT ( 'NONE', #65639 ) ;
#12962 = DIRECTION ( 'NONE',  ( -0.000000000000000000, 1.000000000000000000, -0.000000000000000000 ) ) ;
#12964 = CARTESIAN_POINT ( 'NONE',  ( -6.450000000000014388, 2.500000000000000000, 6.148780366869520897 ) ) ;
#12965 = DIRECTION ( 'NONE',  ( 0.000000000000000000, 0.000000000000000000, -1.000000000000000000 ) ) ;
#12966 = EDGE_LOOP ( 'NONE', ( #18068, #57686 ) ) ;
#12967 = EDGE_CURVE ( 'NONE', #112645, #70298, #25079, .T. ) ;
#12968 = EDGE_LOOP ( 'NONE', ( #71103, #30822, #115175, #19692 ) ) ;
#12969 = VERTEX_POINT ( 'NONE', #15890 ) ;
#12970 = VERTEX_POINT ( 'NONE', #45378 ) ;
#12971 = CARTESIAN_POINT ( 'NONE',  ( -5.600000000000023626, 2.500000000000000000, -4.083716857408426826 ) ) ;
#12972 = AXIS2_PLACEMENT_3D ( 'NONE', #68771, #79258, #60276 ) ;
#12973 = CONICAL_SURFACE ( 'NONE', #48506, 0.09999999999999982514, 0.003490658503988666988 ) ;
#12974 = DIRECTION ( 'NONE',  ( 0.000000000000000000, -0.9999939076577903929, 0.003490651415223739937 ) ) ;
#12975 = CARTESIAN_POINT ( 'NONE',  ( 142.3152275665817115, 2.500000000000000000, 4.152444035927816302 ) ) ;
#12976 = CARTESIAN_POINT ( 'NONE',  ( -10.40000000000000213, 12.50000000000000000, 3.637306695894644726 ) ) ;
#12978 = EDGE_LOOP ( 'NONE', ( #79196, #129369, #117893, #207 ) ) ;
#12977 = CIRCLE ( 'NONE', #44393, 0.09999999999999999167 ) ;
#12979 = AXIS2_PLACEMENT_3D ( 'NONE', #75917, #16960, #126317 ) ;
#12980 = VECTOR ( 'NONE', #19031, 1000.000000000000000 ) ;
#12981 = FACE_OUTER_BOUND ( 'NONE', #118782, .T. ) ;
#12983 = EDGE_LOOP ( 'NONE', ( #106410, #82037 ) ) ;
#12982 = AXIS2_PLACEMENT_3D ( 'NONE', #19172, #66991, #27093 ) ;
#12984 = DIRECTION ( 'NONE',  ( 0.000000000000000000, 0.000000000000000000, 1.000000000000000000 ) ) ;
#12985 = CARTESIAN_POINT ( 'NONE',  ( 4.912722231850287002, -2.499999999999493738, -9.942384338125227927 ) ) ;
#12986 = CONICAL_SURFACE ( 'NONE', #67350, 0.09999999999999982514, 0.003490658503988666988 ) ;
#12987 = DIRECTION ( 'NONE',  ( 0.000000000000000000, 0.000000000000000000, 1.000000000000000000 ) ) ;
#12988 = FACE_OUTER_BOUND ( 'NONE', #71014, .T. ) ;
#12989 = AXIS2_PLACEMENT_3D ( 'NONE', #3155, #51614, #122930 ) ;
#12990 = ORIENTED_EDGE ( 'NONE', *, *, #66351, .F. ) ;
#12991 = ORIENTED_EDGE ( 'NONE', *, *, #18769, .F. ) ;
#12992 = EDGE_LOOP ( 'NONE', ( #57182, #49158, #122128, #70930 ) ) ;
#12993 = DIRECTION ( 'NONE',  ( 0.000000000000000000, 1.000000000000000000, 0.000000000000000000 ) ) ;
#12994 = CARTESIAN_POINT ( 'NONE',  ( -10.85000000000000142, 2.500000000000000000, -5.802370205355746435 ) ) ;
#12995 = DIRECTION ( 'NONE',  ( 0.000000000000000000, -0.9999939076577903929, 0.003490651415223739937 ) ) ;
#12996 = FACE_BOUND ( 'NONE', #104435, .T. ) ;
#12997 = DIRECTION ( 'NONE',  ( 0.000000000000000000, 0.000000000000000000, -1.000000000000000000 ) ) ;
#12998 = FACE_OUTER_BOUND ( 'NONE', #12968, .T. ) ;
#12999 = DIRECTION ( 'NONE',  ( -4.274815082592931898E-19, -0.9999939076577903929, -0.003490651415223739937 ) ) ;
#13000 = CARTESIAN_POINT ( 'NONE',  ( 186.5468750003414300, -8.734944146203032389, -1.604583208406767949E-15 ) ) ;
#13001 = PLANE ( 'NONE',  #52942 ) ;
#13002 = DIRECTION ( 'NONE',  ( 0.000000000000000000, -0.9999939076577903929, 0.003490651415223739937 ) ) ;
#13003 = ORIENTED_EDGE ( 'NONE', *, *, #90188, .F. ) ;
#13004 = EDGE_CURVE ( 'NONE', #101973, #56674, #16522, .T. ) ;
#13005 = CARTESIAN_POINT ( 'NONE',  ( 4.999999999999969802, 12.50000000000000000, 4.330127018922196314 ) ) ;
#13006 = EDGE_LOOP ( 'NONE', ( #127270, #28784, #70697, #31091 ) ) ;
#13007 = ORIENTED_EDGE ( 'NONE', *, *, #19931, .F. ) ;
#13008 = DIRECTION ( 'NONE',  ( 0.000000000000000000, 0.000000000000000000, 1.000000000000000000 ) ) ;
#13009 = EDGE_CURVE ( 'NONE', #38596, #49056, #43451, .T. ) ;
#13010 = DIRECTION ( 'NONE',  ( 0.000000000000000000, -0.9999939076577903929, 0.003490651415223739937 ) ) ;
#13011 = FACE_BOUND ( 'NONE', #119466, .T. ) ;
#13012 = ADVANCED_FACE ( 'NONE', ( #64983 ), #60218, .T. ) ;
#13013 = CARTESIAN_POINT ( 'NONE',  ( -1.900000000000035438, 12.50000000000000000, 3.983716857408420076 ) ) ;
#13014 = AXIS2_PLACEMENT_3D ( 'NONE', #78157, #99083, #36306 ) ;
#13015 = AXIS2_PLACEMENT_3D ( 'NONE', #103631, #53247, #51961 ) ;
#13016 = EDGE_CURVE ( 'NONE', #34741, #58724, #120836, .T. ) ;
#13017 = EDGE_CURVE ( 'NONE', #117086, #65795, #85235, .T. ) ;
#13018 = EDGE_LOOP ( 'NONE', ( #3223, #23106 ) ) ;
#13019 = CARTESIAN_POINT ( 'NONE',  ( 65.34954526967068489, 3.515384427023733327, 5.621991122696823773 ) ) ;
#13020 = EDGE_CURVE ( 'NONE', #73744, #84243, #37221, .T. ) ;
#13021 = EDGE_CURVE ( 'NONE', #94856, #70361, #97833, .T. ) ;
#13022 = LINE ( 'NONE', #83092, #72847 ) ;
#13023 = EDGE_CURVE ( 'NONE', #87315, #78724, #36201, .T. ) ;
#13024 = ORIENTED_EDGE ( 'NONE', *, *, #35686, .T. ) ;
#13026 = FACE_OUTER_BOUND ( 'NONE', #129219, .T. ) ;
#13025 = VECTOR ( 'NONE', #44571, 1000.000000000000000 ) ;
#13027 = PLANE ( 'NONE',  #63786 ) ;
#13028 = AXIS2_PLACEMENT_3D ( 'NONE', #70823, #101582, #39466 ) ;
#13029 = CIRCLE ( 'NONE', #86194, 0.06509327318403745899 ) ;
#13030 = CIRCLE ( 'NONE', #86196, 0.1000000000000002554 ) ;
#13031 = ORIENTED_EDGE ( 'NONE', *, *, #77174, .F. ) ;
#13032 = DIRECTION ( 'NONE',  ( 0.000000000000000000, 0.000000000000000000, -1.000000000000000000 ) ) ;
#13034 = EDGE_CURVE ( 'NONE', #35370, #32515, #116029, .T. ) ;
#13033 = DIRECTION ( 'NONE',  ( -0.000000000000000000, 1.000000000000000000, -0.000000000000000000 ) ) ;
#13035 = CONICAL_SURFACE ( 'NONE', #77996, 0.09999999999999999167, 0.003490658503988666988 ) ;
#13036 = ORIENTED_EDGE ( 'NONE', *, *, #72533, .F. ) ;
#13037 = DIRECTION ( 'NONE',  ( 0.000000000000000000, 1.000000000000000000, 0.000000000000000000 ) ) ;
#13038 = CONICAL_SURFACE ( 'NONE', #117489, 0.1000000000000002554, 0.003490658503988666988 ) ;
#13039 = DIRECTION ( 'NONE',  ( -0.000000000000000000, 1.000000000000000000, -0.000000000000000000 ) ) ;
#13040 = DIRECTION ( 'NONE',  ( 0.000000000000000000, -0.9999939076577903929, 0.003490651415223739937 ) ) ;
#13041 = ORIENTED_EDGE ( 'NONE', *, *, #18761, .F. ) ;
#13042 = ORIENTED_EDGE ( 'NONE', *, *, #76448, .F. ) ;
#13043 = DIRECTION ( 'NONE',  ( 0.000000000000000000, 0.000000000000000000, -1.000000000000000000 ) ) ;
#13044 = EDGE_LOOP ( 'NONE', ( #46334, #7376 ) ) ;
#13045 = CARTESIAN_POINT ( 'NONE',  ( -8.950000000000008171, 2.500000000000000000, 1.918653347947321564 ) ) ;
#13046 = DIRECTION ( 'NONE',  ( 0.000000000000000000, -0.9999939076577903929, 0.003490651415223739937 ) ) ;
#13047 = VERTEX_POINT ( 'NONE', #106220 ) ;
#13048 = CARTESIAN_POINT ( 'NONE',  ( 195.5000000000000000, 0.000000000000000000, 0.000000000000000000 ) ) ;
#13049 = CARTESIAN_POINT ( 'NONE',  ( 11.84999999999990727, 2.500000000000000000, -2.411473670974877859 ) ) ;
#13050 = CARTESIAN_POINT ( 'NONE',  ( 12.29999999999990123, 12.50000000000000000, 0.3464101615137735735 ) ) ;
#13051 = CARTESIAN_POINT ( 'NONE',  ( -3.750000000000025757, 2.500000000000000000, -2.857883832488653741 ) ) ;
#13052 = CIRCLE ( 'NONE', #102959, 0.09999999999999982514 ) ;
#13053 = LINE ( 'NONE', #94864, #99690 ) ;
#13054 = ORIENTED_EDGE ( 'NONE', *, *, #106885, .T. ) ;
#13055 = ORIENTED_EDGE ( 'NONE', *, *, #22342, .F. ) ;
#13056 = DIRECTION ( 'NONE',  ( 0.000000000000000000, 0.000000000000000000, 1.000000000000000000 ) ) ;
#13057 = EDGE_LOOP ( 'NONE', ( #96920, #93253, #54424, #44278 ) ) ;
#13058 = CIRCLE ( 'NONE', #100896, 0.09999999999999999167 ) ;
#13059 = DIRECTION ( 'NONE',  ( 0.000000000000000000, -0.9999939076577903929, 0.003490651415223739937 ) ) ;
#13060 = CIRCLE ( 'NONE', #46522, 0.06509327318403745899 ) ;
#13062 = EDGE_CURVE ( 'NONE', #16232, #79210, #74866, .T. ) ;
#13061 = AXIS2_PLACEMENT_3D ( 'NONE', #87644, #10228, #7145 ) ;
#13064 = ORIENTED_EDGE ( 'NONE', *, *, #6304, .T. ) ;
#13063 = EDGE_LOOP ( 'NONE', ( #108632, #114549 ) ) ;
#13065 = VERTEX_POINT ( 'NONE', #4129 ) ;
#13066 = EDGE_CURVE ( 'NONE', #62016, #96759, #78994, .T. ) ;
#13067 = DIRECTION ( 'NONE',  ( -0.000000000000000000, 1.000000000000000000, -0.000000000000000000 ) ) ;
#13068 = EDGE_CURVE ( 'NONE', #42458, #118390, #49748, .T. ) ;
#13069 = DIRECTION ( 'NONE',  ( 0.000000000000000000, 1.000000000000000000, 0.000000000000000000 ) ) ;
#13070 = CONICAL_SURFACE ( 'NONE', #11021, 0.1000000000000002554, 0.003490658503988666988 ) ;
#13072 = FACE_OUTER_BOUND ( 'NONE', #50654, .T. ) ;
#13071 = CIRCLE ( 'NONE', #115473, 0.06509327318403745899 ) ;
#13073 = ADVANCED_FACE ( 'NONE', ( #56458 ), #7352, .T. ) ;
#13074 =( NAMED_UNIT ( * ) PLANE_ANGLE_UNIT ( ) SI_UNIT ( $, .RADIAN. ) );
#13075 = FACE_OUTER_BOUND ( 'NONE', #87613, .T. ) ;
#13076 = CARTESIAN_POINT ( 'NONE',  ( -5.600000000000020073, 2.500000000000000000, 4.576537180435972019 ) ) ;
#13077 = CARTESIAN_POINT ( 'NONE',  ( -0.6500000000000389910, 2.500000000000000000, -6.048780366869526581 ) ) ;
#13078 = VECTOR ( 'NONE', #70882, 1000.000000000000000 ) ;
#13079 = CARTESIAN_POINT ( 'NONE',  ( 3.349999999999945466, 12.50000000000000000, -2.165063509461101710 ) ) ;
#13080 = CARTESIAN_POINT ( 'NONE',  ( -8.350000000000012079, 2.500000000000000000, -1.472243186433550122 ) ) ;
#13081 = EDGE_CURVE ( 'NONE', #86648, #112541, #57109, .T. ) ;
#13082 = CARTESIAN_POINT ( 'NONE',  ( 7.899999999999924860, 2.500000000000000000, 4.922947341949748257 ) ) ;
#13083 = CIRCLE ( 'NONE', #119705, 0.1000000000000002554 ) ;
#13084 = EDGE_CURVE ( 'NONE', #39004, #121634, #26742, .T. ) ;
#13086 = VERTEX_POINT ( 'NONE', #128456 ) ;
#13085 = ADVANCED_FACE ( 'NONE', ( #97679 ), #87207, .T. ) ;
#13087 = EDGE_CURVE ( 'NONE', #67710, #60176, #106841, .T. ) ;
#13088 = CARTESIAN_POINT ( 'NONE',  ( -3.150000000000030553, 2.500000000000000000, 6.248780366869520542 ) ) ;
#13089 = ORIENTED_EDGE ( 'NONE', *, *, #87692, .T. ) ;
#13090 = EDGE_LOOP ( 'NONE', ( #110355, #46045, #48715, #127508 ) ) ;
#13091 = LINE ( 'NONE', #93606, #33651 ) ;
#13092 = CARTESIAN_POINT ( 'NONE',  ( -2.100000000000033396, 2.500000000000000000, -5.122947341949753763 ) ) ;
#13093 = DIRECTION ( 'NONE',  ( 0.000000000000000000, -0.000000000000000000, 1.000000000000000000 ) ) ;
#13094 = ADVANCED_FACE ( 'NONE', ( #76760 ), #10022, .T. ) ;
#13095 = CIRCLE ( 'NONE', #50774, 0.09999999999999982514 ) ;
#13096 = CARTESIAN_POINT ( 'NONE',  ( 12.89999999999989910, 12.50000000000000000, 0.6928203230275494784 ) ) ;
#13097 = DIRECTION ( 'NONE',  ( -0.000000000000000000, 1.000000000000000000, -0.000000000000000000 ) ) ;
#13098 = CARTESIAN_POINT ( 'NONE',  ( -5.400000000000019895, 2.500000000000000000, -2.276824562219559311E-15 ) ) ;
#13099 = FACE_OUTER_BOUND ( 'NONE', #44753, .T. ) ;
#13100 = EDGE_LOOP ( 'NONE', ( #68005, #22445 ) ) ;
#13101 = VECTOR ( 'NONE', #36196, 1000.000000000000000 ) ;
#13102 = AXIS2_PLACEMENT_3D ( 'NONE', #127352, #9504, #37681 ) ;
#13103 = ORIENTED_EDGE ( 'NONE', *, *, #4044, .F. ) ;
#13104 = AXIS2_PLACEMENT_3D ( 'NONE', #125723, #6576, #56988 ) ;
#13105 = EDGE_LOOP ( 'NONE', ( #77767, #26936, #92010, #66197 ) ) ;
#13106 = EDGE_LOOP ( 'NONE', ( #85851, #62775 ) ) ;
#13107 = EDGE_CURVE ( 'NONE', #22575, #84951, #8003, .T. ) ;
#13108 = EDGE_LOOP ( 'NONE', ( #117519, #9755 ) ) ;
#13109 = VECTOR ( 'NONE', #99491, 1000.000000000000000 ) ;
#13110 = CARTESIAN_POINT ( 'NONE',  ( 9.999999999999948486, 2.500000000000000000, -4.330127018922201643 ) ) ;
#13111 = FACE_OUTER_BOUND ( 'NONE', #106105, .T. ) ;
#13112 = MECHANICAL_DESIGN_GEOMETRIC_PRESENTATION_REPRESENTATION (  '', ( #48647 ), #601 ) ;
#13113 = CIRCLE ( 'NONE', #54987, 0.06509327318403745899 ) ;
#13114 = CARTESIAN_POINT ( 'NONE',  ( 6.249999999999932498, 12.50000000000000000, -5.802370205355749988 ) ) ;
#13115 = CONICAL_SURFACE ( 'NONE', #69564, 0.09999999999999999167, 0.003490658503988666988 ) ;
#13116 = DIRECTION ( 'NONE',  ( 0.000000000000000000, 0.000000000000000000, 1.000000000000000000 ) ) ;
#13117 = DIRECTION ( 'NONE',  ( 0.000000000000000000, 1.000000000000000000, 0.000000000000000000 ) ) ;
#13118 = ORIENTED_EDGE ( 'NONE', *, *, #102486, .T. ) ;
#13119 = CARTESIAN_POINT ( 'NONE',  ( 43.31340628060505793, -2.029328412884075838, 5.113049426574150402 ) ) ;
#13120 = DIRECTION ( 'NONE',  ( 0.000000000000000000, 0.000000000000000000, 1.000000000000000000 ) ) ;
#13121 = CARTESIAN_POINT ( 'NONE',  ( -3.300000000000027800, 12.50000000000000000, 0.06509327318403515528 ) ) ;
#13122 = AXIS2_PLACEMENT_3D ( 'NONE', #52958, #41856, #81752 ) ;
#13123 = AXIS2_PLACEMENT_3D ( 'NONE', #56329, #116546, #115226 ) ;
#13124 = DIRECTION ( 'NONE',  ( -0.000000000000000000, -1.000000000000000000, -0.000000000000000000 ) ) ;
#13125 = VERTEX_POINT ( 'NONE', #28302 ) ;
#13126 = EDGE_CURVE ( 'NONE', #20627, #69676, #22650, .T. ) ;
#13127 = CONICAL_SURFACE ( 'NONE', #98819, 0.1000000000000002554, 0.003490658503988666988 ) ;
#13128 = VECTOR ( 'NONE', #84395, 1000.000000000000000 ) ;
#13129 = ORIENTED_EDGE ( 'NONE', *, *, #113398, .F. ) ;
#13130 = EDGE_LOOP ( 'NONE', ( #25654, #99192, #122534, #87896 ) ) ;
#13131 = DIRECTION ( 'NONE',  ( 0.000000000000000000, -0.9999939076577903929, 0.003490651415223739937 ) ) ;
#13132 = CIRCLE ( 'NONE', #94716, 0.06509327318403745899 ) ;
#13133 = CARTESIAN_POINT ( 'NONE',  ( 4.999999999999936939, 2.500000000000000000, -0.7928203230275542301 ) ) ;
#13134 = LINE ( 'NONE', #14424, #10524 ) ;
#13135 = CIRCLE ( 'NONE', #29885, 0.1000000000000000472 ) ;
#13136 = VERTEX_POINT ( 'NONE', #9301 ) ;
#13137 = DIRECTION ( 'NONE',  ( 0.000000000000000000, 1.000000000000000000, 0.000000000000000000 ) ) ;
#13138 = CARTESIAN_POINT ( 'NONE',  ( -3.350000000000028955, 12.50000000000000000, 2.230156782645134950 ) ) ;
#13139 = ADVANCED_FACE ( 'NONE', ( #77401 ), #69495, .F. ) ;
#13140 = DIRECTION ( 'NONE',  ( 0.000000000000000000, -0.000000000000000000, 1.000000000000000000 ) ) ;
#13141 = PLANE ( 'NONE',  #66492 ) ;
#13142 = DIRECTION ( 'NONE',  ( -0.000000000000000000, -1.000000000000000000, -0.000000000000000000 ) ) ;
#13143 = VERTEX_POINT ( 'NONE', #27630 ) ;
#13144 = AXIS2_PLACEMENT_3D ( 'NONE', #24858, #23566, #64772 ) ;
#13145 = EDGE_LOOP ( 'NONE', ( #88927, #44891 ) ) ;
#13146 = CIRCLE ( 'NONE', #73801, 0.1000000000000002554 ) ;
#13147 = CARTESIAN_POINT ( 'NONE',  ( -1.900000000000035438, 2.500000000000000000, 4.083716857408420609 ) ) ;
#13148 = DIRECTION ( 'NONE',  ( -0.000000000000000000, 1.000000000000000000, -0.000000000000000000 ) ) ;
#13149 = DIRECTION ( 'NONE',  ( -0.000000000000000000, -1.000000000000000000, -0.000000000000000000 ) ) ;
#13150 = DIRECTION ( 'NONE',  ( -0.000000000000000000, 1.000000000000000000, -0.000000000000000000 ) ) ;
#13151 = EDGE_LOOP ( 'NONE', ( #95718, #99214, #121649, #32479 ) ) ;
#13152 = AXIS2_PLACEMENT_3D ( 'NONE', #90754, #32511, #119560 ) ;
#13153 = CIRCLE ( 'NONE', #29912, 0.1000000000000002554 ) ;
#13154 = CIRCLE ( 'NONE', #42446, 0.1000000000000000472 ) ;
#13155 = ORIENTED_EDGE ( 'NONE', *, *, #78972, .T. ) ;
#13156 = PLANE ( 'NONE',  #125371 ) ;
#13157 = DIRECTION ( 'NONE',  ( 0.000000000000000000, -0.9999939076577903929, 0.003490651415223739937 ) ) ;
#13158 = PLANE ( 'NONE',  #82083 ) ;
#13159 = CARTESIAN_POINT ( 'NONE',  ( -6.450000000000019718, 2.500000000000000000, -6.148780366869526226 ) ) ;
#13160 = CARTESIAN_POINT ( 'NONE',  ( 4.999999999999973355, 2.500000000000000000, -4.230127018922201998 ) ) ;
#13161 = VERTEX_POINT ( 'NONE', #86565 ) ;
#13163 = DIRECTION ( 'NONE',  ( -0.000000000000000000, 1.000000000000000000, -0.000000000000000000 ) ) ;
#13162 = CIRCLE ( 'NONE', #59173, 0.06509327318403745899 ) ;
#13164 = ADVANCED_FACE ( 'NONE', ( #8633 ), #60311, .T. ) ;
#13165 = CARTESIAN_POINT ( 'NONE',  ( -10.40000000000000213, 2.500000000000000000, 0.6928203230275494784 ) ) ;
#13166 = AXIS2_PLACEMENT_3D ( 'NONE', #120310, #110481, #20819 ) ;
#13167 = EDGE_LOOP ( 'NONE', ( #102118, #26859, #85353, #100914 ) ) ;
#13168 = DIRECTION ( 'NONE',  ( 0.000000000000000000, 0.000000000000000000, -1.000000000000000000 ) ) ;
#13169 = ORIENTED_EDGE ( 'NONE', *, *, #38468, .T. ) ;
#13170 = VECTOR ( 'NONE', #78008, 1000.000000000000000 ) ;
#13171 = CARTESIAN_POINT ( 'NONE',  ( -1.700000000000034817, 12.50000000000000000, -4.330127018922201643 ) ) ;
#13172 = VERTEX_POINT ( 'NONE', #78705 ) ;
#13173 = DIRECTION ( 'NONE',  ( 0.000000000000000000, 1.000000000000000000, 0.000000000000000000 ) ) ;
#13174 = CARTESIAN_POINT ( 'NONE',  ( 6.649999999999928413, 2.500000000000000000, 1.572243186433545548 ) ) ;
#13175 = ADVANCED_FACE ( 'NONE', ( #127784 ), #119248, .T. ) ;
#13176 = EDGE_LOOP ( 'NONE', ( #79654, #67909, #16343, #73857 ) ) ;
#13177 = ADVANCED_FACE ( 'NONE', ( #38792 ), #39389, .T. ) ;
#13178 = VERTEX_POINT ( 'NONE', #19092 ) ;
#13179 = EDGE_CURVE ( 'NONE', #49764, #179, #59054, .T. ) ;
#13180 = EDGE_CURVE ( 'NONE', #49224, #43749, #129107, .T. ) ;
#13181 = CARTESIAN_POINT ( 'NONE',  ( 185.4635416670080872, -4.367472073101519747, 7.564683531249999149 ) ) ;
#13182 = DIRECTION ( 'NONE',  ( 0.000000000000000000, 0.000000000000000000, 1.000000000000000000 ) ) ;
#13183 = AXIS2_PLACEMENT_3D ( 'NONE', #56467, #77412, #67571 ) ;
#13184 = DIRECTION ( 'NONE',  ( 0.000000000000000000, 0.000000000000000000, -1.000000000000000000 ) ) ;
#13185 = CARTESIAN_POINT ( 'NONE',  ( 5.399999999999936406, 12.50000000000000000, -5.022947341949754119 ) ) ;
#13186 = DIRECTION ( 'NONE',  ( 0.000000000000000000, -0.000000000000000000, 1.000000000000000000 ) ) ;
#13187 = DIRECTION ( 'NONE',  ( 0.000000000000000000, 1.000000000000000000, 0.000000000000000000 ) ) ;
#13188 = CARTESIAN_POINT ( 'NONE',  ( -5.600000000000020073, 12.50000000000000000, -0.3464101615137782364 ) ) ;
#13189 = CARTESIAN_POINT ( 'NONE',  ( 9.199999999999915801, 12.50000000000000000, -4.395220292106239768 ) ) ;
#13190 = CARTESIAN_POINT ( 'NONE',  ( -5.400000000000020783, 12.50000000000000000, 4.957854068765711553 ) ) ;
#13191 = EDGE_CURVE ( 'NONE', #3245, #40491, #110451, .T. ) ;
#13192 = VECTOR ( 'NONE', #90918, 1000.000000000000000 ) ;
#13194 = EDGE_CURVE ( 'NONE', #104331, #121408, #45632, .T. ) ;
#13193 = AXIS2_PLACEMENT_3D ( 'NONE', #106256, #116069, #33654 ) ;
#13195 = CIRCLE ( 'NONE', #92638, 0.1000000000000002554 ) ;
#13196 = ADVANCED_FACE ( 'NONE', ( #30256 ), #49839, .T. ) ;
#13197 = VERTEX_POINT ( 'NONE', #79970 ) ;
#13198 = VERTEX_POINT ( 'NONE', #120545 ) ;
#13199 = DIRECTION ( 'NONE',  ( 0.000000000000000000, 1.000000000000000000, 0.000000000000000000 ) ) ;
#13200 = EDGE_LOOP ( 'NONE', ( #14637, #98227, #73551, #51717 ) ) ;
#13201 = LINE ( 'NONE', #102871, #28693 ) ;
#13202 = CARTESIAN_POINT ( 'NONE',  ( -1.650000000000034328, 12.50000000000000000, -7.188010851410854052 ) ) ;
#13203 = DIRECTION ( 'NONE',  ( 0.000000000000000000, 0.000000000000000000, 1.000000000000000000 ) ) ;
#13205 = ORIENTED_EDGE ( 'NONE', *, *, #108921, .F. ) ;
#13204 = ORIENTED_EDGE ( 'NONE', *, *, #97767, .T. ) ;
#13206 = FACE_BOUND ( 'NONE', #116516, .T. ) ;
#13207 = EDGE_LOOP ( 'NONE', ( #11206, #61153 ) ) ;
#13208 = CIRCLE ( 'NONE', #90581, 0.1000000000000002554 ) ;
#13209 = CARTESIAN_POINT ( 'NONE',  ( -0.4500000000000402012, 12.50000000000000000, 2.165063509461097713 ) ) ;
#13210 = CARTESIAN_POINT ( 'NONE',  ( -1.900000000000034994, 2.500000000000000000, -4.576537180435978236 ) ) ;
#13211 = AXIS2_PLACEMENT_3D ( 'NONE', #127425, #128739, #77028 ) ;
#13212 = FACE_OUTER_BOUND ( 'NONE', #69238, .T. ) ;
#13213 = PLANE ( 'NONE',  #7512 ) ;
#13214 = AXIS2_PLACEMENT_3D ( 'NONE', #104734, #109082, #115186 ) ;
#13215 = DIRECTION ( 'NONE',  ( 0.000000000000000000, 0.000000000000000000, 1.000000000000000000 ) ) ;
#13216 = FACE_OUTER_BOUND ( 'NONE', #36004, .T. ) ;
#13217 = DIRECTION ( 'NONE',  ( 0.000000000000000000, 0.000000000000000000, 1.000000000000000000 ) ) ;
#13218 = DIRECTION ( 'NONE',  ( -4.274815082592931898E-19, -0.9999939076577903929, -0.003490651415223739937 ) ) ;
#13219 = DIRECTION ( 'NONE',  ( 0.000000000000000000, -0.9999939076577903929, 0.003490651415223739937 ) ) ;
#13220 = DIRECTION ( 'NONE',  ( 0.000000000000000000, 0.000000000000000000, 1.000000000000000000 ) ) ;
#13221 = DIRECTION ( 'NONE',  ( -0.000000000000000000, -1.000000000000000000, -0.000000000000000000 ) ) ;
#13222 = ORIENTED_EDGE ( 'NONE', *, *, #121521, .F. ) ;
#13223 = ORIENTED_EDGE ( 'NONE', *, *, #30499, .T. ) ;
#13224 = ORIENTED_EDGE ( 'NONE', *, *, #21382, .T. ) ;
#13225 = CARTESIAN_POINT ( 'NONE',  ( 10.39999999999990976, 2.500000000000000000, 4.430127018922196847 ) ) ;
#13226 = ORIENTED_EDGE ( 'NONE', *, *, #28444, .F. ) ;
#13227 = DIRECTION ( 'NONE',  ( 0.000000000000000000, 0.000000000000000000, 1.000000000000000000 ) ) ;
#13229 = EDGE_LOOP ( 'NONE', ( #28765, #7941 ) ) ;
#13228 = ORIENTED_EDGE ( 'NONE', *, *, #86637, .F. ) ;
#13230 = EDGE_LOOP ( 'NONE', ( #58246, #90153, #56548, #127801 ) ) ;
#13231 = CIRCLE ( 'NONE', #119855, 0.06509327318403745899 ) ;
#13232 = LINE ( 'NONE', #23725, #48039 ) ;
#13233 = DIRECTION ( 'NONE',  ( -4.274815082592931898E-19, -0.9999939076577903929, -0.003490651415223739937 ) ) ;
#13234 = FACE_OUTER_BOUND ( 'NONE', #76372, .T. ) ;
#13235 = CARTESIAN_POINT ( 'NONE',  ( 185.4895833340161175, -4.445597072760163471, -7.699999999999919353 ) ) ;
#13236 = CARTESIAN_POINT ( 'NONE',  ( -9.400000000000007461, 2.500000000000000000, 0.4464101615137735513 ) ) ;
#13237 = ORIENTED_EDGE ( 'NONE', *, *, #46171, .F. ) ;
#13238 = EDGE_CURVE ( 'NONE', #10798, #123447, #58247, .T. ) ;
#13239 = DIRECTION ( 'NONE',  ( 0.000000000000000000, 0.000000000000000000, 1.000000000000000000 ) ) ;
#13240 = ORIENTED_EDGE ( 'NONE', *, *, #94451, .T. ) ;
#13241 = ADVANCED_FACE ( 'NONE', ( #99624 ), #122988, .T. ) ;
#13242 = ORIENTED_EDGE ( 'NONE', *, *, #82237, .F. ) ;
#13243 = ORIENTED_EDGE ( 'NONE', *, *, #108724, .T. ) ;
#13244 = ADVANCED_FACE ( 'NONE', ( #112 ), #20417, .T. ) ;
#13245 = FACE_OUTER_BOUND ( 'NONE', #17994, .T. ) ;
#13246 = CIRCLE ( 'NONE', #80161, 0.09999999999999982514 ) ;
#13247 = AXIS2_PLACEMENT_3D ( 'NONE', #118205, #88747, #67139 ) ;
#13248 = VERTEX_POINT ( 'NONE', #22362 ) ;
#13249 = ORIENTED_EDGE ( 'NONE', *, *, #43912, .F. ) ;
#13250 = ORIENTED_EDGE ( 'NONE', *, *, #82726, .T. ) ;
#13251 = PLANE ( 'NONE',  #86273 ) ;
#13252 = ADVANCED_FACE ( 'NONE', ( #41362 ), #81223, .T. ) ;
#13254 = DIRECTION ( 'NONE',  ( 0.000000000000000000, 0.000000000000000000, 1.000000000000000000 ) ) ;
#13253 = CIRCLE ( 'NONE', #86414, 0.06509327318403741736 ) ;
#13255 = AXIS2_PLACEMENT_3D ( 'NONE', #721, #58380, #77999 ) ;
#13256 = FACE_OUTER_BOUND ( 'NONE', #54597, .T. ) ;
#13258 = LINE ( 'NONE', #74780, #96505 ) ;
#13257 = CONICAL_SURFACE ( 'NONE', #71867, 0.1000000000000000056, 0.003490658503988666988 ) ;
#13259 = DIRECTION ( 'NONE',  ( 1.000000000000000000, 0.000000000000000000, 0.000000000000000000 ) ) ;
#13260 = AXIS2_PLACEMENT_3D ( 'NONE', #102581, #71856, #12898 ) ;
#13261 = CIRCLE ( 'NONE', #50944, 0.09999999999999982514 ) ;
#13262 = DIRECTION ( 'NONE',  ( -4.274815082592931898E-19, -0.9999939076577903929, -0.003490651415223739937 ) ) ;
#13263 = FACE_OUTER_BOUND ( 'NONE', #104039, .T. ) ;
#13264 = AXIS2_PLACEMENT_3D ( 'NONE', #30083, #107976, #88983 ) ;
#13266 = ORIENTED_EDGE ( 'NONE', *, *, #55211, .T. ) ;
#13265 = AXIS2_PLACEMENT_3D ( 'NONE', #41448, #82653, #81366 ) ;
#13267 = CARTESIAN_POINT ( 'NONE',  ( -10.00000000000000711, 12.50000000000000000, -3.637306695894645614 ) ) ;
#13268 = CIRCLE ( 'NONE', #103162, 0.09999999999999999167 ) ;
#13269 = ORIENTED_EDGE ( 'NONE', *, *, #66892, .F. ) ;
#13270 = CARTESIAN_POINT ( 'NONE',  ( 184.9166666666666856, 6.668395609140176816, 3.850000000000000977 ) ) ;
#13271 = VECTOR ( 'NONE', #14828, 1000.000000000000000 ) ;
#13272 = ORIENTED_EDGE ( 'NONE', *, *, #6706, .T. ) ;
#13273 = VECTOR ( 'NONE', #26969, 1000.000000000000000 ) ;
#13274 = VERTEX_POINT ( 'NONE', #50505 ) ;
#13275 = CARTESIAN_POINT ( 'NONE',  ( -11.84999999999999787, 12.50000000000000000, -6.148780366869522673 ) ) ;
#13276 = CARTESIAN_POINT ( 'NONE',  ( 184.4010416670080872, -4.367472073101519747, 7.564683531249999149 ) ) ;
#13277 = CARTESIAN_POINT ( 'NONE',  ( 5.599999999999933031, 2.500000000000000000, -0.4464101615137783252 ) ) ;
#13278 = ORIENTED_EDGE ( 'NONE', *, *, #65843, .F. ) ;
#13279 = ORIENTED_EDGE ( 'NONE', *, *, #53103, .T. ) ;
#13280 = FACE_OUTER_BOUND ( 'NONE', #88634, .T. ) ;
#13281 = DIRECTION ( 'NONE',  ( -0.000000000000000000, -1.000000000000000000, -0.000000000000000000 ) ) ;
#13282 = CARTESIAN_POINT ( 'NONE',  ( -8.950000000000009948, 2.500000000000000000, -1.818653347947326138 ) ) ;
#13283 = DIRECTION ( 'NONE',  ( 0.000000000000000000, 0.000000000000000000, -1.000000000000000000 ) ) ;
#13284 = AXIS2_PLACEMENT_3D ( 'NONE', #109448, #110093, #89804 ) ;
#13285 = DIRECTION ( 'NONE',  ( 0.000000000000000000, 0.000000000000000000, 1.000000000000000000 ) ) ;
#13286 = EDGE_LOOP ( 'NONE', ( #5465, #122974 ) ) ;
#13287 = EDGE_CURVE ( 'NONE', #39657, #82277, #24786, .T. ) ;
#13288 = DIRECTION ( 'NONE',  ( 0.000000000000000000, 0.000000000000000000, -1.000000000000000000 ) ) ;
#13289 = CIRCLE ( 'NONE', #4971, 0.1000000000000002554 ) ;
#13290 = VERTEX_POINT ( 'NONE', #32825 ) ;
#13291 = CIRCLE ( 'NONE', #34258, 0.06509327318403745899 ) ;
#13292 = PLANE ( 'NONE',  #59119 ) ;
#13293 = DIRECTION ( 'NONE',  ( 0.000000000000000000, 0.000000000000000000, 1.000000000000000000 ) ) ;
#13294 = AXIS2_PLACEMENT_3D ( 'NONE', #116839, #37664, #46840 ) ;
#13295 = EDGE_CURVE ( 'NONE', #33480, #43682, #62282, .T. ) ;
#13296 = CARTESIAN_POINT ( 'NONE',  ( 187.2500000000000000, 9.429780353434619030E-16, -7.700000000000000178 ) ) ;
#13297 = CARTESIAN_POINT ( 'NONE',  ( 6.249999999999965361, 12.50000000000000000, 2.230156782645134950 ) ) ;
#13298 = CARTESIAN_POINT ( 'NONE',  ( 0.3999999999999568345, 2.500000000000000000, -3.637306695894650055 ) ) ;
#13299 = ADVANCED_FACE ( 'NONE', ( #70797 ), #129268, .T. ) ;
#13300 = DIRECTION ( 'NONE',  ( -4.274815082592931898E-19, -0.9999939076577903929, -0.003490651415223739937 ) ) ;
#13301 = CIRCLE ( 'NONE', #109458, 0.1000000000000002554 ) ;
#13303 = AXIS2_PLACEMENT_3D ( 'NONE', #60631, #23250, #110977 ) ;
#13302 = CARTESIAN_POINT ( 'NONE',  ( 6.249999999999930722, 2.500000000000000000, -1.372243186433550033 ) ) ;
#13304 = ORIENTED_EDGE ( 'NONE', *, *, #128052, .F. ) ;
#13305 = AXIS2_PLACEMENT_3D ( 'NONE', #81513, #121419, #1009 ) ;
#13306 = CONICAL_SURFACE ( 'NONE', #67690, 0.09999999999999982514, 0.003490658503988666988 ) ;
#13307 = DIRECTION ( 'NONE',  ( -0.000000000000000000, -1.000000000000000000, -0.000000000000000000 ) ) ;
#13308 = DIRECTION ( 'NONE',  ( 0.000000000000000000, 0.000000000000000000, 1.000000000000000000 ) ) ;
#13309 = CARTESIAN_POINT ( 'NONE',  ( 3.299999999999942979, 12.50000000000000000, 4.330127018922196314 ) ) ;
#13310 = VERTEX_POINT ( 'NONE', #82568 ) ;
#13311 = ADVANCED_FACE ( 'NONE', ( #81270 ), #120919, .T. ) ;
#13312 = AXIS2_PLACEMENT_3D ( 'NONE', #99858, #67802, #99212 ) ;
#13313 = CARTESIAN_POINT ( 'NONE',  ( -6.850000000000013856, 12.50000000000000000, 1.883746621131358934 ) ) ;
#13314 = ORIENTED_EDGE ( 'NONE', *, *, #123574, .T. ) ;
#13315 = AXIS2_PLACEMENT_3D ( 'NONE', #83380, #123294, #80806 ) ;
#13317 = VERTEX_POINT ( 'NONE', #122486 ) ;
#13316 = AXIS2_PLACEMENT_3D ( 'NONE', #38006, #38678, #19661 ) ;
#13318 = CIRCLE ( 'NONE', #55108, 0.1000000000000002554 ) ;
#13319 = PLANE ( 'NONE',  #94836 ) ;
#13320 = ORIENTED_EDGE ( 'NONE', *, *, #3449, .T. ) ;
#13321 = CARTESIAN_POINT ( 'NONE',  ( 17.33812564108167109, -2.538896947916728042, -5.379288978446362890 ) ) ;
#13322 = DIRECTION ( 'NONE',  ( -0.000000000000000000, 1.000000000000000000, -0.000000000000000000 ) ) ;
#13323 = CARTESIAN_POINT ( 'NONE',  ( 2.099999999999949463, 2.500000000000000000, -3.637306695894650055 ) ) ;
#13324 = CIRCLE ( 'NONE', #103230, 0.06509327318403745899 ) ;
#13325 = ORIENTED_EDGE ( 'NONE', *, *, #60721, .T. ) ;
#13326 = FACE_OUTER_BOUND ( 'NONE', #14209, .T. ) ;
#13327 = EDGE_CURVE ( 'NONE', #99644, #83794, #9946, .T. ) ;
#13328 = CARTESIAN_POINT ( 'NONE',  ( 9.399999999999915090, 2.500000000000000000, -4.676537180435977881 ) ) ;
#13329 = EDGE_LOOP ( 'NONE', ( #51943, #22724, #7559, #798 ) ) ;
#13330 = EDGE_CURVE ( 'NONE', #95574, #120916, #37315, .T. ) ;
#13331 = EDGE_LOOP ( 'NONE', ( #35059, #83982, #36088, #48029 ) ) ;
#13332 = EDGE_LOOP ( 'NONE', ( #98087, #4659 ) ) ;
#13333 = DIRECTION ( 'NONE',  ( -0.000000000000000000, -1.000000000000000000, -0.000000000000000000 ) ) ;
#13334 = DIRECTION ( 'NONE',  ( 0.000000000000000000, 1.000000000000000000, 0.000000000000000000 ) ) ;
#13336 = CARTESIAN_POINT ( 'NONE',  ( -5.800000000000018474, 12.50000000000000000, -2.276824562219559311E-15 ) ) ;
#13335 = AXIS2_PLACEMENT_3D ( 'NONE', #114364, #86171, #97312 ) ;
#13337 = EDGE_CURVE ( 'NONE', #124980, #75076, #93740, .T. ) ;
#13338 = AXIS2_PLACEMENT_3D ( 'NONE', #55569, #113850, #83739 ) ;
#13339 = ADVANCED_FACE ( 'NONE', ( #761 ), #106254, .T. ) ;
#13340 = ORIENTED_EDGE ( 'NONE', *, *, #112615, .T. ) ;
#13341 = EDGE_CURVE ( 'NONE', #55354, #18200, #66534, .T. ) ;
#13342 = EDGE_CURVE ( 'NONE', #46558, #36089, #43930, .T. ) ;
#13343 = DIRECTION ( 'NONE',  ( 0.000000000000000000, 0.000000000000000000, -1.000000000000000000 ) ) ;
#13344 = DIRECTION ( 'NONE',  ( 0.000000000000000000, 0.000000000000000000, 1.000000000000000000 ) ) ;
#13345 = ORIENTED_EDGE ( 'NONE', *, *, #31233, .F. ) ;
#13346 = DIRECTION ( 'NONE',  ( 0.000000000000000000, -0.9999939076577903929, 0.003490651415223739937 ) ) ;
#13347 = DIRECTION ( 'NONE',  ( 0.000000000000000000, 0.000000000000000000, 1.000000000000000000 ) ) ;
#13348 = CIRCLE ( 'NONE', #117903, 0.1000000000000000472 ) ;
#13349 = AXIS2_PLACEMENT_3D ( 'NONE', #97185, #7504, #47446 ) ;
#13350 = VECTOR ( 'NONE', #89402, 1000.000000000000000 ) ;
#13351 = EDGE_CURVE ( 'NONE', #17483, #90021, #94961, .T. ) ;
#13352 = FACE_OUTER_BOUND ( 'NONE', #71155, .T. ) ;
#13353 = CARTESIAN_POINT ( 'NONE',  ( 2.500000000000002220, -0.5000000000000004441, 10.00000000000000178 ) ) ;
#13354 = CARTESIAN_POINT ( 'NONE',  ( -15.59999999999998010, 12.50000000000000000, -0.3464101615137759604 ) ) ;
#13355 = ADVANCED_FACE ( 'NONE', ( #94291 ), #28905, .T. ) ;
#13356 = CARTESIAN_POINT ( 'NONE',  ( 7.099999999999926814, 12.50000000000000000, 0.06509327318403515528 ) ) ;
#13357 = CARTESIAN_POINT ( 'NONE',  ( -5.400000000000019895, 12.50000000000000000, 4.330127018922196314 ) ) ;
#13358 = AXIS2_PLACEMENT_3D ( 'NONE', #14273, #83676, #113124 ) ;
#13359 = EDGE_CURVE ( 'NONE', #79439, #109003, #83283, .T. ) ;
#13360 = CIRCLE ( 'NONE', #113732, 0.06509327318403745899 ) ;
#13361 = CIRCLE ( 'NONE', #78230, 0.09999999999999982514 ) ;
#13362 = EDGE_CURVE ( 'NONE', #92091, #112676, #108397, .T. ) ;
#13363 = EDGE_LOOP ( 'NONE', ( #85085, #88230, #96699, #60951 ) ) ;
#13364 = ORIENTED_EDGE ( 'NONE', *, *, #21014, .T. ) ;
#13365 = ORIENTED_EDGE ( 'NONE', *, *, #41805, .F. ) ;
#13366 = VERTEX_POINT ( 'NONE', #73367 ) ;
#13367 = DIRECTION ( 'NONE',  ( 0.000000000000000000, -0.000000000000000000, 1.000000000000000000 ) ) ;
#13368 = CARTESIAN_POINT ( 'NONE',  ( -9.400000000000009237, 2.500000000000000000, -3.883716857408422207 ) ) ;
#13369 = DIRECTION ( 'NONE',  ( -0.000000000000000000, -1.000000000000000000, -0.000000000000000000 ) ) ;
#13370 = EDGE_LOOP ( 'NONE', ( #20518, #3828 ) ) ;
#13371 = EDGE_CURVE ( 'NONE', #5489, #27768, #26838, .T. ) ;
#13372 = FACE_BOUND ( 'NONE', #62739, .T. ) ;
#13373 = EDGE_CURVE ( 'NONE', #21305, #12208, #100002, .T. ) ;
#13374 = DIRECTION ( 'NONE',  ( 0.000000000000000000, -0.000000000000000000, 1.000000000000000000 ) ) ;
#13375 = FACE_OUTER_BOUND ( 'NONE', #59574, .T. ) ;
#13376 = DIRECTION ( 'NONE',  ( 0.000000000000000000, 0.000000000000000000, -1.000000000000000000 ) ) ;
#13377 = DIRECTION ( 'NONE',  ( 0.000000000000000000, 0.000000000000000000, 1.000000000000000000 ) ) ;
#13378 = CARTESIAN_POINT ( 'NONE',  ( -3.350000000000029399, 2.500000000000000000, 6.595190528383296780 ) ) ;
#13379 = DIRECTION ( 'NONE',  ( -0.000000000000000000, -1.000000000000000000, -0.000000000000000000 ) ) ;
#13380 = DIRECTION ( 'NONE',  ( 0.000000000000000000, 0.000000000000000000, -1.000000000000000000 ) ) ;
#13381 = CARTESIAN_POINT ( 'NONE',  ( 5.449999999999936229, 2.500000000000000000, 6.595190528383296780 ) ) ;
#13382 = CARTESIAN_POINT ( 'NONE',  ( 13.54999999999990123, 12.50000000000000000, 1.818653347947321475 ) ) ;
#13383 = VECTOR ( 'NONE', #6976, 1000.000000000000000 ) ;
#13384 = ORIENTED_EDGE ( 'NONE', *, *, #22244, .F. ) ;
#13385 = VERTEX_POINT ( 'NONE', #24925 ) ;
#13386 = ORIENTED_EDGE ( 'NONE', *, *, #79697, .T. ) ;
#13387 = ORIENTED_EDGE ( 'NONE', *, *, #26530, .T. ) ;
#13388 = EDGE_LOOP ( 'NONE', ( #114877, #39822 ) ) ;
#13389 = ORIENTED_EDGE ( 'NONE', *, *, #66031, .F. ) ;
#13390 = DIRECTION ( 'NONE',  ( 0.000000000000000000, -0.000000000000000000, 1.000000000000000000 ) ) ;
#13391 = ORIENTED_EDGE ( 'NONE', *, *, #6410, .F. ) ;
#13392 = EDGE_LOOP ( 'NONE', ( #91136, #86358, #66497, #36149 ) ) ;
#13393 = AXIS2_PLACEMENT_3D ( 'NONE', #116556, #119617, #89521 ) ;
#13394 = CARTESIAN_POINT ( 'NONE',  ( 13.12246079397647236, -2.500000000000000444, 7.156134182876034977 ) ) ;
#13395 = DIRECTION ( 'NONE',  ( -0.000000000000000000, 1.000000000000000000, -0.000000000000000000 ) ) ;
#13396 = DIRECTION ( 'NONE',  ( 0.000000000000000000, -0.000000000000000000, 1.000000000000000000 ) ) ;
#13397 = CONICAL_SURFACE ( 'NONE', #590, 0.1000000000000002554, 0.003490658503988666988 ) ;
#13398 = ORIENTED_EDGE ( 'NONE', *, *, #31029, .T. ) ;
#13399 = DIRECTION ( 'NONE',  ( 0.000000000000000000, 0.000000000000000000, -1.000000000000000000 ) ) ;
#13400 = VERTEX_POINT ( 'NONE', #62912 ) ;
#13401 = CONICAL_SURFACE ( 'NONE', #86563, 0.1000000000000002554, 0.003490658503988666988 ) ;
#13402 = ADVANCED_FACE ( 'NONE', ( #53734 ), #93663, .T. ) ;
#13403 = EDGE_LOOP ( 'NONE', ( #90667, #38687, #114327, #22421 ) ) ;
#13404 = DIRECTION ( 'NONE',  ( -0.000000000000000000, 1.000000000000000000, -0.000000000000000000 ) ) ;
#13405 = EDGE_CURVE ( 'NONE', #4060, #114757, #43585, .T. ) ;
#13406 = DIRECTION ( 'NONE',  ( 0.000000000000000000, 1.000000000000000000, 0.000000000000000000 ) ) ;
#13407 = EDGE_LOOP ( 'NONE', ( #3466, #8451 ) ) ;
#13408 = ORIENTED_EDGE ( 'NONE', *, *, #83127, .T. ) ;
#13409 = LINE ( 'NONE', #115459, #35934 ) ;
#13411 = CONICAL_SURFACE ( 'NONE', #15553, 0.09999999999999982514, 0.003490658503988666988 ) ;
#13410 = DIRECTION ( 'NONE',  ( 0.000000000000000000, 0.000000000000000000, 1.000000000000000000 ) ) ;
#13413 = AXIS2_PLACEMENT_3D ( 'NONE', #31421, #102088, #52988 ) ;
#13412 = CARTESIAN_POINT ( 'NONE',  ( 3.349999999999943689, 2.500000000000000000, 1.472243186433545459 ) ) ;
#13414 = AXIS2_PLACEMENT_3D ( 'NONE', #99877, #20026, #111620 ) ;
#13415 = DIRECTION ( 'NONE',  ( 0.000000000000000000, 0.000000000000000000, 1.000000000000000000 ) ) ;
#13416 = CARTESIAN_POINT ( 'NONE',  ( -6.249999999999984901, 2.500000000000000000, -2.065063509461102065 ) ) ;
#13417 = AXIS2_PLACEMENT_3D ( 'NONE', #85962, #15932, #55870 ) ;
#13418 = EDGE_LOOP ( 'NONE', ( #123746, #35138, #13748, #124316 ) ) ;
#13419 = CIRCLE ( 'NONE', #2974, 0.09999999999999999167 ) ;
#13420 = DIRECTION ( 'NONE',  ( -0.000000000000000000, 1.000000000000000000, -0.000000000000000000 ) ) ;
#13421 = ORIENTED_EDGE ( 'NONE', *, *, #62308, .F. ) ;
#13422 = DIRECTION ( 'NONE',  ( 0.000000000000000000, -0.000000000000000000, 1.000000000000000000 ) ) ;
#13423 = ORIENTED_EDGE ( 'NONE', *, *, #70420, .F. ) ;
#13424 = CARTESIAN_POINT ( 'NONE',  ( 15.59999999999988951, 2.500000000000000000, 0.2464101615137735679 ) ) ;
#13425 = CARTESIAN_POINT ( 'NONE',  ( -6.050000000000020250, 12.50000000000000000, -2.511473670974877948 ) ) ;
#13426 = DIRECTION ( 'NONE',  ( -0.000000000000000000, 1.000000000000000000, -0.000000000000000000 ) ) ;
#13427 = FACE_OUTER_BOUND ( 'NONE', #16601, .T. ) ;
#13428 = VERTEX_POINT ( 'NONE', #114575 ) ;
#13429 = FACE_OUTER_BOUND ( 'NONE', #31524, .T. ) ;
#13430 = CIRCLE ( 'NONE', #30190, 0.06509327318403745899 ) ;
#13432 = DIRECTION ( 'NONE',  ( -0.000000000000000000, 1.000000000000000000, -0.000000000000000000 ) ) ;
#13431 = VECTOR ( 'NONE', #66560, 1000.000000000000000 ) ;
#13433 = ORIENTED_EDGE ( 'NONE', *, *, #111619, .T. ) ;
#13434 = ORIENTED_EDGE ( 'NONE', *, *, #39714, .F. ) ;
#13435 = CIRCLE ( 'NONE', #99136, 0.09999999999999982514 ) ;
#13436 = CIRCLE ( 'NONE', #109603, 0.06509327318403745899 ) ;
#13437 = EDGE_LOOP ( 'NONE', ( #74422, #23551 ) ) ;
#13438 = LINE ( 'NONE', #43578, #58330 ) ;
#13439 = DIRECTION ( 'NONE',  ( -4.274815082592931898E-19, -0.9999939076577903929, -0.003490651415223739937 ) ) ;
#13440 = CARTESIAN_POINT ( 'NONE',  ( 186.6093750003414016, 9.264065473108010111E-16, -7.564683531250000925 ) ) ;
#13441 = DIRECTION ( 'NONE',  ( 0.000000000000000000, 1.000000000000000000, 0.000000000000000000 ) ) ;
#13442 = DIRECTION ( 'NONE',  ( -0.000000000000000000, 1.000000000000000000, -0.000000000000000000 ) ) ;
#13443 = EDGE_CURVE ( 'NONE', #38221, #108534, #72900, .T. ) ;
#13444 = AXIS2_PLACEMENT_3D ( 'NONE', #92881, #112516, #22217 ) ;
#13445 = DIRECTION ( 'NONE',  ( 0.000000000000000000, 0.000000000000000000, 1.000000000000000000 ) ) ;
#13446 = AXIS2_PLACEMENT_3D ( 'NONE', #55177, #95104, #83973 ) ;
#13447 = DIRECTION ( 'NONE',  ( 0.000000000000000000, 0.000000000000000000, 1.000000000000000000 ) ) ;
#13448 = VERTEX_POINT ( 'NONE', #74023 ) ;
#13449 = AXIS2_PLACEMENT_3D ( 'NONE', #73211, #43769, #116339 ) ;
#13450 = AXIS2_PLACEMENT_3D ( 'NONE', #9740, #117735, #79142 ) ;
#13451 = CARTESIAN_POINT ( 'NONE',  ( -12.49999999999999289, 2.500000000000000000, -5.022947341949751454 ) ) ;
#13452 = VECTOR ( 'NONE', #88367, 1000.000000000000000 ) ;
#13453 = EDGE_LOOP ( 'NONE', ( #48996, #39643 ) ) ;
#13454 = DIRECTION ( 'NONE',  ( 0.000000000000000000, 1.000000000000000000, 0.000000000000000000 ) ) ;
#13455 = CIRCLE ( 'NONE', #59467, 0.1000000000000002554 ) ;
#13456 = ADVANCED_FACE ( 'NONE', ( #24272 ), #16434, .T. ) ;
#13458 = EDGE_CURVE ( 'NONE', #127834, #27192, #35345, .T. ) ;
#13457 = CARTESIAN_POINT ( 'NONE',  ( -5.800000000000018474, 12.50000000000000000, -2.276824562219559311E-15 ) ) ;
#13459 = FACE_OUTER_BOUND ( 'NONE', #81914, .T. ) ;
#13460 = DIRECTION ( 'NONE',  ( 0.000000000000000000, 1.000000000000000000, 0.000000000000000000 ) ) ;
#13461 = ORIENTED_EDGE ( 'NONE', *, *, #112359, .T. ) ;
#13462 = CARTESIAN_POINT ( 'NONE',  ( -11.05000000000000071, 2.500000000000000000, -2.611473670974873595 ) ) ;
#13464 = ORIENTED_EDGE ( 'NONE', *, *, #110622, .F. ) ;
#13463 = DIRECTION ( 'NONE',  ( 0.000000000000000000, 0.000000000000000000, -1.000000000000000000 ) ) ;
#13465 = EDGE_CURVE ( 'NONE', #85004, #82670, #33207, .T. ) ;
#13466 = CIRCLE ( 'NONE', #124298, 0.06509327318403745899 ) ;
#13467 = ORIENTED_EDGE ( 'NONE', *, *, #91212, .F. ) ;
#13468 = FACE_OUTER_BOUND ( 'NONE', #88251, .T. ) ;
#13469 = ORIENTED_EDGE ( 'NONE', *, *, #23025, .T. ) ;
#13470 = ORIENTED_EDGE ( 'NONE', *, *, #32295, .F. ) ;
#13471 = CARTESIAN_POINT ( 'NONE',  ( 0.1999999999999567124, 2.500000000000000000, -3.983716857408426293 ) ) ;
#13472 = ORIENTED_EDGE ( 'NONE', *, *, #24198, .F. ) ;
#13473 = CARTESIAN_POINT ( 'NONE',  ( -6.900000000000019007, 12.50000000000000000, -4.611443907251940644 ) ) ;
#13474 = CARTESIAN_POINT ( 'NONE',  ( -8.950000000000011724, 12.50000000000000000, -6.083687093685483660 ) ) ;
#13475 = AXIS2_PLACEMENT_3D ( 'NONE', #71825, #23340, #63283 ) ;
#13476 = DIRECTION ( 'NONE',  ( -0.000000000000000000, 1.000000000000000000, -0.000000000000000000 ) ) ;
#13477 = VECTOR ( 'NONE', #24146, 1000.000000000000000 ) ;
#13478 = ORIENTED_EDGE ( 'NONE', *, *, #30809, .F. ) ;
#13479 = FACE_OUTER_BOUND ( 'NONE', #81303, .T. ) ;
#13480 = VERTEX_POINT ( 'NONE', #93024 ) ;
#13481 = DIRECTION ( 'NONE',  ( -0.000000000000000000, 1.000000000000000000, -0.000000000000000000 ) ) ;
#13482 = LINE ( 'NONE', #101237, #6925 ) ;
#13483 = ORIENTED_EDGE ( 'NONE', *, *, #9053, .F. ) ;
#13484 = CONICAL_SURFACE ( 'NONE', #55278, 0.1000000000000002554, 0.003490658503988666988 ) ;
#13485 = EDGE_CURVE ( 'NONE', #33342, #41996, #5265, .T. ) ;
#13486 = ORIENTED_EDGE ( 'NONE', *, *, #60242, .T. ) ;
#13488 = EDGE_LOOP ( 'NONE', ( #86289, #118077, #98582, #30780 ) ) ;
#13487 = CIRCLE ( 'NONE', #63694, 0.1000000000000002554 ) ;
#13489 = EDGE_LOOP ( 'NONE', ( #58015, #18694 ) ) ;
#13490 = DIRECTION ( 'NONE',  ( 0.000000000000000000, 0.000000000000000000, 1.000000000000000000 ) ) ;
#13491 = CARTESIAN_POINT ( 'NONE',  ( 5.399999999999932854, 2.500000000000000000, 3.637306695894644726 ) ) ;
#13492 = CARTESIAN_POINT ( 'NONE',  ( 2.299999999999946976, 2.500000000000000000, 4.676537180435972552 ) ) ;
#13493 = EDGE_CURVE ( 'NONE', #15344, #91497, #66626, .T. ) ;
#13494 = FACE_BOUND ( 'NONE', #15515, .T. ) ;
#13495 = ORIENTED_EDGE ( 'NONE', *, *, #59152, .T. ) ;
#13496 = CARTESIAN_POINT ( 'NONE',  ( 184.8229166673494603, -4.445597072760122614, 7.699999999999998401 ) ) ;
#13497 = EDGE_CURVE ( 'NONE', #55738, #101182, #121014, .T. ) ;
#13498 = DIRECTION ( 'NONE',  ( 0.000000000000000000, 1.000000000000000000, 0.000000000000000000 ) ) ;
#13499 = LINE ( 'NONE', #24630, #12531 ) ;
#13500 = AXIS2_PLACEMENT_3D ( 'NONE', #74390, #4329, #44277 ) ;
#13501 = ADVANCED_FACE ( 'NONE', ( #45856 ), #106347, .T. ) ;
#13502 = CARTESIAN_POINT ( 'NONE',  ( 145.7653593504141725, 0.5000000000000000000, -3.576063159858998475 ) ) ;
#13503 = EDGE_CURVE ( 'NONE', #64922, #17072, #114742, .T. ) ;
#13504 = CARTESIAN_POINT ( 'NONE',  ( 12.49999999999990585, 2.500000000000000000, -5.022947341949754119 ) ) ;
#13505 = VECTOR ( 'NONE', #86458, 1000.000000000000000 ) ;
#13506 = EDGE_CURVE ( 'NONE', #20279, #9507, #22744, .T. ) ;
#13507 = CARTESIAN_POINT ( 'NONE',  ( 129.5000000000000000, 1.500000000000000000, 2.598076211353316900 ) ) ;
#13508 = CONICAL_SURFACE ( 'NONE', #34468, 0.1000000000000000472, 0.003490658503988666988 ) ;
#13509 = CARTESIAN_POINT ( 'NONE',  ( -3.750000000000027534, 2.500000000000000000, -1.472243186433550122 ) ) ;
#13510 = EDGE_CURVE ( 'NONE', #113395, #5884, #68778, .T. ) ;
#13511 = EDGE_LOOP ( 'NONE', ( #89884, #75266 ) ) ;
#13512 = EDGE_LOOP ( 'NONE', ( #70620, #69584, #105066, #11918 ) ) ;
#13513 = ORIENTED_EDGE ( 'NONE', *, *, #122854, .T. ) ;
#13514 = VERTEX_POINT ( 'NONE', #106058 ) ;
#13515 = ORIENTED_EDGE ( 'NONE', *, *, #105325, .T. ) ;
#13516 = PLANE ( 'NONE',  #10439 ) ;
#13517 = DIRECTION ( 'NONE',  ( -0.000000000000000000, -1.000000000000000000, -0.000000000000000000 ) ) ;
#13518 = EDGE_LOOP ( 'NONE', ( #95037, #80468, #118525, #112893 ) ) ;
#13519 = FACE_BOUND ( 'NONE', #63268, .T. ) ;
#13520 = EDGE_CURVE ( 'NONE', #40491, #3245, #26929, .T. ) ;
#13521 = CARTESIAN_POINT ( 'NONE',  ( -6.450000000000019718, 2.500000000000000000, -6.048780366869526581 ) ) ;
#13522 = CONICAL_SURFACE ( 'NONE', #80448, 0.1000000000000002554, 0.003490658503988666988 ) ;
#13523 = VECTOR ( 'NONE', #93954, 1000.000000000000000 ) ;
#13525 = VERTEX_POINT ( 'NONE', #68060 ) ;
#13524 = VECTOR ( 'NONE', #46120, 1000.000000000000000 ) ;
#13526 = AXIS2_PLACEMENT_3D ( 'NONE', #95343, #23356, #33834 ) ;
#13527 = DIRECTION ( 'NONE',  ( 0.000000000000000000, -0.9999939076577903929, 0.003490651415223739937 ) ) ;
#13528 = DIRECTION ( 'NONE',  ( 1.000000000000000000, 0.000000000000000000, 0.000000000000000000 ) ) ;
#13529 = DIRECTION ( 'NONE',  ( 1.000000000000000000, -0.000000000000000000, -0.000000000000000000 ) ) ;
#13530 = ORIENTED_EDGE ( 'NONE', *, *, #73504, .F. ) ;
#13531 = DIRECTION ( 'NONE',  ( 0.000000000000000000, 0.000000000000000000, -1.000000000000000000 ) ) ;
#13532 = CONICAL_SURFACE ( 'NONE', #82604, 0.1000000000000000056, 0.003490658503988666988 ) ;
#13533 = VERTEX_POINT ( 'NONE', #126992 ) ;
#13534 = AXIS2_PLACEMENT_3D ( 'NONE', #91847, #51928, #2814 ) ;
#13535 = ORIENTED_EDGE ( 'NONE', *, *, #65057, .F. ) ;
#13536 = ORIENTED_EDGE ( 'NONE', *, *, #47499, .T. ) ;
#13537 = DIRECTION ( 'NONE',  ( 0.000000000000000000, 1.000000000000000000, 0.000000000000000000 ) ) ;
#13538 = VECTOR ( 'NONE', #122948, 1000.000000000000000 ) ;
#13539 = DIRECTION ( 'NONE',  ( -0.000000000000000000, 1.000000000000000000, -0.000000000000000000 ) ) ;
#13540 = DIRECTION ( 'NONE',  ( 0.000000000000000000, -0.000000000000000000, 1.000000000000000000 ) ) ;
#13541 = ORIENTED_EDGE ( 'NONE', *, *, #49552, .F. ) ;
#13542 = DIRECTION ( 'NONE',  ( 0.000000000000000000, 0.000000000000000000, 1.000000000000000000 ) ) ;
#13543 = CIRCLE ( 'NONE', #44959, 0.1000000000000002554 ) ;
#13544 = CIRCLE ( 'NONE', #30212, 0.06509327318403743123 ) ;
#13545 = DIRECTION ( 'NONE',  ( 0.000000000000000000, -0.000000000000000000, 1.000000000000000000 ) ) ;
#13546 = CARTESIAN_POINT ( 'NONE',  ( -3.749999999999991118, 2.500000000000000000, 2.165063509461097713 ) ) ;
#13547 = CARTESIAN_POINT ( 'NONE',  ( 186.3645833340161175, -6.668395609140180369, 3.849999999999994760 ) ) ;
#13548 = ORIENTED_EDGE ( 'NONE', *, *, #110064, .T. ) ;
#13549 = DIRECTION ( 'NONE',  ( 0.000000000000000000, 0.000000000000000000, 1.000000000000000000 ) ) ;
#13550 = EDGE_LOOP ( 'NONE', ( #120272, #103018, #85423, #115243 ) ) ;
#13551 = DIRECTION ( 'NONE',  ( 0.000000000000000000, 1.224646799147353454E-16, 1.000000000000000000 ) ) ;
#13552 = ORIENTED_EDGE ( 'NONE', *, *, #122864, .F. ) ;
#13553 = EDGE_CURVE ( 'NONE', #119152, #86156, #16986, .T. ) ;
#13554 = ORIENTED_EDGE ( 'NONE', *, *, #105431, .F. ) ;
#13555 = LINE ( 'NONE', #24044, #70155 ) ;
#13556 = CARTESIAN_POINT ( 'NONE',  ( 10.84999999999990905, 2.500000000000000000, -5.902370205355750521 ) ) ;
#13557 = PLANE ( 'NONE',  #50904 ) ;
#13558 = DIRECTION ( 'NONE',  ( 0.000000000000000000, 0.000000000000000000, 1.000000000000000000 ) ) ;
#13559 = LINE ( 'NONE', #53509, #43447 ) ;
#13560 = AXIS2_PLACEMENT_3D ( 'NONE', #118011, #28360, #95800 ) ;
#13561 = ORIENTED_EDGE ( 'NONE', *, *, #66420, .F. ) ;
#13562 = VERTEX_POINT ( 'NONE', #18311 ) ;
#13563 = EDGE_CURVE ( 'NONE', #33691, #120278, #49935, .T. ) ;
#13564 = CARTESIAN_POINT ( 'NONE',  ( 0.3999999999999559464, 12.50000000000000000, -4.330127018922201643 ) ) ;
#13565 = DIRECTION ( 'NONE',  ( 0.000000000000000000, 1.000000000000000000, 0.000000000000000000 ) ) ;
#13566 = CARTESIAN_POINT ( 'NONE',  ( -0.6000000000000388356, 2.500000000000000000, 3.983716857408420964 ) ) ;
#13567 = EDGE_LOOP ( 'NONE', ( #121236, #27837 ) ) ;
#13568 = VERTEX_POINT ( 'NONE', #57611 ) ;
#13569 = DIRECTION ( 'NONE',  ( 0.000000000000000000, 0.000000000000000000, 1.000000000000000000 ) ) ;
#13570 = CIRCLE ( 'NONE', #26199, 0.06509327318403745899 ) ;
#13571 = EDGE_LOOP ( 'NONE', ( #65108, #43647 ) ) ;
#13573 = CIRCLE ( 'NONE', #105534, 0.09999999999999982514 ) ;
#13572 = CARTESIAN_POINT ( 'NONE',  ( 2.899999999999944844, 12.50000000000000000, 3.637306695894644726 ) ) ;
#13574 = CARTESIAN_POINT ( 'NONE',  ( 4.599999999999938360, 2.500000000000000000, -0.5928203230275541635 ) ) ;
#13575 = EDGE_LOOP ( 'NONE', ( #5209, #109289 ) ) ;
#13576 = CARTESIAN_POINT ( 'NONE',  ( -5.400000000000023448, 12.50000000000000000, -5.022947341949754119 ) ) ;
#13577 = DIRECTION ( 'NONE',  ( -0.000000000000000000, 1.000000000000000000, -0.000000000000000000 ) ) ;
#13578 = DIRECTION ( 'NONE',  ( 0.000000000000000000, 0.000000000000000000, 1.000000000000000000 ) ) ;
#13579 = LINE ( 'NONE', #3139, #84464 ) ;
#13580 = CARTESIAN_POINT ( 'NONE',  ( -7.900000000000014566, 2.500000000000000000, -4.430127018922202176 ) ) ;
#13581 = ORIENTED_EDGE ( 'NONE', *, *, #33478, .T. ) ;
#13582 = CIRCLE ( 'NONE', #88809, 0.1000000000000002554 ) ;
#13583 = DIRECTION ( 'NONE',  ( -0.000000000000000000, 1.000000000000000000, -0.000000000000000000 ) ) ;
#13585 = AXIS2_PLACEMENT_3D ( 'NONE', #6416, #14321, #66649 ) ;
#13584 = CARTESIAN_POINT ( 'NONE',  ( -9.350000000000004974, 2.500000000000000000, 6.148780366869520897 ) ) ;
#13586 = ORIENTED_EDGE ( 'NONE', *, *, #30883, .T. ) ;
#13587 = ORIENTED_EDGE ( 'NONE', *, *, #127280, .F. ) ;
#13588 = CARTESIAN_POINT ( 'NONE',  ( 184.7760416670080588, 6.551208109652274736, 3.782341765625001351 ) ) ;
#13589 = CARTESIAN_POINT ( 'NONE',  ( -7.950000000000009059, 2.500000000000000000, 6.495190528383297135 ) ) ;
#13590 = CARTESIAN_POINT ( 'NONE',  ( -10.85000000000000142, 12.50000000000000000, -5.802370205355746435 ) ) ;
#13591 = FACE_OUTER_BOUND ( 'NONE', #3589, .T. ) ;
#13592 = CARTESIAN_POINT ( 'NONE',  ( -4.600000000000024514, 12.50000000000000000, 0.6928203230275494784 ) ) ;
#13593 = ADVANCED_FACE ( 'NONE', ( #16360 ), #129362, .T. ) ;
#13594 = CIRCLE ( 'NONE', #36617, 0.06509327318403745899 ) ;
#13595 = CARTESIAN_POINT ( 'NONE',  ( -1.850000000000033840, 12.50000000000000000, 6.213873640053559022 ) ) ;
#13596 = AXIS2_PLACEMENT_3D ( 'NONE', #52660, #53324, #41583 ) ;
#13597 = CARTESIAN_POINT ( 'NONE',  ( 1.699999999999950218, 2.500000000000000000, 4.330127018922196314 ) ) ;
#13598 = DIRECTION ( 'NONE',  ( -0.000000000000000000, 1.000000000000000000, -0.000000000000000000 ) ) ;
#13599 = DIRECTION ( 'NONE',  ( 0.000000000000000000, 0.000000000000000000, 1.000000000000000000 ) ) ;
#13600 = CARTESIAN_POINT ( 'NONE',  ( 186.5000000000000000, 0.000000000000000000, 7.700000000000000178 ) ) ;
#13601 = PLANE ( 'NONE',  #20802 ) ;
#13602 = EDGE_CURVE ( 'NONE', #98295, #41903, #56159, .T. ) ;
#13603 = ORIENTED_EDGE ( 'NONE', *, *, #67377, .F. ) ;
#13604 = ORIENTED_EDGE ( 'NONE', *, *, #100409, .T. ) ;
#13605 = EDGE_LOOP ( 'NONE', ( #43808, #122746, #113392, #75983 ) ) ;
#13606 = ADVANCED_FACE ( 'NONE', ( #97518 ), #28147, .T. ) ;
#13607 = ORIENTED_EDGE ( 'NONE', *, *, #87358, .F. ) ;
#13608 = EDGE_CURVE ( 'NONE', #71950, #12555, #54115, .T. ) ;
#13609 = CONICAL_SURFACE ( 'NONE', #51305, 0.1000000000000000472, 0.003490658503988666988 ) ;
#13610 = CARTESIAN_POINT ( 'NONE',  ( 11.89999999999990798, 2.500000000000000000, -4.083716857408426826 ) ) ;
#13611 = DIRECTION ( 'NONE',  ( 0.000000000000000000, 0.000000000000000000, 1.000000000000000000 ) ) ;
#13612 = VERTEX_POINT ( 'NONE', #116512 ) ;
#13613 = CARTESIAN_POINT ( 'NONE',  ( 3.099999999999944134, 2.500000000000000000, 4.676537180435972552 ) ) ;
#13614 = CIRCLE ( 'NONE', #86776, 0.1000000000000000472 ) ;
#13615 = EDGE_CURVE ( 'NONE', #31532, #42779, #127289, .T. ) ;
#13616 = VECTOR ( 'NONE', #35050, 1000.000000000000000 ) ;
#13617 = DIRECTION ( 'NONE',  ( 0.000000000000000000, -0.000000000000000000, 1.000000000000000000 ) ) ;
#13619 = ORIENTED_EDGE ( 'NONE', *, *, #36993, .F. ) ;
#13618 = CARTESIAN_POINT ( 'NONE',  ( 5.449999999999934452, 12.50000000000000000, 2.165063509461097713 ) ) ;
#13620 = CIRCLE ( 'NONE', #101467, 0.1000000000000002554 ) ;
#13621 = EDGE_CURVE ( 'NONE', #73563, #74488, #39475, .T. ) ;
#13622 = LINE ( 'NONE', #64663, #18189 ) ;
#13623 = DIRECTION ( 'NONE',  ( 0.000000000000000000, 0.000000000000000000, 1.000000000000000000 ) ) ;
#13624 = VERTEX_POINT ( 'NONE', #68705 ) ;
#13625 = VECTOR ( 'NONE', #76065, 1000.000000000000000 ) ;
#13626 = CONICAL_SURFACE ( 'NONE', #30389, 0.1000000000000002554, 0.003490658503988666988 ) ;
#13627 = ORIENTED_EDGE ( 'NONE', *, *, #123403, .T. ) ;
#13628 = ORIENTED_EDGE ( 'NONE', *, *, #127435, .F. ) ;
#13629 = EDGE_LOOP ( 'NONE', ( #115845, #34183, #91288, #118627 ) ) ;
#13630 = DIRECTION ( 'NONE',  ( 0.000000000000000000, -0.9999939076577903929, 0.003490651415223739937 ) ) ;
#13631 = DIRECTION ( 'NONE',  ( 0.000000000000000000, 1.000000000000000000, 0.000000000000000000 ) ) ;
#13632 = CARTESIAN_POINT ( 'NONE',  ( 1.649999999999951061, 12.50000000000000000, -6.430097255199264339 ) ) ;
#13633 = VECTOR ( 'NONE', #13439, 1000.000000000000000 ) ;
#13634 = DIRECTION ( 'NONE',  ( 0.000000000000000000, 1.000000000000000000, 0.000000000000000000 ) ) ;
#13635 = CIRCLE ( 'NONE', #80477, 0.1000000000000002554 ) ;
#13636 = ORIENTED_EDGE ( 'NONE', *, *, #19931, .T. ) ;
#13638 = AXIS2_PLACEMENT_3D ( 'NONE', #118571, #66893, #79324 ) ;
#13637 = FACE_OUTER_BOUND ( 'NONE', #84356, .T. ) ;
#13639 = VERTEX_POINT ( 'NONE', #46481 ) ;
#13640 = CARTESIAN_POINT ( 'NONE',  ( -9.999999999999971578, 2.500000000000000000, -4.330127018922197202 ) ) ;
#13641 = DIRECTION ( 'NONE',  ( -0.000000000000000000, 1.000000000000000000, -0.000000000000000000 ) ) ;
#13642 = CARTESIAN_POINT ( 'NONE',  ( 12.49999999999990408, 12.50000000000000000, -3.637306695894650055 ) ) ;
#13643 = CARTESIAN_POINT ( 'NONE',  ( 4.149999999999936406, 2.500000000000000000, 6.495190528383297135 ) ) ;
#13644 = ORIENTED_EDGE ( 'NONE', *, *, #119407, .T. ) ;
#13645 = ORIENTED_EDGE ( 'NONE', *, *, #2111, .F. ) ;
#13646 = ORIENTED_EDGE ( 'NONE', *, *, #65383, .F. ) ;
#13647 = DIRECTION ( 'NONE',  ( -0.000000000000000000, 1.000000000000000000, -0.000000000000000000 ) ) ;
#13648 = DIRECTION ( 'NONE',  ( 0.000000000000000000, 1.000000000000000000, 0.000000000000000000 ) ) ;
#13649 = DIRECTION ( 'NONE',  ( 0.000000000000000000, 0.000000000000000000, -1.000000000000000000 ) ) ;
#13650 = FACE_BOUND ( 'NONE', #91976, .T. ) ;
#13651 = CARTESIAN_POINT ( 'NONE',  ( -8.150000000000014566, 12.50000000000000000, -6.841600689897073373 ) ) ;
#13652 = CIRCLE ( 'NONE', #97289, 0.06509327318403745899 ) ;
#13653 = DIRECTION ( 'NONE',  ( 0.000000000000000000, 0.000000000000000000, -1.000000000000000000 ) ) ;
#13654 = ADVANCED_FACE ( 'NONE', ( #106690 ), #115874, .T. ) ;
#13655 = CARTESIAN_POINT ( 'NONE',  ( 8.549999999999918998, 12.50000000000000000, 6.841600689897072485 ) ) ;
#13656 = EDGE_CURVE ( 'NONE', #21944, #98236, #123078, .T. ) ;
#13657 = CARTESIAN_POINT ( 'NONE',  ( -2.500000000000032419, 2.500000000000000000, -3.537306695894649966 ) ) ;
#13658 = AXIS2_PLACEMENT_3D ( 'NONE', #93091, #94352, #4662 ) ;
#13659 = DIRECTION ( 'NONE',  ( 0.4999999999999992228, 0.000000000000000000, -0.8660254037844391517 ) ) ;
#13660 = ADVANCED_FACE ( 'NONE', ( #78553 ), #8483, .T. ) ;
#13661 = CARTESIAN_POINT ( 'NONE',  ( 3.099999999999945022, 2.500000000000000000, -4.676537180435978769 ) ) ;
#13662 = VERTEX_POINT ( 'NONE', #58900 ) ;
#13663 = CIRCLE ( 'NONE', #118317, 0.1000000000000002554 ) ;
#13664 = EDGE_CURVE ( 'NONE', #85870, #74320, #98805, .T. ) ;
#13665 = AXIS2_PLACEMENT_3D ( 'NONE', #95945, #6253, #46197 ) ;
#13666 = PLANE ( 'NONE',  #1488 ) ;
#13667 = EDGE_CURVE ( 'NONE', #102762, #120000, #116799, .T. ) ;
#13668 = EDGE_LOOP ( 'NONE', ( #6709, #88019, #87302, #120981 ) ) ;
#13669 = EDGE_LOOP ( 'NONE', ( #99546, #128770 ) ) ;
#13670 = ORIENTED_EDGE ( 'NONE', *, *, #9910, .F. ) ;
#13671 = CARTESIAN_POINT ( 'NONE',  ( -12.69999999999999396, 2.500000000000000000, 0.3464101615137776813 ) ) ;
#13672 = FACE_BOUND ( 'NONE', #55416, .T. ) ;
#13673 = FACE_OUTER_BOUND ( 'NONE', #84866, .T. ) ;
#13674 = EDGE_CURVE ( 'NONE', #121706, #78315, #100094, .T. ) ;
#13675 = CONICAL_SURFACE ( 'NONE', #49219, 0.1000000000000000472, 0.003490658503988666988 ) ;
#13676 = EDGE_CURVE ( 'NONE', #114100, #52047, #62447, .T. ) ;
#13677 = CIRCLE ( 'NONE', #65913, 0.09999999999999982514 ) ;
#13678 = ORIENTED_EDGE ( 'NONE', *, *, #20758, .T. ) ;
#13679 = DIRECTION ( 'NONE',  ( 0.000000000000000000, 0.000000000000000000, 1.000000000000000000 ) ) ;
#13680 = DIRECTION ( 'NONE',  ( 0.000000000000000000, 0.000000000000000000, 1.000000000000000000 ) ) ;
#13681 = ORIENTED_EDGE ( 'NONE', *, *, #25639, .T. ) ;
#13682 = DIRECTION ( 'NONE',  ( 0.000000000000000000, -0.9999939076577903929, 0.003490651415223739937 ) ) ;
#13683 = DIRECTION ( 'NONE',  ( -0.000000000000000000, -1.000000000000000000, -0.000000000000000000 ) ) ;
#13684 = AXIS2_PLACEMENT_3D ( 'NONE', #8667, #49934, #120584 ) ;
#13685 = AXIS2_PLACEMENT_3D ( 'NONE', #79407, #7413, #87900 ) ;
#13686 = B_SPLINE_CURVE_WITH_KNOTS ( 'NONE', 3,
 ( #84688, #44123, #95799, #5467, #93233, #95161, #6116, #15930, #103699, #116082 ),
 .UNSPECIFIED., .F., .F.,
 ( 4, 2, 2, 2, 4 ),
 ( 0.003751885956794874175, 0.02035553200375761485, 0.03695917805072035378, 0.05356282409768309272, 0.07016647014464583165 ),
 .UNSPECIFIED. ) ;
#13687 = EDGE_LOOP ( 'NONE', ( #61164, #7318 ) ) ;
#13688 = DIRECTION ( 'NONE',  ( 0.000000000000000000, 0.000000000000000000, 1.000000000000000000 ) ) ;
#13689 = CARTESIAN_POINT ( 'NONE',  ( -11.64999999999999680, 12.50000000000000000, 2.099970236277060032 ) ) ;
#13690 = EDGE_CURVE ( 'NONE', #27968, #75118, #104460, .T. ) ;
#13691 = ORIENTED_EDGE ( 'NONE', *, *, #19671, .F. ) ;
#13692 = CARTESIAN_POINT ( 'NONE',  ( -14.14999999999998792, 2.500000000000000000, -1.472243186433547901 ) ) ;
#13693 = DIRECTION ( 'NONE',  ( -4.274815082592931898E-19, -0.9999939076577903929, -0.003490651415223739937 ) ) ;
#13694 = CONICAL_SURFACE ( 'NONE', #26239, 0.1000000000000002554, 0.003490658503988666988 ) ;
#13695 = DIRECTION ( 'NONE',  ( 0.000000000000000000, 1.000000000000000000, 0.000000000000000000 ) ) ;
#13696 = ORIENTED_EDGE ( 'NONE', *, *, #117371, .T. ) ;
#13697 = ORIENTED_EDGE ( 'NONE', *, *, #92558, .F. ) ;
#13698 = EDGE_CURVE ( 'NONE', #127947, #102323, #64571, .T. ) ;
#13699 = CARTESIAN_POINT ( 'NONE',  ( 4.799999999999937650, 2.500000000000000000, -0.4464101615137782142 ) ) ;
#13700 = AXIS2_PLACEMENT_3D ( 'NONE', #50957, #62066, #80413 ) ;
#13701 = ORIENTED_EDGE ( 'NONE', *, *, #109733, .T. ) ;
#13702 = CARTESIAN_POINT ( 'NONE',  ( 0.6499999999999561684, 12.50000000000000000, -1.818653347947325916 ) ) ;
#13703 = FACE_OUTER_BOUND ( 'NONE', #21415, .T. ) ;
#13704 = VERTEX_POINT ( 'NONE', #112982 ) ;
#13705 = CIRCLE ( 'NONE', #32525, 0.06509327318403745899 ) ;
#13706 = DIRECTION ( 'NONE',  ( 0.000000000000000000, 1.000000000000000000, 0.000000000000000000 ) ) ;
#13707 = DIRECTION ( 'NONE',  ( -0.000000000000000000, 1.000000000000000000, -0.000000000000000000 ) ) ;
#13708 = FACE_OUTER_BOUND ( 'NONE', #79972, .T. ) ;
#13709 = DIRECTION ( 'NONE',  ( 0.000000000000000000, 0.000000000000000000, 1.000000000000000000 ) ) ;
#13710 = CARTESIAN_POINT ( 'NONE',  ( -10.45000000000000107, 2.500000000000000000, 6.395190528383296602 ) ) ;
#13711 = AXIS2_PLACEMENT_3D ( 'NONE', #34874, #63678, #74781 ) ;
#13712 = EDGE_LOOP ( 'NONE', ( #111843, #60130 ) ) ;
#13713 = EDGE_CURVE ( 'NONE', #18092, #122603, #91765, .T. ) ;
#13714 = EDGE_LOOP ( 'NONE', ( #116360, #29678 ) ) ;
#13715 = CARTESIAN_POINT ( 'NONE',  ( -4.600000000000025402, 12.50000000000000000, 4.330127018922196314 ) ) ;
#13716 = DIRECTION ( 'NONE',  ( 0.000000000000000000, 0.000000000000000000, 1.000000000000000000 ) ) ;
#13719 = ORIENTED_EDGE ( 'NONE', *, *, #26864, .F. ) ;
#13718 = ORIENTED_EDGE ( 'NONE', *, *, #29086, .T. ) ;
#13717 = CONICAL_SURFACE ( 'NONE', #11676, 0.1000000000000002554, 0.003490658503988666988 ) ;
#13720 = ORIENTED_EDGE ( 'NONE', *, *, #56646, .F. ) ;
#13721 = DIRECTION ( 'NONE',  ( 0.000000000000000000, 1.000000000000000000, 0.000000000000000000 ) ) ;
#13722 = CONICAL_SURFACE ( 'NONE', #17939, 0.09999999999999982514, 0.003490658503988666988 ) ;
#13724 = VECTOR ( 'NONE', #119305, 1000.000000000000000 ) ;
#13723 = DIRECTION ( 'NONE',  ( 0.000000000000000000, -0.9999939076577903929, 0.003490651415223739937 ) ) ;
#13725 = CARTESIAN_POINT ( 'NONE',  ( -13.34999999999999076, 2.500000000000000000, 2.165063509461101265 ) ) ;
#13726 = AXIS2_PLACEMENT_3D ( 'NONE', #78796, #108862, #118692 ) ;
#13727 = PRESENTATION_STYLE_ASSIGNMENT (( #105348 ) ) ;
#13728 = CARTESIAN_POINT ( 'NONE',  ( -12.69999999999999218, 2.500000000000000000, -0.4464101615137741064 ) ) ;
#13729 = CARTESIAN_POINT ( 'NONE',  ( 184.9062500006828031, -8.891194145520236347, -1.633285867636356299E-15 ) ) ;
#13730 = DIRECTION ( 'NONE',  ( 0.000000000000000000, -0.000000000000000000, 1.000000000000000000 ) ) ;
#13731 = CIRCLE ( 'NONE', #43023, 0.06509327318403745899 ) ;
#13732 = FACE_OUTER_BOUND ( 'NONE', #92275, .T. ) ;
#13733 = CARTESIAN_POINT ( 'NONE',  ( -7.900000000000011013, 2.500000000000000000, 3.537306695894645081 ) ) ;
#13734 = PLANE ( 'NONE',  #56117 ) ;
#13735 = VERTEX_POINT ( 'NONE', #69340 ) ;
#13736 = DIRECTION ( 'NONE',  ( 0.000000000000000000, 0.000000000000000000, 1.000000000000000000 ) ) ;
#13737 = ORIENTED_EDGE ( 'NONE', *, *, #51079, .F. ) ;
#13738 = ORIENTED_EDGE ( 'NONE', *, *, #81915, .T. ) ;
#13739 = CARTESIAN_POINT ( 'NONE',  ( -8.950000000000009948, 12.50000000000000000, -1.818653347947326138 ) ) ;
#13740 = DIRECTION ( 'NONE',  ( -0.000000000000000000, 1.000000000000000000, -0.000000000000000000 ) ) ;
#13741 = CONICAL_SURFACE ( 'NONE', #61894, 0.1000000000000000056, 0.003490658503988666988 ) ;
#13742 = PLANE ( 'NONE',  #84182 ) ;
#13743 = DIRECTION ( 'NONE',  ( 0.000000000000000000, 0.000000000000000000, 1.000000000000000000 ) ) ;
#13745 = DIRECTION ( 'NONE',  ( 0.000000000000000000, 0.000000000000000000, 1.000000000000000000 ) ) ;
#13744 = PRODUCT_DEFINITION_SHAPE ( 'NONE', 'NONE',  #129625 ) ;
#13746 = CARTESIAN_POINT ( 'NONE',  ( 185.8229166673494319, -4.445597072760079982, 7.700000000000070344 ) ) ;
#13747 = CARTESIAN_POINT ( 'NONE',  ( 11.24999999999994316, 2.500000000000000000, 2.165063509461097713 ) ) ;
#13748 = ORIENTED_EDGE ( 'NONE', *, *, #54287, .T. ) ;
#13749 = DIRECTION ( 'NONE',  ( 0.000000000000000000, 0.000000000000000000, -1.000000000000000000 ) ) ;
#13750 = AXIS2_PLACEMENT_3D ( 'NONE', #48485, #98218, #58322 ) ;
#13751 = CIRCLE ( 'NONE', #78636, 0.1000000000000002554 ) ;
#13752 = CIRCLE ( 'NONE', #101604, 0.1000000000000002554 ) ;
#13753 = CARTESIAN_POINT ( 'NONE',  ( -6.850000000000017408, 2.500000000000000000, -2.511473670974877948 ) ) ;
#13754 = ORIENTED_EDGE ( 'NONE', *, *, #70109, .F. ) ;
#13755 = EDGE_CURVE ( 'NONE', #28046, #11893, #129594, .T. ) ;
#13756 = ORIENTED_EDGE ( 'NONE', *, *, #81773, .T. ) ;
#13757 = AXIS2_PLACEMENT_3D ( 'NONE', #98195, #87721, #36062 ) ;
#13758 = ORIENTED_EDGE ( 'NONE', *, *, #34230, .T. ) ;
#13759 = ADVANCED_FACE ( 'NONE', ( #62609 ), #39913, .T. ) ;
#13760 = VERTEX_POINT ( 'NONE', #3673 ) ;
#13761 = EDGE_CURVE ( 'NONE', #62383, #61737, #22691, .T. ) ;
#13762 = DIRECTION ( 'NONE',  ( -0.000000000000000000, -1.000000000000000000, -0.000000000000000000 ) ) ;
#13763 = FACE_OUTER_BOUND ( 'NONE', #99855, .T. ) ;
#13764 = AXIS2_PLACEMENT_3D ( 'NONE', #80494, #68711, #108638 ) ;
#13765 = DIRECTION ( 'NONE',  ( 0.000000000000000000, -0.9999939076577903929, 0.003490651415223739937 ) ) ;
#13766 = LINE ( 'NONE', #53704, #4741 ) ;
#13768 = CIRCLE ( 'NONE', #91152, 0.1000000000000002554 ) ;
#13767 = AXIS2_PLACEMENT_3D ( 'NONE', #125601, #47073, #27395 ) ;
#13769 = EDGE_CURVE ( 'NONE', #88360, #17776, #45810, .T. ) ;
#13770 = DIRECTION ( 'NONE',  ( 0.000000000000000000, 0.000000000000000000, 1.000000000000000000 ) ) ;
#13772 = ORIENTED_EDGE ( 'NONE', *, *, #108457, .T. ) ;
#13771 = ADVANCED_FACE ( 'NONE', ( #30099 ), #116880, .T. ) ;
#13773 = DIRECTION ( 'NONE',  ( -0.000000000000000000, -1.000000000000000000, -0.000000000000000000 ) ) ;
#13774 = EDGE_CURVE ( 'NONE', #74262, #46085, #52770, .T. ) ;
#13775 = DIRECTION ( 'NONE',  ( 0.000000000000000000, 1.000000000000000000, 0.000000000000000000 ) ) ;
#13776 = EDGE_CURVE ( 'NONE', #57128, #103454, #119736, .T. ) ;
#13777 = CARTESIAN_POINT ( 'NONE',  ( -12.49999999999999289, 2.500000000000000000, -5.122947341949751987 ) ) ;
#13778 = DIRECTION ( 'NONE',  ( -0.000000000000000000, -1.000000000000000000, -0.000000000000000000 ) ) ;
#13779 = EDGE_LOOP ( 'NONE', ( #108950, #115453, #30838, #23655 ) ) ;
#13780 = VERTEX_POINT ( 'NONE', #109937 ) ;
#13781 = ORIENTED_EDGE ( 'NONE', *, *, #107633, .F. ) ;
#13782 = FACE_OUTER_BOUND ( 'NONE', #103297, .T. ) ;
#13783 = EDGE_CURVE ( 'NONE', #83794, #65306, #89710, .T. ) ;
#13784 = CARTESIAN_POINT ( 'NONE',  ( 2.899999999999946620, 2.500000000000000000, -3.537306695894649966 ) ) ;
#13785 = CARTESIAN_POINT ( 'NONE',  ( -11.24999999999996270, 2.500000000000000000, 2.165063509461097713 ) ) ;
#13786 = ORIENTED_EDGE ( 'NONE', *, *, #33497, .F. ) ;
#13787 = LINE ( 'NONE', #102809, #85007 ) ;
#13788 = DIRECTION ( 'NONE',  ( 0.000000000000000000, 0.000000000000000000, 1.000000000000000000 ) ) ;
#13789 = DIRECTION ( 'NONE',  ( -4.274815082592931898E-19, -0.9999939076577903929, -0.003490651415223739937 ) ) ;
#13790 = CARTESIAN_POINT ( 'NONE',  ( -0.8500000000000386136, 2.500000000000000000, 5.902370205355745192 ) ) ;
#13791 = AXIS2_PLACEMENT_3D ( 'NONE', #17731, #17062, #57011 ) ;
#13792 = CARTESIAN_POINT ( 'NONE',  ( -1.650000000000034328, 12.50000000000000000, -6.495190528383302464 ) ) ;
#13793 = VECTOR ( 'NONE', #45196, 1000.000000000000000 ) ;
#13794 = ORIENTED_EDGE ( 'NONE', *, *, #56774, .T. ) ;
#13795 = EDGE_LOOP ( 'NONE', ( #50717, #19584 ) ) ;
#13796 = EDGE_CURVE ( 'NONE', #113294, #14153, #20257, .T. ) ;
#13797 = DIRECTION ( 'NONE',  ( -0.000000000000000000, 1.000000000000000000, -0.000000000000000000 ) ) ;
#13798 = DIRECTION ( 'NONE',  ( 0.000000000000000000, 0.000000000000000000, -1.000000000000000000 ) ) ;
#13799 = LINE ( 'NONE', #113298, #47055 ) ;
#13800 = DIRECTION ( 'NONE',  ( 0.000000000000000000, -0.000000000000000000, 1.000000000000000000 ) ) ;
#13801 = AXIS2_PLACEMENT_3D ( 'NONE', #126210, #8999, #106558 ) ;
#13802 = FACE_OUTER_BOUND ( 'NONE', #109017, .T. ) ;
#13803 = ORIENTED_EDGE ( 'NONE', *, *, #15112, .T. ) ;
#13804 = EDGE_CURVE ( 'NONE', #24108, #124192, #23966, .T. ) ;
#13805 = ORIENTED_EDGE ( 'NONE', *, *, #39599, .F. ) ;
#13806 = ADVANCED_FACE ( 'NONE', ( #79194 ), #9788, .T. ) ;
#13807 = DIRECTION ( 'NONE',  ( 0.000000000000000000, -0.000000000000000000, 1.000000000000000000 ) ) ;
#13808 = CARTESIAN_POINT ( 'NONE',  ( -7.100000000000017408, 2.500000000000000000, -3.737306695894649700 ) ) ;
#13809 = DIRECTION ( 'NONE',  ( 0.000000000000000000, 1.000000000000000000, 0.000000000000000000 ) ) ;
#13810 = EDGE_CURVE ( 'NONE', #72978, #125967, #43765, .T. ) ;
#13811 = CYLINDRICAL_SURFACE ( 'NONE', #120018, 5.000000000000000000 ) ;
#13812 = VERTEX_POINT ( 'NONE', #6227 ) ;
#13813 = CONICAL_SURFACE ( 'NONE', #105865, 0.09999999999999982514, 0.003490658503988666988 ) ;
#13814 = DIRECTION ( 'NONE',  ( -4.274815082592931898E-19, -0.9999939076577903929, -0.003490651415223739937 ) ) ;
#13815 = EDGE_CURVE ( 'NONE', #57879, #22979, #84806, .T. ) ;
#13816 = VECTOR ( 'NONE', #40656, 1000.000000000000000 ) ;
#13817 = LINE ( 'NONE', #113968, #28508 ) ;
#13818 = EDGE_CURVE ( 'NONE', #122473, #77164, #123167, .T. ) ;
#13819 = ORIENTED_EDGE ( 'NONE', *, *, #23379, .F. ) ;
#13820 = FACE_OUTER_BOUND ( 'NONE', #112830, .T. ) ;
#13821 = EDGE_CURVE ( 'NONE', #10798, #73823, #114268, .T. ) ;
#13822 = ORIENTED_EDGE ( 'NONE', *, *, #36976, .T. ) ;
#13823 = DIRECTION ( 'NONE',  ( 0.000000000000000000, 1.000000000000000000, 0.000000000000000000 ) ) ;
#13824 = EDGE_CURVE ( 'NONE', #12959, #113477, #26543, .T. ) ;
#13825 = EDGE_CURVE ( 'NONE', #69331, #17546, #22836, .T. ) ;
#13826 = EDGE_CURVE ( 'NONE', #87887, #19796, #100182, .T. ) ;
#13827 = ORIENTED_EDGE ( 'NONE', *, *, #27127, .F. ) ;
#13828 = CARTESIAN_POINT ( 'NONE',  ( 4.599999999999936584, 2.500000000000000000, 3.637306695894644726 ) ) ;
#13829 = CARTESIAN_POINT ( 'NONE',  ( -1.250000000000035749, 2.500000000000000000, -7.088010851410853519 ) ) ;
#13830 = ORIENTED_EDGE ( 'NONE', *, *, #112679, .T. ) ;
#13831 = VERTEX_POINT ( 'NONE', #124090 ) ;
#13832 = CARTESIAN_POINT ( 'NONE',  ( 185.7552083336747444, 6.551208109652275624, -3.782341765624998686 ) ) ;
#13833 = CARTESIAN_POINT ( 'NONE',  ( -4.550000000000022915, 2.500000000000000000, 6.495190528383297135 ) ) ;
#13834 = VECTOR ( 'NONE', #120928, 1000.000000000000000 ) ;
#13835 = ADVANCED_FACE ( 'NONE', ( #95920 ), #95971, .T. ) ;
#13836 = CARTESIAN_POINT ( 'NONE',  ( 186.2552083336747444, 6.551208109652275624, -3.782341765624998686 ) ) ;
#13837 = CARTESIAN_POINT ( 'NONE',  ( 184.8593750003413732, 0.000000000000000000, 7.564683531250000925 ) ) ;
#13838 = AXIS2_PLACEMENT_3D ( 'NONE', #12772, #33719, #113575 ) ;
#13839 = DIRECTION ( 'NONE',  ( -0.000000000000000000, -1.000000000000000000, -0.000000000000000000 ) ) ;
#13840 = CARTESIAN_POINT ( 'NONE',  ( 3.549999999999944755, 12.50000000000000000, -6.841600689897077814 ) ) ;
#13841 = DIRECTION ( 'NONE',  ( 0.000000000000000000, 1.000000000000000000, 0.000000000000000000 ) ) ;
#13842 = CIRCLE ( 'NONE', #95430, 3.000000000000000000 ) ;
#13843 = DIRECTION ( 'NONE',  ( -4.274815082592931898E-19, -0.9999939076577903929, -0.003490651415223739937 ) ) ;
#13844 = CIRCLE ( 'NONE', #20123, 0.09999999999999982514 ) ;
#13845 = AXIS2_PLACEMENT_3D ( 'NONE', #81939, #91128, #149 ) ;
#13846 = ORIENTED_EDGE ( 'NONE', *, *, #62106, .F. ) ;
#13847 = AXIS2_PLACEMENT_3D ( 'NONE', #54259, #33978, #73895 ) ;
#13848 = VERTEX_POINT ( 'NONE', #4947 ) ;
#13849 = DIRECTION ( 'NONE',  ( 0.000000000000000000, 0.000000000000000000, 1.000000000000000000 ) ) ;
#13850 = ORIENTED_EDGE ( 'NONE', *, *, #61674, .F. ) ;
#13851 = CARTESIAN_POINT ( 'NONE',  ( -12.09999999999999609, 2.500000000000000000, -3.637306695894647390 ) ) ;
#13852 = FACE_OUTER_BOUND ( 'NONE', #64018, .T. ) ;
#13853 = FACE_OUTER_BOUND ( 'NONE', #8807, .T. ) ;
#13855 = ORIENTED_EDGE ( 'NONE', *, *, #4207, .T. ) ;
#13854 = ORIENTED_EDGE ( 'NONE', *, *, #91572, .F. ) ;
#13856 = DIRECTION ( 'NONE',  ( -4.274815082592931898E-19, -0.9999939076577903929, -0.003490651415223739937 ) ) ;
#13857 = EDGE_LOOP ( 'NONE', ( #22699, #51731, #25820, #123209 ) ) ;
#13858 = CARTESIAN_POINT ( 'NONE',  ( 11.44999999999990692, 2.500000000000000000, 1.818653347947321475 ) ) ;
#13859 = DIRECTION ( 'NONE',  ( 0.000000000000000000, 0.000000000000000000, 1.000000000000000000 ) ) ;
#13860 = AXIS2_PLACEMENT_3D ( 'NONE', #14917, #27330, #55533 ) ;
#13861 = DIRECTION ( 'NONE',  ( -0.000000000000000000, -1.000000000000000000, -0.000000000000000000 ) ) ;
#13862 = CARTESIAN_POINT ( 'NONE',  ( -13.09999999999999254, 12.50000000000000000, -4.676537180435975216 ) ) ;
#13863 = CARTESIAN_POINT ( 'NONE',  ( 10.39999999999990976, 12.50000000000000000, 4.330127018922196314 ) ) ;
#13865 = VECTOR ( 'NONE', #13046, 1000.000000000000000 ) ;
#13864 = VECTOR ( 'NONE', #8408, 1000.000000000000000 ) ;
#13866 = DIRECTION ( 'NONE',  ( 0.000000000000000000, 0.000000000000000000, 1.000000000000000000 ) ) ;
#13867 = CARTESIAN_POINT ( 'NONE',  ( -5.400000000000019895, 2.500000000000000000, 4.330127018922196314 ) ) ;
#13868 = LINE ( 'NONE', #33535, #104875 ) ;
#13869 = CARTESIAN_POINT ( 'NONE',  ( 186.0677083336747444, -4.367472073101514418, -7.564683531250002702 ) ) ;
#13870 = DIRECTION ( 'NONE',  ( -0.000000000000000000, -1.000000000000000000, -0.000000000000000000 ) ) ;
#13871 = CARTESIAN_POINT ( 'NONE',  ( 3.749999999999976907, 12.50000000000000000, 2.165063509461097713 ) ) ;
#13872 = EDGE_LOOP ( 'NONE', ( #63528, #49035 ) ) ;
#13873 = VERTEX_POINT ( 'NONE', #45547 ) ;
#13874 = EDGE_CURVE ( 'NONE', #94218, #83042, #106381, .T. ) ;
#13875 = ORIENTED_EDGE ( 'NONE', *, *, #104846, .F. ) ;
#13876 = DIRECTION ( 'NONE',  ( -0.000000000000000000, -1.000000000000000000, -0.000000000000000000 ) ) ;
#13877 = ORIENTED_EDGE ( 'NONE', *, *, #118017, .F. ) ;
#13878 = DIRECTION ( 'NONE',  ( 0.000000000000000000, 0.000000000000000000, 1.000000000000000000 ) ) ;
#13880 = ORIENTED_EDGE ( 'NONE', *, *, #36285, .T. ) ;
#13879 = ORIENTED_EDGE ( 'NONE', *, *, #51485, .T. ) ;
#13881 = EDGE_LOOP ( 'NONE', ( #50627, #121778, #11457, #127616 ) ) ;
#13882 = DIRECTION ( 'NONE',  ( 0.000000000000000000, 0.000000000000000000, 1.000000000000000000 ) ) ;
#13883 = DIRECTION ( 'NONE',  ( 0.000000000000000000, 0.000000000000000000, -1.000000000000000000 ) ) ;
#13884 = SURFACE_STYLE_USAGE ( .BOTH. , #5990 ) ;
#13885 = DIRECTION ( 'NONE',  ( 0.000000000000000000, 1.000000000000000000, 0.000000000000000000 ) ) ;
#13886 = DIRECTION ( 'NONE',  ( 0.000000000000000000, -0.000000000000000000, 1.000000000000000000 ) ) ;
#13887 = DIRECTION ( 'NONE',  ( 0.000000000000000000, 0.000000000000000000, -1.000000000000000000 ) ) ;
#13888 = EDGE_CURVE ( 'NONE', #95786, #63967, #72990, .T. ) ;
#13889 = VERTEX_POINT ( 'NONE', #126676 ) ;
#13890 = DIRECTION ( 'NONE',  ( 0.000000000000000000, 0.000000000000000000, 1.000000000000000000 ) ) ;
#13891 = ORIENTED_EDGE ( 'NONE', *, *, #15919, .F. ) ;
#13893 = ORIENTED_EDGE ( 'NONE', *, *, #62126, .T. ) ;
#13892 = AXIS2_PLACEMENT_3D ( 'NONE', #114495, #45134, #85033 ) ;
#13894 = ORIENTED_EDGE ( 'NONE', *, *, #99826, .F. ) ;
#13895 = VECTOR ( 'NONE', #94271, 1000.000000000000000 ) ;
#13896 = FACE_OUTER_BOUND ( 'NONE', #126561, .T. ) ;
#13897 = VERTEX_POINT ( 'NONE', #16689 ) ;
#13898 = ORIENTED_EDGE ( 'NONE', *, *, #95079, .F. ) ;
#13899 = ORIENTED_EDGE ( 'NONE', *, *, #4781, .F. ) ;
#13900 = DIRECTION ( 'NONE',  ( 0.000000000000000000, 0.000000000000000000, 1.000000000000000000 ) ) ;
#13902 = AXIS2_PLACEMENT_3D ( 'NONE', #100308, #69540, #45572 ) ;
#13901 = CIRCLE ( 'NONE', #59910, 0.06509327318403745899 ) ;
#13903 = DIRECTION ( 'NONE',  ( 0.000000000000000000, 0.000000000000000000, 1.000000000000000000 ) ) ;
#13904 = DIRECTION ( 'NONE',  ( 0.000000000000000000, 1.000000000000000000, 0.000000000000000000 ) ) ;
#13905 = PLANE ( 'NONE',  #31690 ) ;
#13906 = LINE ( 'NONE', #85237, #38802 ) ;
#13907 = DIRECTION ( 'NONE',  ( 0.000000000000000000, 1.000000000000000000, 0.000000000000000000 ) ) ;
#13908 = CARTESIAN_POINT ( 'NONE',  ( 7.899999999999923084, 2.500000000000000000, 0.6928203230275494784 ) ) ;
#13910 = AXIS2_PLACEMENT_3D ( 'NONE', #780, #41379, #62303 ) ;
#13909 = CIRCLE ( 'NONE', #126799, 0.09999999999999982514 ) ;
#13911 = ORIENTED_EDGE ( 'NONE', *, *, #119077, .T. ) ;
#13912 = FACE_OUTER_BOUND ( 'NONE', #15011, .T. ) ;
#13914 = EDGE_CURVE ( 'NONE', #95931, #129515, #118403, .T. ) ;
#13913 = AXIS2_PLACEMENT_3D ( 'NONE', #64128, #93593, #1980 ) ;
#13915 = ORIENTED_EDGE ( 'NONE', *, *, #52068, .T. ) ;
#13916 = CARTESIAN_POINT ( 'NONE',  ( 185.8229166673494319, -4.445597072760079982, 7.700000000000070344 ) ) ;
#13917 = ORIENTED_EDGE ( 'NONE', *, *, #112345, .F. ) ;
#13918 = EDGE_LOOP ( 'NONE', ( #98523, #55265 ) ) ;
#13919 = EDGE_CURVE ( 'NONE', #14887, #35541, #64116, .T. ) ;
#13920 = DIRECTION ( 'NONE',  ( -0.000000000000000000, 1.000000000000000000, -0.000000000000000000 ) ) ;
#13921 = DIRECTION ( 'NONE',  ( -4.274815082592931898E-19, -0.9999939076577903929, -0.003490651415223739937 ) ) ;
#13922 = DIRECTION ( 'NONE',  ( 0.000000000000000000, 0.000000000000000000, -1.000000000000000000 ) ) ;
#13923 = ORIENTED_EDGE ( 'NONE', *, *, #126370, .F. ) ;
#13924 = ADVANCED_FACE ( 'NONE', ( #74347 ), #45251, .T. ) ;
#13926 = VERTEX_POINT ( 'NONE', #76931 ) ;
#13925 = EDGE_CURVE ( 'NONE', #48111, #26681, #86741, .T. ) ;
#13927 = CARTESIAN_POINT ( 'NONE',  ( 3.949999999999938893, 12.50000000000000000, 6.083687093685482772 ) ) ;
#13928 = CARTESIAN_POINT ( 'NONE',  ( 8.949999999999917577, 12.50000000000000000, -2.511473670974877948 ) ) ;
#13929 = EDGE_CURVE ( 'NONE', #104068, #11740, #91224, .T. ) ;
#13930 = DIRECTION ( 'NONE',  ( -0.000000000000000000, 1.000000000000000000, -0.000000000000000000 ) ) ;
#13931 = EDGE_CURVE ( 'NONE', #11186, #37345, #4288, .T. ) ;
#13932 = CONICAL_SURFACE ( 'NONE', #47402, 0.09999999999999982514, 0.003490658503988666988 ) ;
#13933 = EDGE_CURVE ( 'NONE', #128871, #98765, #116836, .T. ) ;
#13934 = DIRECTION ( 'NONE',  ( -0.000000000000000000, 1.000000000000000000, -0.000000000000000000 ) ) ;
#13935 = CARTESIAN_POINT ( 'NONE',  ( -0.4000000000000392131, 2.500000000000000000, -5.122947341949753763 ) ) ;
#13936 = ORIENTED_EDGE ( 'NONE', *, *, #113826, .T. ) ;
#13937 = B_SPLINE_CURVE_WITH_KNOTS ( 'NONE', 3,
 ( #20442, #100299, #10594, #99653, #81300, #30281, #39467, #121860, #121213, #31555, #79374, #69531, #40751, #50532, #791, #71462 ),
 .UNSPECIFIED., .F., .F.,
 ( 4, 2, 2, 2, 2, 2, 2, 4 ),
 ( 0.000000000000000000, 0.0008828639377709713437, 0.001765727875541942687, 0.003531455751083888411, 0.005297183626625834134, 0.007062911502167780291, 0.01059436725325167694, 0.01412582300433557272 ),
 .UNSPECIFIED. ) ;
#13938 = EDGE_CURVE ( 'NONE', #82940, #65438, #70384, .T. ) ;
#13939 = EDGE_LOOP ( 'NONE', ( #35323, #31126, #128553, #105815 ) ) ;
#13940 = CIRCLE ( 'NONE', #49483, 0.06509327318403745899 ) ;
#13941 = EDGE_CURVE ( 'NONE', #121566, #84561, #107942, .T. ) ;
#13942 = DIRECTION ( 'NONE',  ( -0.000000000000000000, -1.000000000000000000, -0.000000000000000000 ) ) ;
#13943 = DIRECTION ( 'NONE',  ( -0.000000000000000000, -1.000000000000000000, -0.000000000000000000 ) ) ;
#13944 = EDGE_CURVE ( 'NONE', #10631, #41518, #32752, .T. ) ;
#13945 = AXIS2_PLACEMENT_3D ( 'NONE', #127776, #118597, #38117 ) ;
#13946 = CARTESIAN_POINT ( 'NONE',  ( 184.2552083336747444, 6.551208109652275624, -3.782341765624998686 ) ) ;
#13948 = VECTOR ( 'NONE', #51096, 1000.000000000000000 ) ;
#13947 = LINE ( 'NONE', #114731, #36464 ) ;
#13949 = FACE_OUTER_BOUND ( 'NONE', #60071, .T. ) ;
#13950 = FACE_OUTER_BOUND ( 'NONE', #87132, .T. ) ;
#13951 = DIRECTION ( 'NONE',  ( -0.000000000000000000, -1.000000000000000000, -0.000000000000000000 ) ) ;
#13952 = EDGE_LOOP ( 'NONE', ( #89486, #20805, #69898, #17945 ) ) ;
#13953 = CIRCLE ( 'NONE', #112171, 0.06509327318403745899 ) ;
#13954 = CARTESIAN_POINT ( 'NONE',  ( -13.34999999999999076, 12.50000000000000000, -2.165063509461099489 ) ) ;
#13956 = CIRCLE ( 'NONE', #24433, 0.09999999999999982514 ) ;
#13955 = CIRCLE ( 'NONE', #85067, 0.06509327318403745899 ) ;
#13957 = DIRECTION ( 'NONE',  ( 0.000000000000000000, -0.9999939076577903929, 0.003490651415223739937 ) ) ;
#13958 = CARTESIAN_POINT ( 'NONE',  ( 0.8499999999999553468, 2.500000000000000000, -2.757883832488654097 ) ) ;
#13959 = ORIENTED_EDGE ( 'NONE', *, *, #40890, .T. ) ;
#13960 = CARTESIAN_POINT ( 'NONE',  ( 9.799999999999913669, 12.50000000000000000, 4.676537180435972552 ) ) ;
#13961 = EDGE_LOOP ( 'NONE', ( #112653, #80659 ) ) ;
#13962 = CARTESIAN_POINT ( 'NONE',  ( -1.900000000000034106, 2.500000000000000000, 0.3464101615137735735 ) ) ;
#13963 = ORIENTED_EDGE ( 'NONE', *, *, #94959, .T. ) ;
#13964 = DIRECTION ( 'NONE',  ( 0.000000000000000000, 0.000000000000000000, 1.000000000000000000 ) ) ;
#13965 = DIRECTION ( 'NONE',  ( 0.000000000000000000, 0.000000000000000000, 1.000000000000000000 ) ) ;
#13966 = AXIS2_PLACEMENT_3D ( 'NONE', #92777, #73754, #13549 ) ;
#13967 = CARTESIAN_POINT ( 'NONE',  ( 8.349999999999919709, 2.500000000000000000, -2.857883832488653741 ) ) ;
#13968 = VERTEX_POINT ( 'NONE', #108943 ) ;
#13969 = DIRECTION ( 'NONE',  ( 0.000000000000000000, -0.000000000000000000, 1.000000000000000000 ) ) ;
#13970 = CARTESIAN_POINT ( 'NONE',  ( -8.950000000000009948, 2.500000000000000000, 2.411473670974873862 ) ) ;
#13971 = EDGE_CURVE ( 'NONE', #6869, #86595, #37660, .T. ) ;
#13972 = EDGE_LOOP ( 'NONE', ( #84717, #41693, #92938, #7328 ) ) ;
#13973 = EDGE_CURVE ( 'NONE', #9476, #13889, #27818, .T. ) ;
#13974 = AXIS2_PLACEMENT_3D ( 'NONE', #18872, #8402, #36613 ) ;
#13975 = ORIENTED_EDGE ( 'NONE', *, *, #103601, .T. ) ;
#13976 = VECTOR ( 'NONE', #99453, 1000.000000000000000 ) ;
#13977 = EDGE_CURVE ( 'NONE', #20697, #13290, #20215, .T. ) ;
#13978 = EDGE_LOOP ( 'NONE', ( #83134, #43120 ) ) ;
#13979 = FACE_OUTER_BOUND ( 'NONE', #91749, .T. ) ;
#13980 = DIRECTION ( 'NONE',  ( 0.000000000000000000, -0.000000000000000000, 1.000000000000000000 ) ) ;
#13981 = DIRECTION ( 'NONE',  ( -0.000000000000000000, 1.000000000000000000, -0.000000000000000000 ) ) ;
#13982 = ORIENTED_EDGE ( 'NONE', *, *, #10418, .F. ) ;
#13983 = CARTESIAN_POINT ( 'NONE',  ( 2.099999999999948574, 2.500000000000000000, 3.637306695894644726 ) ) ;
#13984 = LINE ( 'NONE', #112208, #81585 ) ;
#13985 = VERTEX_POINT ( 'NONE', #120085 ) ;
#13986 = EDGE_CURVE ( 'NONE', #27533, #41344, #99631, .T. ) ;
#13987 = VECTOR ( 'NONE', #42467, 1000.000000000000000 ) ;
#13988 = DIRECTION ( 'NONE',  ( -0.000000000000000000, -1.000000000000000000, -0.000000000000000000 ) ) ;
#13989 = DIRECTION ( 'NONE',  ( 0.000000000000000000, 0.000000000000000000, 1.000000000000000000 ) ) ;
#13990 = FACE_OUTER_BOUND ( 'NONE', #14692, .T. ) ;
#13991 = DIRECTION ( 'NONE',  ( 0.000000000000000000, 1.000000000000000000, 0.000000000000000000 ) ) ;
#13992 = DIRECTION ( 'NONE',  ( 0.000000000000000000, 0.000000000000000000, 1.000000000000000000 ) ) ;
#13993 = CARTESIAN_POINT ( 'NONE',  ( -4.400000000000028777, 12.50000000000000000, -3.918623584224389056 ) ) ;
#13994 = CARTESIAN_POINT ( 'NONE',  ( -10.60000000000000142, 12.50000000000000000, 0.3464101615137736845 ) ) ;
#13995 = AXIS2_PLACEMENT_3D ( 'NONE', #96897, #38656, #78575 ) ;
#13996 = CONICAL_SURFACE ( 'NONE', #60014, 0.1000000000000000472, 0.003490658503988666988 ) ;
#13997 = ORIENTED_EDGE ( 'NONE', *, *, #86402, .F. ) ;
#13998 = ORIENTED_EDGE ( 'NONE', *, *, #9634, .T. ) ;
#13999 = ORIENTED_EDGE ( 'NONE', *, *, #122429, .F. ) ;
#14000 = ORIENTED_EDGE ( 'NONE', *, *, #108363, .F. ) ;
#14001 = FACE_OUTER_BOUND ( 'NONE', #41097, .T. ) ;
#14002 = FACE_OUTER_BOUND ( 'NONE', #6717, .T. ) ;
#14003 = DIRECTION ( 'NONE',  ( -4.274815082592931898E-19, -0.9999939076577903929, -0.003490651415223739937 ) ) ;
#14004 = EDGE_LOOP ( 'NONE', ( #86123, #45825, #7526, #66310 ) ) ;
#14005 = FACE_BOUND ( 'NONE', #123227, .T. ) ;
#14006 = ADVANCED_FACE ( 'NONE', ( #89330 ), #112156, .T. ) ;
#14007 = DIRECTION ( 'NONE',  ( 0.000000000000000000, 0.000000000000000000, 1.000000000000000000 ) ) ;
#14008 = CARTESIAN_POINT ( 'NONE',  ( 7.699999999999925571, 12.50000000000000000, -4.676537180435978769 ) ) ;
#14009 = CARTESIAN_POINT ( 'NONE',  ( -10.60000000000000142, 2.500000000000000000, 0.3464101615137736845 ) ) ;
#14010 = CARTESIAN_POINT ( 'NONE',  ( 107.5000000000000142, -1.500000000000000222, -1.322875655532295136 ) ) ;
#14011 = CARTESIAN_POINT ( 'NONE',  ( -2.100000000000033396, 12.50000000000000000, -3.702399969078687292 ) ) ;
#14012 = DIRECTION ( 'NONE',  ( -0.000000000000000000, 1.000000000000000000, -0.000000000000000000 ) ) ;
#14013 = FACE_OUTER_BOUND ( 'NONE', #61402, .T. ) ;
#14014 = DIRECTION ( 'NONE',  ( 0.000000000000000000, 0.000000000000000000, 1.000000000000000000 ) ) ;
#14015 = CARTESIAN_POINT ( 'NONE',  ( 184.5000000000000000, 0.000000000000000000, -7.699999999999999289 ) ) ;
#14016 = AXIS2_PLACEMENT_3D ( 'NONE', #4509, #85676, #84392 ) ;
#14017 = CIRCLE ( 'NONE', #64199, 0.06509327318403745899 ) ;
#14018 = CARTESIAN_POINT ( 'NONE',  ( 2.099999999999948574, 2.500000000000000000, 4.330127018922196314 ) ) ;
#14019 = ORIENTED_EDGE ( 'NONE', *, *, #43973, .T. ) ;
#14020 = EDGE_LOOP ( 'NONE', ( #109836, #101801, #24691, #90109 ) ) ;
#14022 = ORIENTED_EDGE ( 'NONE', *, *, #43676, .F. ) ;
#14021 = AXIS2_PLACEMENT_3D ( 'NONE', #53914, #29601, #127803 ) ;
#14023 = EDGE_CURVE ( 'NONE', #23927, #67054, #41166, .T. ) ;
#14024 = ORIENTED_EDGE ( 'NONE', *, *, #124315, .F. ) ;
#14025 = ORIENTED_EDGE ( 'NONE', *, *, #34914, .T. ) ;
#14026 = ORIENTED_EDGE ( 'NONE', *, *, #35455, .F. ) ;
#14027 = FACE_OUTER_BOUND ( 'NONE', #10077, .T. ) ;
#14028 = VERTEX_POINT ( 'NONE', #20590 ) ;
#14030 = ORIENTED_EDGE ( 'NONE', *, *, #72648, .T. ) ;
#14029 = CONICAL_SURFACE ( 'NONE', #68412, 0.09999999999999982514, 0.003490658503988666988 ) ;
#14031 = CARTESIAN_POINT ( 'NONE',  ( 12.65326442612073166, -2.500000000000508038, 8.428886917615358243 ) ) ;
#14032 = CARTESIAN_POINT ( 'NONE',  ( 0.8499999999999550138, 12.50000000000000000, -5.802370205355749988 ) ) ;
#14033 = DIRECTION ( 'NONE',  ( -4.274815082592931898E-19, -0.9999939076577903929, -0.003490651415223739937 ) ) ;
#14034 = EDGE_CURVE ( 'NONE', #122281, #111372, #68221, .T. ) ;
#14035 = ORIENTED_EDGE ( 'NONE', *, *, #128982, .T. ) ;
#14036 = DIRECTION ( 'NONE',  ( 0.000000000000000000, -0.9999939076577903929, 0.003490651415223739937 ) ) ;
#14037 = EDGE_LOOP ( 'NONE', ( #78181, #9378, #69485, #119446 ) ) ;
#14039 = CIRCLE ( 'NONE', #51721, 0.06509327318403745899 ) ;
#14038 = VECTOR ( 'NONE', #125311, 1000.000000000000000 ) ;
#14040 = ORIENTED_EDGE ( 'NONE', *, *, #459, .T. ) ;
#14042 = ORIENTED_EDGE ( 'NONE', *, *, #75702, .F. ) ;
#14041 = FACE_OUTER_BOUND ( 'NONE', #126694, .T. ) ;
#14043 = CARTESIAN_POINT ( 'NONE',  ( 106.0514428414850272, 9.000000000000001776, 1.124999999999998002 ) ) ;
#14044 = ORIENTED_EDGE ( 'NONE', *, *, #59194, .T. ) ;
#14045 = UNCERTAINTY_MEASURE_WITH_UNIT (LENGTH_MEASURE( 1.000000000000000082E-05 ), #22472, 'distance_accuracy_value', 'NONE');
#14046 = CARTESIAN_POINT ( 'NONE',  ( -6.700000000000019718, 2.500000000000000000, -2.385244779468109755E-15 ) ) ;
#14047 = DIRECTION ( 'NONE',  ( -0.000000000000000000, 1.000000000000000000, -0.000000000000000000 ) ) ;
#14048 = DIRECTION ( 'NONE',  ( 0.000000000000000000, 0.000000000000000000, 1.000000000000000000 ) ) ;
#14049 = CARTESIAN_POINT ( 'NONE',  ( 1.449999999999949551, 2.500000000000000000, 6.741600689897071952 ) ) ;
#14050 = LINE ( 'NONE', #15985, #127640 ) ;
#14051 = AXIS2_PLACEMENT_3D ( 'NONE', #99222, #89396, #29206 ) ;
#14052 = ORIENTED_EDGE ( 'NONE', *, *, #111186, .T. ) ;
#14053 = LINE ( 'NONE', #54006, #107547 ) ;
#14054 = ORIENTED_EDGE ( 'NONE', *, *, #11463, .T. ) ;
#14055 = CARTESIAN_POINT ( 'NONE',  ( 87.50000000000001421, 4.424430252271040587, -6.079088403633664761 ) ) ;
#14056 = ADVANCED_FACE ( 'NONE', ( #49417 ), #24415, .T. ) ;
#14057 = VERTEX_POINT ( 'NONE', #39611 ) ;
#14058 = CARTESIAN_POINT ( 'NONE',  ( 4.149999999999938183, 2.500000000000000000, 2.065063509461097624 ) ) ;
#14059 = CARTESIAN_POINT ( 'NONE',  ( 0.000000000000000000, 1.500000000000000000, -8.999999999999998224 ) ) ;
#14060 = CARTESIAN_POINT ( 'NONE',  ( 8.299999999999922551, 12.50000000000000000, 4.330127018922196314 ) ) ;
#14061 = DIRECTION ( 'NONE',  ( 0.000000000000000000, 1.000000000000000000, 0.000000000000000000 ) ) ;
#14062 = ORIENTED_EDGE ( 'NONE', *, *, #52955, .F. ) ;
#14063 = EDGE_CURVE ( 'NONE', #114185, #115197, #82912, .T. ) ;
#14064 =( NAMED_UNIT ( * ) SI_UNIT ( $, .STERADIAN. ) SOLID_ANGLE_UNIT ( ) );
#14065 = AXIS2_PLACEMENT_3D ( 'NONE', #74435, #35166, #94703 ) ;
#14066 = AXIS2_PLACEMENT_3D ( 'NONE', #81427, #33610, #72258 ) ;
#14067 = CARTESIAN_POINT ( 'NONE',  ( -13.54999999999999005, 12.50000000000000000, 2.446380397790839822 ) ) ;
#14068 = EDGE_LOOP ( 'NONE', ( #98199, #129505, #22050, #57791 ) ) ;
#14069 = ORIENTED_EDGE ( 'NONE', *, *, #6834, .F. ) ;
#14070 = EDGE_CURVE ( 'NONE', #51458, #78977, #97845, .T. ) ;
#14072 = EDGE_LOOP ( 'NONE', ( #72679, #31100 ) ) ;
#14071 = ADVANCED_FACE ( 'NONE', ( #109620 ), #101691, .T. ) ;
#14073 = FACE_OUTER_BOUND ( 'NONE', #65009, .T. ) ;
#14074 = FACE_OUTER_BOUND ( 'NONE', #96061, .T. ) ;
#14075 = ADVANCED_FACE ( 'NONE', ( #10126 ), #87092, .T. ) ;
#14076 = CARTESIAN_POINT ( 'NONE',  ( 184.6927083336747160, 6.551208109652275624, -3.782341765624998686 ) ) ;
#14077 = EDGE_CURVE ( 'NONE', #54383, #105257, #28479, .T. ) ;
#14078 = LINE ( 'NONE', #122134, #1016 ) ;
#14080 = VECTOR ( 'NONE', #116324, 1000.000000000000000 ) ;
#14079 = CONICAL_SURFACE ( 'NONE', #26617, 0.09999999999999982514, 0.003490658503988666988 ) ;
#14081 = CIRCLE ( 'NONE', #97717, 0.09999999999999999167 ) ;
#14082 = LINE ( 'NONE', #63203, #105398 ) ;
#14083 = PLANE ( 'NONE',  #94456 ) ;
#14084 = EDGE_CURVE ( 'NONE', #72875, #43830, #18138, .T. ) ;
#14085 = ADVANCED_FACE ( 'NONE', ( #118136 ), #110089, .T. ) ;
#14086 = EDGE_CURVE ( 'NONE', #121533, #111424, #110253, .T. ) ;
#14088 = CIRCLE ( 'NONE', #59830, 0.1000000000000002554 ) ;
#14087 = CIRCLE ( 'NONE', #1574, 0.1000000000000002554 ) ;
#14089 = ORIENTED_EDGE ( 'NONE', *, *, #32620, .T. ) ;
#14090 = EDGE_CURVE ( 'NONE', #32421, #21428, #128903, .T. ) ;
#14091 = PLANE ( 'NONE',  #115417 ) ;
#14092 = AXIS2_PLACEMENT_3D ( 'NONE', #56512, #29007, #68911 ) ;
#14093 = EDGE_CURVE ( 'NONE', #90527, #113481, #126816, .T. ) ;
#14094 = ORIENTED_EDGE ( 'NONE', *, *, #110465, .F. ) ;
#14095 = FACE_OUTER_BOUND ( 'NONE', #46471, .T. ) ;
#14096 = FACE_OUTER_BOUND ( 'NONE', #87873, .T. ) ;
#14097 = DIRECTION ( 'NONE',  ( 0.000000000000000000, 1.000000000000000000, 0.000000000000000000 ) ) ;
#14098 = CARTESIAN_POINT ( 'NONE',  ( -4.600000000000028066, 2.500000000000000000, -5.022947341949754119 ) ) ;
#14099 = EDGE_CURVE ( 'NONE', #88292, #121575, #47409, .T. ) ;
#14100 = EDGE_LOOP ( 'NONE', ( #78539, #37288 ) ) ;
#14101 = AXIS2_PLACEMENT_3D ( 'NONE', #72960, #110927, #70375 ) ;
#14102 = FACE_OUTER_BOUND ( 'NONE', #47291, .T. ) ;
#14104 = ORIENTED_EDGE ( 'NONE', *, *, #57355, .T. ) ;
#14103 = DIRECTION ( 'NONE',  ( 0.000000000000000000, 0.000000000000000000, -1.000000000000000000 ) ) ;
#14105 = AXIS2_PLACEMENT_3D ( 'NONE', #38697, #126408, #6590 ) ;
#14106 = AXIS2_PLACEMENT_3D ( 'NONE', #35939, #105967, #14348 ) ;
#14107 = VERTEX_POINT ( 'NONE', #21894 ) ;
#14108 = FACE_OUTER_BOUND ( 'NONE', #48034, .T. ) ;
#14109 = AXIS2_PLACEMENT_3D ( 'NONE', #61797, #72262, #91889 ) ;
#14110 = ORIENTED_EDGE ( 'NONE', *, *, #61238, .F. ) ;
#14111 = ORIENTED_EDGE ( 'NONE', *, *, #7424, .F. ) ;
#14112 = DIRECTION ( 'NONE',  ( 0.000000000000000000, -0.000000000000000000, 1.000000000000000000 ) ) ;
#14113 = AXIS2_PLACEMENT_3D ( 'NONE', #19161, #70228, #72168 ) ;
#14114 = ORIENTED_EDGE ( 'NONE', *, *, #105446, .T. ) ;
#14115 = DIRECTION ( 'NONE',  ( -4.274815082592931898E-19, -0.9999939076577903929, -0.003490651415223739937 ) ) ;
#14116 = CARTESIAN_POINT ( 'NONE',  ( -11.04999999999999893, 2.500000000000000000, 6.248780366869520542 ) ) ;
#14117 = AXIS2_PLACEMENT_3D ( 'NONE', #13382, #62511, #92598 ) ;
#14118 = CARTESIAN_POINT ( 'NONE',  ( -10.84999999999999964, 2.500000000000000000, 7.088010851410848190 ) ) ;
#14119 = VERTEX_POINT ( 'NONE', #122016 ) ;
#14120 = CIRCLE ( 'NONE', #35004, 0.09999999999999999167 ) ;
#14121 = AXIS2_PLACEMENT_3D ( 'NONE', #102669, #13641, #102041 ) ;
#14122 = DIRECTION ( 'NONE',  ( 0.000000000000000000, -0.9999939076577903929, 0.003490651415223739937 ) ) ;
#14124 = VERTEX_POINT ( 'NONE', #72280 ) ;
#14123 = CARTESIAN_POINT ( 'NONE',  ( 12.94999999999989981, 2.500000000000000000, -2.265063509461101798 ) ) ;
#14125 = CARTESIAN_POINT ( 'NONE',  ( 5.449999999999934452, 12.50000000000000000, 2.230156782645134950 ) ) ;
#14126 = AXIS2_PLACEMENT_3D ( 'NONE', #24051, #93431, #54152 ) ;
#14127 = DIRECTION ( 'NONE',  ( -0.000000000000000000, 1.000000000000000000, -0.000000000000000000 ) ) ;
#14128 = ORIENTED_EDGE ( 'NONE', *, *, #111024, .T. ) ;
#14129 = EDGE_CURVE ( 'NONE', #75768, #128878, #112190, .T. ) ;
#14131 = AXIS2_PLACEMENT_3D ( 'NONE', #85285, #6067, #75460 ) ;
#14130 = AXIS2_PLACEMENT_3D ( 'NONE', #49357, #89254, #39547 ) ;
#14132 = EDGE_LOOP ( 'NONE', ( #67047, #88585, #5866, #28705 ) ) ;
#14134 = EDGE_LOOP ( 'NONE', ( #87226, #31430 ) ) ;
#14133 = EDGE_CURVE ( 'NONE', #51338, #81852, #26476, .T. ) ;
#14135 = ORIENTED_EDGE ( 'NONE', *, *, #17592, .T. ) ;
#14136 = DIRECTION ( 'NONE',  ( 0.000000000000000000, 0.000000000000000000, 1.000000000000000000 ) ) ;
#14137 = DIRECTION ( 'NONE',  ( 0.000000000000000000, 0.000000000000000000, -1.000000000000000000 ) ) ;
#14138 = PLANE ( 'NONE',  #8646 ) ;
#14139 = FACE_BOUND ( 'NONE', #75103, .T. ) ;
#14140 = VERTEX_POINT ( 'NONE', #103002 ) ;
#14141 = CARTESIAN_POINT ( 'NONE',  ( 186.4427083336747160, -6.551208109652278289, 3.782341765624995134 ) ) ;
#14142 = DIRECTION ( 'NONE',  ( -0.000000000000000000, 1.000000000000000000, -0.000000000000000000 ) ) ;
#14143 = CARTESIAN_POINT ( 'NONE',  ( 8.749999999999953815, 2.500000000000000000, 6.495190528383297135 ) ) ;
#14144 = EDGE_CURVE ( 'NONE', #11222, #107586, #120556, .T. ) ;
#14145 = CARTESIAN_POINT ( 'NONE',  ( 0.8499999999999557909, 2.500000000000000000, -6.495190528383302464 ) ) ;
#14146 = CARTESIAN_POINT ( 'NONE',  ( -4.350000000000023626, 12.50000000000000000, 1.753560074763284016 ) ) ;
#14147 = AXIS2_PLACEMENT_3D ( 'NONE', #107878, #28689, #78448 ) ;
#14148 = CARTESIAN_POINT ( 'NONE',  ( -1.450000000000036371, 2.500000000000000000, 2.511473670974873507 ) ) ;
#14149 = CARTESIAN_POINT ( 'NONE',  ( 10.84999999999990905, 2.500000000000000000, -5.702370205355749455 ) ) ;
#14150 = ORIENTED_EDGE ( 'NONE', *, *, #113564, .F. ) ;
#14151 = ORIENTED_EDGE ( 'NONE', *, *, #121385, .T. ) ;
#14152 = ORIENTED_EDGE ( 'NONE', *, *, #127164, .T. ) ;
#14153 = VERTEX_POINT ( 'NONE', #3524 ) ;
#14154 = ORIENTED_EDGE ( 'NONE', *, *, #104839, .F. ) ;
#14155 = DIRECTION ( 'NONE',  ( 0.000000000000000000, -0.9999939076577903929, 0.003490651415223739937 ) ) ;
#14156 = CARTESIAN_POINT ( 'NONE',  ( 8.749999999999918288, 12.50000000000000000, 7.122917578226811486 ) ) ;
#14157 = ORIENTED_EDGE ( 'NONE', *, *, #18720, .F. ) ;
#14158 = FACE_BOUND ( 'NONE', #93206, .T. ) ;
#14159 = FACE_OUTER_BOUND ( 'NONE', #33240, .T. ) ;
#14160 = CIRCLE ( 'NONE', #33078, 0.1000000000000000472 ) ;
#14161 = AXIS2_PLACEMENT_3D ( 'NONE', #40053, #99623, #60352 ) ;
#14162 = ORIENTED_EDGE ( 'NONE', *, *, #6247, .F. ) ;
#14163 = CARTESIAN_POINT ( 'NONE',  ( 12.69999999999989981, 2.500000000000000000, -0.4464101615137783252 ) ) ;
#14164 = CARTESIAN_POINT ( 'NONE',  ( 4.799999999999939426, 12.50000000000000000, -4.676537180435977881 ) ) ;
#14165 = DIRECTION ( 'NONE',  ( -0.000000000000000000, -1.000000000000000000, -0.000000000000000000 ) ) ;
#14166 = EDGE_LOOP ( 'NONE', ( #86658, #20625, #26215, #43059 ) ) ;
#14167 = CARTESIAN_POINT ( 'NONE',  ( 15.83209681635537258, -2.500000000000000000, 5.404881881984331393 ) ) ;
#14168 = AXIS2_PLACEMENT_3D ( 'NONE', #88161, #78388, #118293 ) ;
#14169 = EDGE_CURVE ( 'NONE', #74255, #78385, #74586, .T. ) ;
#14170 = ORIENTED_EDGE ( 'NONE', *, *, #91259, .T. ) ;
#14171 = CONICAL_SURFACE ( 'NONE', #122860, 0.1000000000000002554, 0.003490658503988666988 ) ;
#14172 = CONICAL_SURFACE ( 'NONE', #120799, 0.1000000000000002554, 0.003490658503988666988 ) ;
#14173 = VERTEX_POINT ( 'NONE', #12679 ) ;
#14174 = VERTEX_POINT ( 'NONE', #11405 ) ;
#14175 = DIRECTION ( 'NONE',  ( -0.000000000000000000, -1.000000000000000000, -0.000000000000000000 ) ) ;
#14176 = FACE_OUTER_BOUND ( 'NONE', #10379, .T. ) ;
#14177 = DIRECTION ( 'NONE',  ( 0.000000000000000000, -0.9999939076577903929, 0.003490651415223739937 ) ) ;
#14178 = ORIENTED_EDGE ( 'NONE', *, *, #108057, .T. ) ;
#14179 = DIRECTION ( 'NONE',  ( 0.000000000000000000, 1.000000000000000000, 0.000000000000000000 ) ) ;
#14180 = CIRCLE ( 'NONE', #1667, 0.09999999999999999167 ) ;
#14181 = CARTESIAN_POINT ( 'NONE',  ( 11.69999999999990870, 2.500000000000000000, 4.230127018922196669 ) ) ;
#14182 = DIRECTION ( 'NONE',  ( 0.000000000000000000, 0.000000000000000000, -1.000000000000000000 ) ) ;
#14183 = CARTESIAN_POINT ( 'NONE',  ( 185.4479166673494603, -6.668395609140176816, -3.850000000000003642 ) ) ;
#14184 = ORIENTED_EDGE ( 'NONE', *, *, #88580, .F. ) ;
#14185 = EDGE_CURVE ( 'NONE', #25038, #5720, #28623, .T. ) ;
#14186 = FACE_OUTER_BOUND ( 'NONE', #24380, .T. ) ;
#14187 = EDGE_CURVE ( 'NONE', #83267, #72199, #53745, .T. ) ;
#14188 = ORIENTED_EDGE ( 'NONE', *, *, #24004, .T. ) ;
#14189 = DIRECTION ( 'NONE',  ( 0.000000000000000000, 0.000000000000000000, 1.000000000000000000 ) ) ;
#14190 = CIRCLE ( 'NONE', #47671, 0.06509327318403745899 ) ;
#14191 = EDGE_LOOP ( 'NONE', ( #78000, #123029 ) ) ;
#14192 = ORIENTED_EDGE ( 'NONE', *, *, #22092, .F. ) ;
#14193 = CARTESIAN_POINT ( 'NONE',  ( -0.2000000000000399791, 2.500000000000000000, -4.776537180435977525 ) ) ;
#14194 = AXIS2_PLACEMENT_3D ( 'NONE', #31613, #11320, #122572 ) ;
#14195 = CARTESIAN_POINT ( 'NONE',  ( 1.649999999999950617, 2.500000000000000000, 2.165063509461097713 ) ) ;
#14196 = FACE_OUTER_BOUND ( 'NONE', #10802, .T. ) ;
#14198 = ADVANCED_FACE ( 'NONE', ( #10734 ), #128995, .T. ) ;
#14197 = DIRECTION ( 'NONE',  ( 0.000000000000000000, 1.000000000000000000, 0.000000000000000000 ) ) ;
#14200 = CONICAL_SURFACE ( 'NONE', #62352, 0.09999999999999999167, 0.003490658503988666988 ) ;
#14199 = CARTESIAN_POINT ( 'NONE',  ( -0.6000000000000323963, 2.500000000000000000, -0.4464101615137759382 ) ) ;
#14201 = ORIENTED_EDGE ( 'NONE', *, *, #85223, .F. ) ;
#14202 = AXIS2_PLACEMENT_3D ( 'NONE', #13725, #63492, #112597 ) ;
#14203 = EDGE_LOOP ( 'NONE', ( #86550, #30054, #8122, #52219 ) ) ;
#14204 = DIRECTION ( 'NONE',  ( 0.000000000000000000, 1.000000000000000000, 0.000000000000000000 ) ) ;
#14205 = CIRCLE ( 'NONE', #45533, 0.1000000000000002554 ) ;
#14206 = DIRECTION ( 'NONE',  ( 0.000000000000000000, 0.000000000000000000, -1.000000000000000000 ) ) ;
#14207 = FACE_OUTER_BOUND ( 'NONE', #93588, .T. ) ;
#14208 = ORIENTED_EDGE ( 'NONE', *, *, #38903, .T. ) ;
#14209 = EDGE_LOOP ( 'NONE', ( #21954, #94314, #83194, #109520 ) ) ;
#14210 = DIRECTION ( 'NONE',  ( 0.000000000000000000, 1.000000000000000000, 0.000000000000000000 ) ) ;
#14211 = CIRCLE ( 'NONE', #24700, 0.06509327318403745899 ) ;
#14212 = AXIS2_PLACEMENT_3D ( 'NONE', #7422, #109505, #59791 ) ;
#14213 = VERTEX_POINT ( 'NONE', #92541 ) ;
#14214 = CARTESIAN_POINT ( 'NONE',  ( 179.5000000000000000, -0.6250000000000000000, 7.634788798650553154 ) ) ;
#14215 = DIRECTION ( 'NONE',  ( -1.000000000000000000, -0.000000000000000000, -0.000000000000000000 ) ) ;
#14216 = EDGE_LOOP ( 'NONE', ( #83478, #101961 ) ) ;
#14217 = CARTESIAN_POINT ( 'NONE',  ( -12.69999999999999218, 2.500000000000000000, 4.676537180435972552 ) ) ;
#14218 = CARTESIAN_POINT ( 'NONE',  ( -3.469446951953614189E-14, 12.50000000000000000, -0.6928203230275519209 ) ) ;
#14219 = DIRECTION ( 'NONE',  ( -0.000000000000000000, 1.000000000000000000, -0.000000000000000000 ) ) ;
#14220 = AXIS2_PLACEMENT_3D ( 'NONE', #42023, #64234, #21743 ) ;
#14221 = CARTESIAN_POINT ( 'NONE',  ( -0.6000000000000323963, 12.50000000000000000, -0.3464101615137759604 ) ) ;
#14222 = ORIENTED_EDGE ( 'NONE', *, *, #5113, .T. ) ;
#14223 = EDGE_CURVE ( 'NONE', #21908, #111830, #120652, .T. ) ;
#14224 = FACE_OUTER_BOUND ( 'NONE', #28477, .T. ) ;
#14226 = VECTOR ( 'NONE', #112667, 1000.000000000000000 ) ;
#14225 = CONICAL_SURFACE ( 'NONE', #26763, 0.09999999999999982514, 0.003490658503988666988 ) ;
#14227 = CARTESIAN_POINT ( 'NONE',  ( 26.76314062975269081, -1.072173157150710043, 4.440523076943300396 ) ) ;
#14228 = ORIENTED_EDGE ( 'NONE', *, *, #9429, .F. ) ;
#14229 =( BOUNDED_CURVE ( )  B_SPLINE_CURVE ( 2, ( #60447, #108228, #100354, #68948, #28392, #108860, #18560 ),
 .UNSPECIFIED., .F., .F. ) 
 B_SPLINE_CURVE_WITH_KNOTS ( ( 3, 2, 2, 3 ),
 ( 0.4285714285714289362, 0.4523809523809527722, 0.4761904761904766081, 0.5000000000000004441 ),
 .UNSPECIFIED. ) 
 CURVE ( )  GEOMETRIC_REPRESENTATION_ITEM ( )  RATIONAL_B_SPLINE_CURVE ( ( 0.9999999999999977796, 0.8660254037844409281, 1.000000000000000000, 0.8660254037844387076, 1.000000000000000000, 0.8660254037844361541, 1.000000000000002442 ) ) 
 REPRESENTATION_ITEM ( '' )  );
#14230 = ORIENTED_EDGE ( 'NONE', *, *, #127488, .T. ) ;
#14231 = EDGE_CURVE ( 'NONE', #47341, #41439, #80807, .T. ) ;
#14232 = CARTESIAN_POINT ( 'NONE',  ( 184.9427083336747160, -6.551208109652278289, 3.782341765624995134 ) ) ;
#14233 = DIRECTION ( 'NONE',  ( 0.000000000000000000, 0.000000000000000000, 1.000000000000000000 ) ) ;
#14234 = FACE_OUTER_BOUND ( 'NONE', #106693, .T. ) ;
#14235 = ADVANCED_FACE ( 'NONE', ( #120719 ), #63086, .T. ) ;
#14236 = DIRECTION ( 'NONE',  ( 0.000000000000000000, 0.000000000000000000, 1.000000000000000000 ) ) ;
#14237 = FACE_OUTER_BOUND ( 'NONE', #10479, .T. ) ;
#14238 = CARTESIAN_POINT ( 'NONE',  ( -0.6000000000000388356, 2.500000000000000000, 4.576537180435972019 ) ) ;
#14239 = DIRECTION ( 'NONE',  ( 0.000000000000000000, 1.000000000000000000, 0.000000000000000000 ) ) ;
#14240 = DIRECTION ( 'NONE',  ( 0.000000000000000000, 0.000000000000000000, 1.000000000000000000 ) ) ;
#14241 = CARTESIAN_POINT ( 'NONE',  ( 4.799999999999939426, 2.500000000000000000, -4.776537180435977525 ) ) ;
#14242 = DIRECTION ( 'NONE',  ( 0.000000000000000000, -0.9999939076577903929, 0.003490651415223739937 ) ) ;
#14243 = EDGE_CURVE ( 'NONE', #108419, #84285, #31702, .T. ) ;
#14244 = ADVANCED_FACE ( 'NONE', ( #51992 ), #64202, .T. ) ;
#14245 = EDGE_CURVE ( 'NONE', #1262, #111853, #49558, .T. ) ;
#14246 = LINE ( 'NONE', #83020, #12476 ) ;
#14247 = VERTEX_POINT ( 'NONE', #123296 ) ;
#14248 = ORIENTED_EDGE ( 'NONE', *, *, #53884, .F. ) ;
#14249 = EDGE_CURVE ( 'NONE', #2581, #107840, #45359, .T. ) ;
#14250 = EDGE_LOOP ( 'NONE', ( #14464, #27483 ) ) ;
#14251 = CIRCLE ( 'NONE', #24732, 0.1000000000000002554 ) ;
#14252 = VECTOR ( 'NONE', #115598, 1000.000000000000000 ) ;
#14253 = EDGE_LOOP ( 'NONE', ( #3330, #75026 ) ) ;
#14254 = EDGE_CURVE ( 'NONE', #85684, #17230, #122707, .T. ) ;
#14255 = DIRECTION ( 'NONE',  ( -0.000000000000000000, -1.000000000000000000, -0.000000000000000000 ) ) ;
#14256 = CARTESIAN_POINT ( 'NONE',  ( -4.400000000000028777, 2.500000000000000000, -4.776537180435978414 ) ) ;
#14257 = ADVANCED_FACE ( 'NONE', ( #106237 ), #34293, .T. ) ;
#14258 = ORIENTED_EDGE ( 'NONE', *, *, #51331, .F. ) ;
#14259 = CONICAL_SURFACE ( 'NONE', #118825, 0.1000000000000002554, 0.003490658503988666988 ) ;
#14260 = CARTESIAN_POINT ( 'NONE',  ( 1.049999999999954525, 2.500000000000000000, -2.511473670974877948 ) ) ;
#14261 = AXIS2_PLACEMENT_3D ( 'NONE', #36027, #74657, #15725 ) ;
#14262 = CARTESIAN_POINT ( 'NONE',  ( -4.350000000000023626, 12.50000000000000000, 2.446380397790835826 ) ) ;
#14264 = EDGE_LOOP ( 'NONE', ( #124137, #24173, #116378, #44428 ) ) ;
#14263 = CARTESIAN_POINT ( 'NONE',  ( 184.5000000000000000, -2.986254062820097310, -7.097343634930640022 ) ) ;
#14265 = CARTESIAN_POINT ( 'NONE',  ( 13.74999999999989697, 12.50000000000000000, 2.857883832488649301 ) ) ;
#14266 = VECTOR ( 'NONE', #46336, 1000.000000000000000 ) ;
#14267 = CARTESIAN_POINT ( 'NONE',  ( 2.699999999999944666, 2.500000000000000000, 4.776537180435972196 ) ) ;
#14268 = EDGE_LOOP ( 'NONE', ( #53727, #1840, #38894, #46116 ) ) ;
#14269 = AXIS2_PLACEMENT_3D ( 'NONE', #123708, #91051, #62886 ) ;
#14270 = VERTEX_POINT ( 'NONE', #14608 ) ;
#14271 = ORIENTED_EDGE ( 'NONE', *, *, #86744, .F. ) ;
#14272 = EDGE_LOOP ( 'NONE', ( #28358, #41243, #38757, #52642 ) ) ;
#14273 = CARTESIAN_POINT ( 'NONE',  ( -10.40000000000000213, 2.500000000000000000, -4.330127018922197202 ) ) ;
#14274 = CARTESIAN_POINT ( 'NONE',  ( 3.099999999999945466, 2.500000000000000000, -4.083716857408426826 ) ) ;
#14275 = CARTESIAN_POINT ( 'NONE',  ( 15.19999999999989093, 2.500000000000000000, 0.3464101615137735735 ) ) ;
#14276 = LINE ( 'NONE', #54222, #114675 ) ;
#14277 = VECTOR ( 'NONE', #30145, 1000.000000000000000 ) ;
#14278 = EDGE_LOOP ( 'NONE', ( #22363, #96196, #63227, #31646 ) ) ;
#14279 = CARTESIAN_POINT ( 'NONE',  ( 12.29999999999990656, 2.500000000000000000, -4.676537180435977881 ) ) ;
#14280 = ORIENTED_EDGE ( 'NONE', *, *, #70683, .F. ) ;
#14281 = VECTOR ( 'NONE', #21178, 1000.000000000000000 ) ;
#14282 = DIRECTION ( 'NONE',  ( 0.000000000000000000, -0.9999939076577903929, 0.003490651415223739937 ) ) ;
#14283 = FACE_OUTER_BOUND ( 'NONE', #29084, .T. ) ;
#14284 = CARTESIAN_POINT ( 'NONE',  ( 4.599999999999939249, 2.500000000000000000, -3.637306695894650055 ) ) ;
#14285 = CARTESIAN_POINT ( 'NONE',  ( 6.699999999999930012, 2.500000000000000000, -4.430127018922202176 ) ) ;
#14286 = ORIENTED_EDGE ( 'NONE', *, *, #127988, .F. ) ;
#14287 = CIRCLE ( 'NONE', #112513, 0.1000000000000002554 ) ;
#14288 = EDGE_CURVE ( 'NONE', #95225, #88750, #116428, .T. ) ;
#14289 = VERTEX_POINT ( 'NONE', #63741 ) ;
#14290 = ORIENTED_EDGE ( 'NONE', *, *, #69105, .T. ) ;
#14291 = CARTESIAN_POINT ( 'NONE',  ( -1.250000000000036193, 12.50000000000000000, 1.537336459617582918 ) ) ;
#14292 = CARTESIAN_POINT ( 'NONE',  ( -6.050000000000020250, 12.50000000000000000, -2.446380397790840266 ) ) ;
#14293 = CARTESIAN_POINT ( 'NONE',  ( -4.400000000000028777, 2.500000000000000000, -3.983716857408426293 ) ) ;
#14294 = FACE_BOUND ( 'NONE', #108517, .T. ) ;
#14295 = DIRECTION ( 'NONE',  ( 0.000000000000000000, 1.000000000000000000, 0.000000000000000000 ) ) ;
#14296 = LINE ( 'NONE', #53605, #40249 ) ;
#14297 = DIRECTION ( 'NONE',  ( 0.000000000000000000, -0.9999939076577903929, 0.003490651415223739937 ) ) ;
#14298 = EDGE_CURVE ( 'NONE', #88991, #102186, #18234, .T. ) ;
#14299 = AXIS2_PLACEMENT_3D ( 'NONE', #91080, #1405, #121184 ) ;
#14300 = CARTESIAN_POINT ( 'NONE',  ( 186.8385416670080872, 6.551208109652274736, 3.782341765625001351 ) ) ;
#14301 = CARTESIAN_POINT ( 'NONE',  ( 3.349999999999944578, 12.50000000000000000, -5.867463478539787225 ) ) ;
#14302 = CONICAL_SURFACE ( 'NONE', #87464, 0.09999999999999982514, 0.003490658503988666988 ) ;
#14303 = DIRECTION ( 'NONE',  ( 0.000000000000000000, 0.000000000000000000, 1.000000000000000000 ) ) ;
#14304 = EDGE_LOOP ( 'NONE', ( #3603, #105185, #36368, #124928 ) ) ;
#14305 = DIRECTION ( 'NONE',  ( -0.000000000000000000, -1.000000000000000000, -0.000000000000000000 ) ) ;
#14306 = ORIENTED_EDGE ( 'NONE', *, *, #65959, .F. ) ;
#14307 = ORIENTED_EDGE ( 'NONE', *, *, #78669, .T. ) ;
#14308 = ORIENTED_EDGE ( 'NONE', *, *, #26067, .T. ) ;
#14309 = VERTEX_POINT ( 'NONE', #25093 ) ;
#14310 = CONICAL_SURFACE ( 'NONE', #72913, 0.09999999999999982514, 0.003490658503988666988 ) ;
#14311 = CARTESIAN_POINT ( 'NONE',  ( 1.049999999999952083, 2.500000000000000000, 6.841600689897072485 ) ) ;
#14312 = FACE_BOUND ( 'NONE', #98129, .T. ) ;
#14313 = DIRECTION ( 'NONE',  ( -0.000000000000000000, 1.000000000000000000, -0.000000000000000000 ) ) ;
#14315 = CIRCLE ( 'NONE', #125154, 0.06509327318403745899 ) ;
#14314 = AXIS2_PLACEMENT_3D ( 'NONE', #53949, #64403, #124621 ) ;
#14316 = ORIENTED_EDGE ( 'NONE', *, *, #62439, .T. ) ;
#14317 = DIRECTION ( 'NONE',  ( 0.000000000000000000, 1.000000000000000000, 0.000000000000000000 ) ) ;
#14318 = DIRECTION ( 'NONE',  ( 0.000000000000000000, 0.000000000000000000, -1.000000000000000000 ) ) ;
#14319 = ORIENTED_EDGE ( 'NONE', *, *, #53415, .T. ) ;
#14320 = CARTESIAN_POINT ( 'NONE',  ( -5.000000000000023093, 2.500000000000000000, 0.6928203230275494784 ) ) ;
#14321 = DIRECTION ( 'NONE',  ( 0.000000000000000000, 1.000000000000000000, 0.000000000000000000 ) ) ;
#14322 = EDGE_CURVE ( 'NONE', #68325, #18847, #51702, .T. ) ;
#14323 = ORIENTED_EDGE ( 'NONE', *, *, #90524, .F. ) ;
#14324 = AXIS2_PLACEMENT_3D ( 'NONE', #65355, #2558, #13680 ) ;
#14325 = DIRECTION ( 'NONE',  ( 0.000000000000000000, -0.000000000000000000, 1.000000000000000000 ) ) ;
#14326 = DIRECTION ( 'NONE',  ( 0.000000000000000000, 1.000000000000000000, 0.000000000000000000 ) ) ;
#14327 = ADVANCED_FACE ( 'NONE', ( #94466 ), #44749, .T. ) ;
#14328 = ORIENTED_EDGE ( 'NONE', *, *, #77498, .T. ) ;
#14329 = AXIS2_PLACEMENT_3D ( 'NONE', #100870, #87823, #127764 ) ;
#14330 = CARTESIAN_POINT ( 'NONE',  ( 10.44999999999991047, 2.500000000000000000, -6.495190528383302464 ) ) ;
#14331 = CIRCLE ( 'NONE', #127239, 0.06509327318403745899 ) ;
#14332 = CARTESIAN_POINT ( 'NONE',  ( -7.100000000000013856, 2.500000000000000000, 3.537306695894645081 ) ) ;
#14333 = CIRCLE ( 'NONE', #1828, 0.06509327318403745899 ) ;
#14334 = DIRECTION ( 'NONE',  ( 0.000000000000000000, 0.000000000000000000, 1.000000000000000000 ) ) ;
#14335 = EDGE_LOOP ( 'NONE', ( #112103, #29750 ) ) ;
#14336 = EDGE_CURVE ( 'NONE', #103569, #116451, #60030, .T. ) ;
#14337 = ORIENTED_EDGE ( 'NONE', *, *, #5394, .F. ) ;
#14338 = EDGE_CURVE ( 'NONE', #104652, #118880, #55807, .T. ) ;
#14339 = LINE ( 'NONE', #54283, #72364 ) ;
#14341 = VERTEX_POINT ( 'NONE', #44089 ) ;
#14340 = AXIS2_PLACEMENT_3D ( 'NONE', #115276, #98239, #125750 ) ;
#14342 = DIRECTION ( 'NONE',  ( -0.000000000000000000, 1.000000000000000000, -0.000000000000000000 ) ) ;
#14343 = CARTESIAN_POINT ( 'NONE',  ( -13.94999999999998685, 2.500000000000000000, -2.511473670974875727 ) ) ;
#14344 = VECTOR ( 'NONE', #84420, 1000.000000000000000 ) ;
#14345 = EDGE_LOOP ( 'NONE', ( #64424, #24627 ) ) ;
#14346 = EDGE_CURVE ( 'NONE', #41508, #22099, #7767, .T. ) ;
#14347 = CONICAL_SURFACE ( 'NONE', #104253, 0.09999999999999982514, 0.003490658503988666988 ) ;
#14348 = DIRECTION ( 'NONE',  ( 0.000000000000000000, 0.000000000000000000, -1.000000000000000000 ) ) ;
#14349 = DIRECTION ( 'NONE',  ( 0.000000000000000000, 0.000000000000000000, 1.000000000000000000 ) ) ;
#14350 = CARTESIAN_POINT ( 'NONE',  ( 7.499999999999925393, 2.500000000000000000, -0.5928203230275541635 ) ) ;
#14351 = DIRECTION ( 'NONE',  ( 0.000000000000000000, 0.000000000000000000, 1.000000000000000000 ) ) ;
#14352 = EDGE_CURVE ( 'NONE', #25279, #102784, #112247, .T. ) ;
#14353 = CARTESIAN_POINT ( 'NONE',  ( -10.60000000000000142, 2.500000000000000000, 4.083716857408421497 ) ) ;
#14354 = CIRCLE ( 'NONE', #108448, 0.1000000000000002554 ) ;
#14355 = ORIENTED_EDGE ( 'NONE', *, *, #55964, .F. ) ;
#14356 = VERTEX_POINT ( 'NONE', #75474 ) ;
#14357 = CARTESIAN_POINT ( 'NONE',  ( 4.149999999999941735, 2.500000000000000000, -5.702370205355749455 ) ) ;
#14358 = CARTESIAN_POINT ( 'NONE',  ( -0.8500000000000386136, 12.50000000000000000, 5.802370205355744659 ) ) ;
#14359 = DIRECTION ( 'NONE',  ( 0.000000000000000000, 1.000000000000000000, 0.000000000000000000 ) ) ;
#14361 = ORIENTED_EDGE ( 'NONE', *, *, #10557, .T. ) ;
#14360 = ORIENTED_EDGE ( 'NONE', *, *, #66115, .T. ) ;
#14362 = ORIENTED_EDGE ( 'NONE', *, *, #11073, .F. ) ;
#14363 = DIRECTION ( 'NONE',  ( 0.000000000000000000, 0.000000000000000000, 1.000000000000000000 ) ) ;
#14365 = CARTESIAN_POINT ( 'NONE',  ( -3.643930204294122679E-14, 12.50000000000000000, 0.6277270498435143509 ) ) ;
#14364 = VECTOR ( 'NONE', #49634, 1000.000000000000000 ) ;
#14366 = DIRECTION ( 'NONE',  ( -0.000000000000000000, -1.000000000000000000, -0.000000000000000000 ) ) ;
#14367 = FILL_AREA_STYLE_COLOUR ( '', #49923 ) ;
#14368 = CARTESIAN_POINT ( 'NONE',  ( 11.04999999999991189, 2.500000000000000000, -2.611473670974877592 ) ) ;
#14369 = CARTESIAN_POINT ( 'NONE',  ( 9.599999999999914380, 2.500000000000000000, -5.022947341949754119 ) ) ;
#14370 = LINE ( 'NONE', #22931, #38200 ) ;
#14371 = CARTESIAN_POINT ( 'NONE',  ( 11.84999999999990372, 12.50000000000000000, 2.511473670974873507 ) ) ;
#14372 = AXIS2_PLACEMENT_3D ( 'NONE', #114392, #126805, #37143 ) ;
#14373 = CARTESIAN_POINT ( 'NONE',  ( -11.24999999999999822, 2.500000000000000000, 5.702370205355745014 ) ) ;
#14374 = DIRECTION ( 'NONE',  ( 0.000000000000000000, 0.000000000000000000, 1.000000000000000000 ) ) ;
#14375 = ORIENTED_EDGE ( 'NONE', *, *, #99412, .T. ) ;
#14376 = EDGE_CURVE ( 'NONE', #78982, #24357, #89256, .T. ) ;
#14377 = VECTOR ( 'NONE', #12147, 1000.000000000000000 ) ;
#14378 = DIRECTION ( 'NONE',  ( -0.000000000000000000, -1.000000000000000000, -0.000000000000000000 ) ) ;
#14379 = ORIENTED_EDGE ( 'NONE', *, *, #54875, .T. ) ;
#14380 = EDGE_LOOP ( 'NONE', ( #71649, #115904 ) ) ;
#14381 = EDGE_CURVE ( 'NONE', #6322, #36965, #22374, .T. ) ;
#14382 = DIRECTION ( 'NONE',  ( 0.000000000000000000, 0.000000000000000000, -1.000000000000000000 ) ) ;
#14383 = DIRECTION ( 'NONE',  ( 0.000000000000000000, 1.000000000000000000, 0.000000000000000000 ) ) ;
#14384 = AXIS2_PLACEMENT_3D ( 'NONE', #40827, #89895, #98412 ) ;
#14385 = CARTESIAN_POINT ( 'NONE',  ( -2.100000000000034284, 2.500000000000000000, 0.09999999999999761857 ) ) ;
#14386 = EDGE_CURVE ( 'NONE', #50878, #74924, #126526, .T. ) ;
#14388 = AXIS2_PLACEMENT_3D ( 'NONE', #14434, #4597, #36032 ) ;
#14387 = CARTESIAN_POINT ( 'NONE',  ( 1.649999999999951950, 12.50000000000000000, -7.122917578226816815 ) ) ;
#14389 = DIRECTION ( 'NONE',  ( 0.000000000000000000, 0.000000000000000000, 1.000000000000000000 ) ) ;
#14390 = FACE_OUTER_BOUND ( 'NONE', #18638, .T. ) ;
#14391 = CARTESIAN_POINT ( 'NONE',  ( 11.84999999999990372, 12.50000000000000000, 1.818653347947321475 ) ) ;
#14392 = ORIENTED_EDGE ( 'NONE', *, *, #89579, .F. ) ;
#14393 = CARTESIAN_POINT ( 'NONE',  ( -4.550000000000022915, 12.50000000000000000, -2.099970236277064473 ) ) ;
#14394 = ADVANCED_FACE ( 'NONE', ( #25732 ), #3574, .T. ) ;
#14395 = AXIS2_PLACEMENT_3D ( 'NONE', #60597, #40963, #71682 ) ;
#14396 = ADVANCED_FACE ( 'NONE', ( #124592 ), #105602, .T. ) ;
#14397 = EDGE_CURVE ( 'NONE', #118850, #50117, #2370, .T. ) ;
#14398 = LINE ( 'NONE', #104711, #72938 ) ;
#14399 = VERTEX_POINT ( 'NONE', #13970 ) ;
#14400 = ORIENTED_EDGE ( 'NONE', *, *, #25909, .T. ) ;
#14401 = EDGE_CURVE ( 'NONE', #88713, #2945, #47496, .T. ) ;
#14402 = VERTEX_POINT ( 'NONE', #98991 ) ;
#14403 = AXIS2_PLACEMENT_3D ( 'NONE', #129317, #52028, #121398 ) ;
#14404 = VERTEX_POINT ( 'NONE', #9968 ) ;
#14405 = CARTESIAN_POINT ( 'NONE',  ( 10.39999999999991154, 2.500000000000000000, 3.537306695894645081 ) ) ;
#14406 = CARTESIAN_POINT ( 'NONE',  ( 10.39999999999991154, 2.500000000000000000, -5.022947341949754119 ) ) ;
#14407 = EDGE_CURVE ( 'NONE', #48905, #38438, #87185, .T. ) ;
#14410 = EDGE_CURVE ( 'NONE', #120005, #16509, #76738, .T. ) ;
#14409 = CONICAL_SURFACE ( 'NONE', #87573, 0.09999999999999982514, 0.003490658503988666988 ) ;
#14408 = CONICAL_SURFACE ( 'NONE', #29116, 0.1000000000000000056, 0.003490658503988666988 ) ;
#14411 = CARTESIAN_POINT ( 'NONE',  ( -3.550000000000028244, 12.50000000000000000, 2.511473670974873507 ) ) ;
#14412 = CARTESIAN_POINT ( 'NONE',  ( 8.349999999999923261, 12.50000000000000000, 2.230156782645134950 ) ) ;
#14413 = DIRECTION ( 'NONE',  ( 0.000000000000000000, -0.000000000000000000, 1.000000000000000000 ) ) ;
#14414 = ORIENTED_EDGE ( 'NONE', *, *, #100341, .F. ) ;
#14415 = CARTESIAN_POINT ( 'NONE',  ( -6.450000000000017941, 2.500000000000000000, -6.741600689897077281 ) ) ;
#14416 = CARTESIAN_POINT ( 'NONE',  ( 2.299999999999946976, 12.50000000000000000, 4.611443907251934426 ) ) ;
#14417 = CARTESIAN_POINT ( 'NONE',  ( -1.900000000000034994, 12.50000000000000000, -0.3464101615137783474 ) ) ;
#14418 = ORIENTED_EDGE ( 'NONE', *, *, #76219, .F. ) ;
#14419 = ORIENTED_EDGE ( 'NONE', *, *, #66682, .T. ) ;
#14420 = ORIENTED_EDGE ( 'NONE', *, *, #215, .T. ) ;
#14421 = AXIS2_PLACEMENT_3D ( 'NONE', #122058, #72315, #11443 ) ;
#14422 = CARTESIAN_POINT ( 'NONE',  ( 2.299999999999946976, 2.500000000000000000, 4.676537180435972552 ) ) ;
#14423 = CARTESIAN_POINT ( 'NONE',  ( 11.89999999999990443, 2.500000000000000000, -0.2464101615137782308 ) ) ;
#14424 = CARTESIAN_POINT ( 'NONE',  ( -11.05000000000000249, 2.500000000000000000, -6.048780366869523029 ) ) ;
#14425 = AXIS2_PLACEMENT_3D ( 'NONE', #14417, #96848, #85101 ) ;
#14426 = CIRCLE ( 'NONE', #108532, 0.09999999999999982514 ) ;
#14427 = ORIENTED_EDGE ( 'NONE', *, *, #48484, .F. ) ;
#14428 = DIRECTION ( 'NONE',  ( 0.000000000000000000, 0.000000000000000000, 1.000000000000000000 ) ) ;
#14429 = CARTESIAN_POINT ( 'NONE',  ( -12.69999999999999218, 2.500000000000000000, -0.2464101615137741230 ) ) ;
#14430 = DIRECTION ( 'NONE',  ( 0.000000000000000000, 0.000000000000000000, 1.000000000000000000 ) ) ;
#14431 = CARTESIAN_POINT ( 'NONE',  ( 9.599999999999914380, 12.50000000000000000, 5.088040615133786027 ) ) ;
#14432 = AXIS2_PLACEMENT_3D ( 'NONE', #105713, #95889, #46138 ) ;
#14433 = CIRCLE ( 'NONE', #93880, 0.1000000000000002554 ) ;
#14434 = CARTESIAN_POINT ( 'NONE',  ( -9.800000000000006040, 2.500000000000000000, 4.676537180435972552 ) ) ;
#14435 = EDGE_CURVE ( 'NONE', #123378, #52442, #108156, .T. ) ;
#14436 = EDGE_LOOP ( 'NONE', ( #71460, #95093 ) ) ;
#14437 = EDGE_LOOP ( 'NONE', ( #23274, #109808 ) ) ;
#14438 = CARTESIAN_POINT ( 'NONE',  ( -9.800000000000007816, 2.500000000000000000, -4.083716857408422385 ) ) ;
#14439 = DIRECTION ( 'NONE',  ( 0.000000000000000000, 0.000000000000000000, 1.000000000000000000 ) ) ;
#14440 = AXIS2_PLACEMENT_3D ( 'NONE', #88525, #117312, #125869 ) ;
#14441 = DIRECTION ( 'NONE',  ( 0.000000000000000000, 0.000000000000000000, -1.000000000000000000 ) ) ;
#14442 = CARTESIAN_POINT ( 'NONE',  ( 11.24999999999990941, 12.50000000000000000, -1.472243186433550122 ) ) ;
#14443 = CARTESIAN_POINT ( 'NONE',  ( -6.900000000000015454, 2.500000000000000000, 4.576537180435972019 ) ) ;
#14444 = EDGE_CURVE ( 'NONE', #2289, #27095, #48608, .T. ) ;
#14445 = VECTOR ( 'NONE', #44368, 1000.000000000000000 ) ;
#14446 = VERTEX_POINT ( 'NONE', #27034 ) ;
#14447 = VERTEX_POINT ( 'NONE', #47972 ) ;
#14448 = CARTESIAN_POINT ( 'NONE',  ( 9.349999999999916156, 2.500000000000000000, -1.818653347947326138 ) ) ;
#14449 = DIRECTION ( 'NONE',  ( 0.000000000000000000, 0.000000000000000000, -1.000000000000000000 ) ) ;
#14450 = LINE ( 'NONE', #70976, #19376 ) ;
#14451 = DIRECTION ( 'NONE',  ( 0.000000000000000000, 0.000000000000000000, -1.000000000000000000 ) ) ;
#14452 = ORIENTED_EDGE ( 'NONE', *, *, #15132, .F. ) ;
#14453 = CARTESIAN_POINT ( 'NONE',  ( -0.4000000000000404898, 2.500000000000000000, 4.922947341949748257 ) ) ;
#14454 = DIRECTION ( 'NONE',  ( 0.000000000000000000, 0.000000000000000000, -1.000000000000000000 ) ) ;
#14455 = AXIS2_PLACEMENT_3D ( 'NONE', #401, #128092, #69151 ) ;
#14456 = ORIENTED_EDGE ( 'NONE', *, *, #120957, .T. ) ;
#14457 = DIRECTION ( 'NONE',  ( -0.000000000000000000, -1.000000000000000000, -0.000000000000000000 ) ) ;
#14458 =( BOUNDED_SURFACE ( )  B_SPLINE_SURFACE ( 2, 3, ( 
 ( #11515, #61272, #1683, #2994 ),
 ( #101834, #122129, #42944, #110983 ),
 ( #80909, #111659, #101192, #62569 ),
 ( #123395, #82856, #82197, #41653 ),
 ( #121456, #22644, #1048, #52096 ) ),
 .UNSPECIFIED., .F., .F., .F. ) 
 B_SPLINE_SURFACE_WITH_KNOTS ( ( 3, 2, 3 ),
 ( 4, 4 ),
 ( -0.1337713181301400378, 0.000000000000000000, 1.000000000000000000 ),
 ( -0.0002500000000000000052, 0.005250000000000000326 ),
 .UNSPECIFIED. ) 
 GEOMETRIC_REPRESENTATION_ITEM ( )  RATIONAL_B_SPLINE_SURFACE ( (
 ( 1.000000000000000000, 1.000000000000000000, 1.000000000000000000, 1.000000000000000000),
 ( 1.000000000000000000, 1.000000000000000000, 1.000000000000000000, 1.000000000000000000),
 ( 1.000000000000000000, 1.000000000000000000, 1.000000000000000000, 1.000000000000000000),
 ( 0.7071067811865475727, 0.7071067811865475727, 0.7071067811865475727, 0.7071067811865475727),
 ( 1.000000000000000000, 1.000000000000000000, 1.000000000000000000, 1.000000000000000000) ) ) 
 REPRESENTATION_ITEM ( '' )  SURFACE ( )  );
#14459 = EDGE_LOOP ( 'NONE', ( #92361, #92682 ) ) ;
#14460 = DIRECTION ( 'NONE',  ( 0.000000000000000000, -0.000000000000000000, 1.000000000000000000 ) ) ;
#14461 = ORIENTED_EDGE ( 'NONE', *, *, #83070, .F. ) ;
#14462 = DIRECTION ( 'NONE',  ( 0.000000000000000000, 0.000000000000000000, 1.000000000000000000 ) ) ;
#14463 = DIRECTION ( 'NONE',  ( -0.000000000000000000, -1.000000000000000000, -0.000000000000000000 ) ) ;
#14464 = ORIENTED_EDGE ( 'NONE', *, *, #60258, .T. ) ;
#14465 = ORIENTED_EDGE ( 'NONE', *, *, #123776, .F. ) ;
#14466 = CARTESIAN_POINT ( 'NONE',  ( 185.5052083336747444, -6.551208109652278289, 3.782341765624995134 ) ) ;
#14467 = CARTESIAN_POINT ( 'NONE',  ( 133.2169897921533845, 0.5000000000000000000, -0.01898911740318533561 ) ) ;
#14468 = AXIS2_PLACEMENT_3D ( 'NONE', #53213, #64301, #44032 ) ;
#14469 = CARTESIAN_POINT ( 'NONE',  ( 185.3385416670080872, 6.551208109652274736, 3.782341765625001351 ) ) ;
#14470 = DIRECTION ( 'NONE',  ( 0.000000000000000000, 0.000000000000000000, -1.000000000000000000 ) ) ;
#14471 = CARTESIAN_POINT ( 'NONE',  ( 8.549999999999918998, 2.500000000000000000, 6.941600689897073018 ) ) ;
#14472 = CARTESIAN_POINT ( 'NONE',  ( 1.449999999999952216, 2.500000000000000000, 1.818653347947321475 ) ) ;
#14473 = CARTESIAN_POINT ( 'NONE',  ( 5.399999999999934630, 2.500000000000000000, -0.6928203230275542523 ) ) ;
#14474 = DIRECTION ( 'NONE',  ( -0.000000000000000000, -1.000000000000000000, -0.000000000000000000 ) ) ;
#14475 = AXIS2_PLACEMENT_3D ( 'NONE', #51270, #70247, #110175 ) ;
#14476 = ADVANCED_FACE ( 'NONE', ( #128473 ), #27650, .T. ) ;
#14477 = EDGE_LOOP ( 'NONE', ( #13243, #68914 ) ) ;
#14478 = EDGE_LOOP ( 'NONE', ( #98235, #33496, #89148, #6517 ) ) ;
#14479 = DIRECTION ( 'NONE',  ( -0.000000000000000000, -1.000000000000000000, -0.000000000000000000 ) ) ;
#14481 = CONICAL_SURFACE ( 'NONE', #47970, 0.1000000000000002554, 0.003490658503988666988 ) ;
#14480 = AXIS2_PLACEMENT_3D ( 'NONE', #109063, #128095, #7656 ) ;
#14482 = DIRECTION ( 'NONE',  ( 0.000000000000000000, 0.000000000000000000, -1.000000000000000000 ) ) ;
#14483 = CARTESIAN_POINT ( 'NONE',  ( -14.79999999999998472, 12.50000000000000000, 0.3464101615137758494 ) ) ;
#14484 = DIRECTION ( 'NONE',  ( 0.000000000000000000, 0.000000000000000000, -1.000000000000000000 ) ) ;
#14485 = CIRCLE ( 'NONE', #1985, 0.06509327318403745899 ) ;
#14487 = ORIENTED_EDGE ( 'NONE', *, *, #126855, .T. ) ;
#14486 = ORIENTED_EDGE ( 'NONE', *, *, #67206, .T. ) ;
#14488 = EDGE_CURVE ( 'NONE', #40728, #124471, #74676, .T. ) ;
#14489 = FACE_BOUND ( 'NONE', #72417, .T. ) ;
#14490 = ORIENTED_EDGE ( 'NONE', *, *, #64077, .F. ) ;
#14491 = ADVANCED_FACE ( 'NONE', ( #117978 ), #62083, .T. ) ;
#14492 = FACE_OUTER_BOUND ( 'NONE', #123804, .T. ) ;
#14493 = DIRECTION ( 'NONE',  ( 0.000000000000000000, -0.000000000000000000, 1.000000000000000000 ) ) ;
#14494 = EDGE_LOOP ( 'NONE', ( #68779, #88285, #114812, #43315 ) ) ;
#14495 = DIRECTION ( 'NONE',  ( 0.000000000000000000, 1.000000000000000000, 0.000000000000000000 ) ) ;
#14498 = CARTESIAN_POINT ( 'NONE',  ( -7.900000000000014566, 2.500000000000000000, -5.122947341949753763 ) ) ;
#14497 = CIRCLE ( 'NONE', #62652, 0.06509327318403745899 ) ;
#14496 = VECTOR ( 'NONE', #100536, 1000.000000000000000 ) ;
#14499 = PLANE ( 'NONE',  #47259 ) ;
#14500 = DIRECTION ( 'NONE',  ( -0.000000000000000000, -1.000000000000000000, -0.000000000000000000 ) ) ;
#14501 = EDGE_CURVE ( 'NONE', #63883, #24530, #49267, .T. ) ;
#14502 = CARTESIAN_POINT ( 'NONE',  ( 1.249999999999954259, 12.50000000000000000, -7.122917578226816815 ) ) ;
#14503 = ADVANCED_FACE ( 'NONE', ( #107524 ), #127181, .T. ) ;
#14504 = DIRECTION ( 'NONE',  ( 0.000000000000000000, 0.000000000000000000, 1.000000000000000000 ) ) ;
#14505 = CARTESIAN_POINT ( 'NONE',  ( 185.9427083336747160, -6.551208109652278289, 3.782341765624995134 ) ) ;
#14506 = DIRECTION ( 'NONE',  ( 0.000000000000000000, -0.000000000000000000, 1.000000000000000000 ) ) ;
#14507 = EDGE_CURVE ( 'NONE', #41590, #2959, #118488, .T. ) ;
#14508 = DIRECTION ( 'NONE',  ( 0.000000000000000000, 0.000000000000000000, 1.000000000000000000 ) ) ;
#14509 = VERTEX_POINT ( 'NONE', #128 ) ;
#14510 = ORIENTED_EDGE ( 'NONE', *, *, #62119, .F. ) ;
#14511 = EDGE_LOOP ( 'NONE', ( #29037, #7273 ) ) ;
#14512 = LINE ( 'NONE', #85835, #70072 ) ;
#14513 = VERTEX_POINT ( 'NONE', #89173 ) ;
#14514 = DIRECTION ( 'NONE',  ( 0.000000000000000000, 0.000000000000000000, 1.000000000000000000 ) ) ;
#14515 = AXIS2_PLACEMENT_3D ( 'NONE', #84695, #116087, #74883 ) ;
#14517 = EDGE_LOOP ( 'NONE', ( #69099, #82975 ) ) ;
#14516 = ORIENTED_EDGE ( 'NONE', *, *, #120229, .T. ) ;
#14518 = EDGE_LOOP ( 'NONE', ( #89468, #16055, #27398, #84579 ) ) ;
#14519 = CARTESIAN_POINT ( 'NONE',  ( -9.600000000000008527, 12.50000000000000000, -2.385244779468109755E-15 ) ) ;
#14520 = CIRCLE ( 'NONE', #43802, 0.06509327318403745899 ) ;
#14521 = AXIS2_PLACEMENT_3D ( 'NONE', #55481, #14869, #75748 ) ;
#14522 = DIRECTION ( 'NONE',  ( 0.000000000000000000, 0.000000000000000000, 1.000000000000000000 ) ) ;
#14523 = DIRECTION ( 'NONE',  ( 0.000000000000000000, 0.000000000000000000, 1.000000000000000000 ) ) ;
#14524 = CARTESIAN_POINT ( 'NONE',  ( 185.3645833340161175, -6.668395609140180369, 3.849999999999994760 ) ) ;
#14525 = CARTESIAN_POINT ( 'NONE',  ( -9.600000000000006750, 12.50000000000000000, 3.572213422710607489 ) ) ;
#14526 = ORIENTED_EDGE ( 'NONE', *, *, #110001, .F. ) ;
#14527 = CONICAL_SURFACE ( 'NONE', #125269, 0.09999999999999982514, 0.003490658503988666988 ) ;
#14530 = AXIS2_PLACEMENT_3D ( 'NONE', #115965, #36780, #16456 ) ;
#14529 = LINE ( 'NONE', #54466, #104067 ) ;
#14528 = CIRCLE ( 'NONE', #58390, 0.1000000000000000056 ) ;
#14531 = EDGE_LOOP ( 'NONE', ( #72387, #101579, #9771, #36133 ) ) ;
#14532 = AXIS2_PLACEMENT_3D ( 'NONE', #86329, #124343, #105344 ) ;
#14533 = ORIENTED_EDGE ( 'NONE', *, *, #117521, .T. ) ;
#14534 = EDGE_LOOP ( 'NONE', ( #56775, #100350, #4082, #12638 ) ) ;
#14535 = CARTESIAN_POINT ( 'NONE',  ( -5.000000000000026645, 2.500000000000000000, -3.637306695894650055 ) ) ;
#14536 = VERTEX_POINT ( 'NONE', #106858 ) ;
#14537 = VERTEX_POINT ( 'NONE', #28975 ) ;
#14538 = ORIENTED_EDGE ( 'NONE', *, *, #64835, .F. ) ;
#14539 = VECTOR ( 'NONE', #106868, 1000.000000000000000 ) ;
#14540 = DIRECTION ( 'NONE',  ( 0.000000000000000000, 0.000000000000000000, -1.000000000000000000 ) ) ;
#14541 = VECTOR ( 'NONE', #27782, 1000.000000000000000 ) ;
#14542 = DIRECTION ( 'NONE',  ( -0.000000000000000000, 1.000000000000000000, -0.000000000000000000 ) ) ;
#14543 = CARTESIAN_POINT ( 'NONE',  ( 2.299999999999947864, 2.500000000000000000, 3.883716857408421319 ) ) ;
#14544 = AXIS2_PLACEMENT_3D ( 'NONE', #127797, #127172, #8015 ) ;
#14545 = DIRECTION ( 'NONE',  ( 0.000000000000000000, -0.000000000000000000, 1.000000000000000000 ) ) ;
#14546 = DIRECTION ( 'NONE',  ( 0.000000000000000000, 1.000000000000000000, 0.000000000000000000 ) ) ;
#14547 = EDGE_CURVE ( 'NONE', #997, #66180, #34778, .T. ) ;
#14548 = CARTESIAN_POINT ( 'NONE',  ( 1.699999999999951994, 12.50000000000000000, -2.276824562219559311E-15 ) ) ;
#14549 = ORIENTED_EDGE ( 'NONE', *, *, #107799, .T. ) ;
#14550 = EDGE_CURVE ( 'NONE', #128041, #94142, #19995, .T. ) ;
#14551 = EDGE_CURVE ( 'NONE', #53518, #96649, #107916, .T. ) ;
#14552 = FACE_OUTER_BOUND ( 'NONE', #126213, .T. ) ;
#14553 = VERTEX_POINT ( 'NONE', #68876 ) ;
#14554 = DIRECTION ( 'NONE',  ( 0.000000000000000000, 1.000000000000000000, 0.000000000000000000 ) ) ;
#14555 = EDGE_LOOP ( 'NONE', ( #35303, #107684 ) ) ;
#14556 = CARTESIAN_POINT ( 'NONE',  ( 185.7812500006828031, 0.000000000000000000, 7.700000000000000178 ) ) ;
#14557 = ADVANCED_FACE ( 'NONE', ( #8020 ), #76622, .T. ) ;
#14558 = VECTOR ( 'NONE', #65505, 1000.000000000000000 ) ;
#14560 = ORIENTED_EDGE ( 'NONE', *, *, #22353, .F. ) ;
#14559 = ADVANCED_FACE ( 'NONE', ( #3368 ), #112686, .T. ) ;
#14561 = ORIENTED_EDGE ( 'NONE', *, *, #69519, .T. ) ;
#14562 = FACE_OUTER_BOUND ( 'NONE', #18435, .T. ) ;
#14563 = CARTESIAN_POINT ( 'NONE',  ( 8.749999999999923617, 2.500000000000000000, -7.188010851410854052 ) ) ;
#14564 = EDGE_CURVE ( 'NONE', #34866, #7578, #1301, .T. ) ;
#14565 = EDGE_CURVE ( 'NONE', #124238, #55845, #45233, .T. ) ;
#14566 = CARTESIAN_POINT ( 'NONE',  ( -6.249999999999984901, 2.500000000000000000, -2.165063509461101710 ) ) ;
#14567 = EDGE_LOOP ( 'NONE', ( #96342, #5407 ) ) ;
#14568 = LINE ( 'NONE', #66250, #105603 ) ;
#14569 = EDGE_LOOP ( 'NONE', ( #122881, #65882, #68301, #81817 ) ) ;
#14570 = CARTESIAN_POINT ( 'NONE',  ( 5.599999999999934808, 2.500000000000000000, -4.576537180435978236 ) ) ;
#14571 = FACE_OUTER_BOUND ( 'NONE', #40006, .T. ) ;
#14572 = LINE ( 'NONE', #123257, #85704 ) ;
#14573 = DIRECTION ( 'NONE',  ( 0.000000000000000000, 1.000000000000000000, 0.000000000000000000 ) ) ;
#14574 = EDGE_CURVE ( 'NONE', #73886, #6433, #64092, .T. ) ;
#14575 = DIRECTION ( 'NONE',  ( 0.000000000000000000, -0.000000000000000000, 1.000000000000000000 ) ) ;
#14576 = ORIENTED_EDGE ( 'NONE', *, *, #64689, .F. ) ;
#14577 = CIRCLE ( 'NONE', #2056, 0.09999999999999982514 ) ;
#14578 = VERTEX_POINT ( 'NONE', #102839 ) ;
#14579 = CARTESIAN_POINT ( 'NONE',  ( -7.700000000000012612, 12.50000000000000000, 4.611443907251934426 ) ) ;
#14580 = CARTESIAN_POINT ( 'NONE',  ( 2.499999999999947153, 12.50000000000000000, -3.637306695894650055 ) ) ;
#14582 = CIRCLE ( 'NONE', #48063, 0.06509327318403745899 ) ;
#14581 = VECTOR ( 'NONE', #86056, 1000.000000000000000 ) ;
#14583 = CIRCLE ( 'NONE', #39676, 0.06509327318403745899 ) ;
#14584 = CARTESIAN_POINT ( 'NONE',  ( 184.4218750003414016, 0.000000000000000000, 7.564683531250000925 ) ) ;
#14585 = DIRECTION ( 'NONE',  ( 0.000000000000000000, 0.000000000000000000, 1.000000000000000000 ) ) ;
#14586 = DIRECTION ( 'NONE',  ( 0.000000000000000000, 0.000000000000000000, -1.000000000000000000 ) ) ;
#14587 = CARTESIAN_POINT ( 'NONE',  ( -6.050000000000017586, 2.500000000000000000, 1.918653347947321564 ) ) ;
#14588 = DIRECTION ( 'NONE',  ( -0.000000000000000000, -1.000000000000000000, -0.000000000000000000 ) ) ;
#14589 = ORIENTED_EDGE ( 'NONE', *, *, #53991, .F. ) ;
#14591 = AXIS2_PLACEMENT_3D ( 'NONE', #47154, #118458, #77255 ) ;
#14590 = AXIS2_PLACEMENT_3D ( 'NONE', #2180, #25052, #42120 ) ;
#14592 = CARTESIAN_POINT ( 'NONE',  ( 7.099999999999927702, 2.500000000000000000, -3.637306695894650055 ) ) ;
#14593 = CARTESIAN_POINT ( 'NONE',  ( 4.599999999999937472, 2.500000000000000000, 0.5928203230275495006 ) ) ;
#14594 = FACE_OUTER_BOUND ( 'NONE', #80746, .T. ) ;
#14595 = ORIENTED_EDGE ( 'NONE', *, *, #103376, .T. ) ;
#14596 = DIRECTION ( 'NONE',  ( -4.274815082592931898E-19, -0.9999939076577903929, -0.003490651415223739937 ) ) ;
#14597 = EDGE_CURVE ( 'NONE', #83387, #123828, #49451, .T. ) ;
#14598 = ORIENTED_EDGE ( 'NONE', *, *, #78079, .T. ) ;
#14599 = LINE ( 'NONE', #34284, #44671 ) ;
#14600 = ORIENTED_EDGE ( 'NONE', *, *, #4214, .T. ) ;
#14601 = DIRECTION ( 'NONE',  ( 0.000000000000000000, 1.000000000000000000, 0.000000000000000000 ) ) ;
#14602 = DIRECTION ( 'NONE',  ( 0.000000000000000000, 1.000000000000000000, 0.000000000000000000 ) ) ;
#14603 = DIRECTION ( 'NONE',  ( -0.000000000000000000, 1.000000000000000000, -0.000000000000000000 ) ) ;
#14604 = VERTEX_POINT ( 'NONE', #70182 ) ;
#14605 = CIRCLE ( 'NONE', #39707, 0.06509327318403745899 ) ;
#14606 = DIRECTION ( 'NONE',  ( 0.000000000000000000, 1.000000000000000000, 0.000000000000000000 ) ) ;
#14607 = AXIS2_PLACEMENT_3D ( 'NONE', #27085, #99697, #48659 ) ;
#14608 = CARTESIAN_POINT ( 'NONE',  ( -8.950000000000009948, 2.500000000000000000, -6.941600689897073018 ) ) ;
#14609 = ORIENTED_EDGE ( 'NONE', *, *, #123504, .T. ) ;
#14610 = AXIS2_PLACEMENT_3D ( 'NONE', #77329, #116599, #17081 ) ;
#14611 = CARTESIAN_POINT ( 'NONE',  ( 10.39999999999991509, 12.50000000000000000, 0.6928203230275494784 ) ) ;
#14612 = EDGE_LOOP ( 'NONE', ( #96484, #34652, #81617, #83569 ) ) ;
#14613 = ORIENTED_EDGE ( 'NONE', *, *, #61064, .T. ) ;
#14614 = LINE ( 'NONE', #53293, #113205 ) ;
#14615 = CARTESIAN_POINT ( 'NONE',  ( -4.150000000000024336, 2.500000000000000000, -2.857883832488653741 ) ) ;
#14616 = FACE_OUTER_BOUND ( 'NONE', #83764, .T. ) ;
#14617 = VERTEX_POINT ( 'NONE', #2712 ) ;
#14618 = VECTOR ( 'NONE', #31252, 1000.000000000000000 ) ;
#14619 = CARTESIAN_POINT ( 'NONE',  ( 129.5000000000000000, -0.6250000000000004441, 6.000000000000000000 ) ) ;
#14620 = DIRECTION ( 'NONE',  ( -4.274815082592931898E-19, -0.9999939076577903929, -0.003490651415223739937 ) ) ;
#14621 = ORIENTED_EDGE ( 'NONE', *, *, #65101, .T. ) ;
#14623 = FACE_OUTER_BOUND ( 'NONE', #114680, .T. ) ;
#14622 = CONICAL_SURFACE ( 'NONE', #31394, 0.09999999999999999167, 0.003490658503988666988 ) ;
#14624 = CARTESIAN_POINT ( 'NONE',  ( -13.14999999999999147, 12.50000000000000000, -2.511473670974875727 ) ) ;
#14625 = AXIS2_PLACEMENT_3D ( 'NONE', #31534, #111357, #2055 ) ;
#14626 = CARTESIAN_POINT ( 'NONE',  ( -15.39999999999998082, 12.50000000000000000, 0.6928203230275518099 ) ) ;
#14627 = FACE_OUTER_BOUND ( 'NONE', #111432, .T. ) ;
#14628 = DIRECTION ( 'NONE',  ( 0.000000000000000000, 0.000000000000000000, 1.000000000000000000 ) ) ;
#14629 = VECTOR ( 'NONE', #46547, 1000.000000000000000 ) ;
#14630 = CARTESIAN_POINT ( 'NONE',  ( 12.89999999999990088, 2.500000000000000000, 4.230127018922196669 ) ) ;
#14631 = DIRECTION ( 'NONE',  ( -0.000000000000000000, 1.000000000000000000, -0.000000000000000000 ) ) ;
#14632 = AXIS2_PLACEMENT_3D ( 'NONE', #56121, #55494, #115686 ) ;
#14633 = EDGE_CURVE ( 'NONE', #29713, #128031, #20187, .T. ) ;
#14634 = ORIENTED_EDGE ( 'NONE', *, *, #55525, .F. ) ;
#14635 = ORIENTED_EDGE ( 'NONE', *, *, #49910, .F. ) ;
#14636 = EDGE_LOOP ( 'NONE', ( #51257, #54418, #80668, #63802 ) ) ;
#14637 = ORIENTED_EDGE ( 'NONE', *, *, #122149, .F. ) ;
#14638 = AXIS2_PLACEMENT_3D ( 'NONE', #109301, #18340, #88353 ) ;
#14639 = CARTESIAN_POINT ( 'NONE',  ( 3.549999999999940314, 12.50000000000000000, 6.906693963081109722 ) ) ;
#14640 = CARTESIAN_POINT ( 'NONE',  ( 7.299999999999926104, 12.50000000000000000, 4.741630453620009789 ) ) ;
#14641 = CARTESIAN_POINT ( 'NONE',  ( 7.899999999999923084, 2.500000000000000000, -0.5928203230275542746 ) ) ;
#14642 = EDGE_LOOP ( 'NONE', ( #20808, #50642 ) ) ;
#14643 = ADVANCED_FACE ( 'NONE', ( #53122 ), #126800, .T. ) ;
#14644 = FACE_BOUND ( 'NONE', #29822, .T. ) ;
#14645 = ADVANCED_FACE ( 'NONE', ( #101573 ), #32726, .T. ) ;
#14646 = DIRECTION ( 'NONE',  ( -0.000000000000000000, -1.000000000000000000, -0.000000000000000000 ) ) ;
#14647 = CARTESIAN_POINT ( 'NONE',  ( -2.100000000000033396, 2.500000000000000000, -0.5928203230275542746 ) ) ;
#14648 = DIRECTION ( 'NONE',  ( -4.274815082592931898E-19, -0.9999939076577903929, -0.003490651415223739937 ) ) ;
#14649 = CARTESIAN_POINT ( 'NONE',  ( 12.04999999999990834, 2.500000000000000000, -2.265063509461101798 ) ) ;
#14650 = CARTESIAN_POINT ( 'NONE',  ( 3.149999999999946176, 2.500000000000000000, -6.248780366869526759 ) ) ;
#14651 = EDGE_CURVE ( 'NONE', #106111, #111925, #122598, .T. ) ;
#14652 = DIRECTION ( 'NONE',  ( 0.000000000000000000, 0.000000000000000000, 1.000000000000000000 ) ) ;
#14653 = ADVANCED_FACE ( 'NONE', ( #72119 ), #57758, .T. ) ;
#14654 = CARTESIAN_POINT ( 'NONE',  ( 0.6499999999999566125, 12.50000000000000000, -6.841600689897077814 ) ) ;
#14655 = DIRECTION ( 'NONE',  ( 0.000000000000000000, 0.000000000000000000, 1.000000000000000000 ) ) ;
#14656 = EDGE_CURVE ( 'NONE', #18715, #18830, #121203, .T. ) ;
#14657 = CARTESIAN_POINT ( 'NONE',  ( 11.84999999999990372, 12.50000000000000000, 1.883746621131358934 ) ) ;
#14658 = EDGE_CURVE ( 'NONE', #10004, #20333, #99614, .T. ) ;
#14659 = EDGE_CURVE ( 'NONE', #126889, #11040, #3462, .T. ) ;
#14660 = FACE_OUTER_BOUND ( 'NONE', #22143, .T. ) ;
#14661 = ORIENTED_EDGE ( 'NONE', *, *, #13804, .F. ) ;
#14662 = ORIENTED_EDGE ( 'NONE', *, *, #13497, .T. ) ;
#14663 = VERTEX_POINT ( 'NONE', #20432 ) ;
#14664 = ORIENTED_EDGE ( 'NONE', *, *, #122607, .T. ) ;
#14665 = DIRECTION ( 'NONE',  ( 0.000000000000000000, 1.000000000000000000, 0.000000000000000000 ) ) ;
#14666 = ORIENTED_EDGE ( 'NONE', *, *, #100403, .T. ) ;
#14667 = AXIS2_PLACEMENT_3D ( 'NONE', #102458, #100513, #81530 ) ;
#14668 = CARTESIAN_POINT ( 'NONE',  ( -0.8500000000000382805, 12.50000000000000000, -2.857883832488653741 ) ) ;
#14669 = CONICAL_SURFACE ( 'NONE', #8414, 0.1000000000000000472, 0.003490658503988666988 ) ;
#14670 = EDGE_LOOP ( 'NONE', ( #7732, #7586, #92325, #87026 ) ) ;
#14671 = EDGE_CURVE ( 'NONE', #2125, #83526, #42006, .T. ) ;
#14672 = ORIENTED_EDGE ( 'NONE', *, *, #42509, .T. ) ;
#14673 = AXIS2_PLACEMENT_3D ( 'NONE', #29152, #108957, #80821 ) ;
#14674 = CARTESIAN_POINT ( 'NONE',  ( 6.714630671517820559, -1.499999999999809708, 9.763603585529462947 ) ) ;
#14675 = CARTESIAN_POINT ( 'NONE',  ( -7.500000000000015099, 2.500000000000000000, -5.022947341949754119 ) ) ;
#14676 = FACE_OUTER_BOUND ( 'NONE', #89649, .T. ) ;
#14677 = LINE ( 'NONE', #54604, #53842 ) ;
#14678 = ORIENTED_EDGE ( 'NONE', *, *, #8606, .F. ) ;
#14679 = ORIENTED_EDGE ( 'NONE', *, *, #57830, .F. ) ;
#14680 = ORIENTED_EDGE ( 'NONE', *, *, #123776, .T. ) ;
#14682 = EDGE_LOOP ( 'NONE', ( #32200, #68385 ) ) ;
#14681 = FACE_OUTER_BOUND ( 'NONE', #70610, .T. ) ;
#14683 = CARTESIAN_POINT ( 'NONE',  ( 3.349999999999941025, 2.500000000000000000, 7.088010851410848190 ) ) ;
#14684 = VERTEX_POINT ( 'NONE', #62931 ) ;
#14685 = ORIENTED_EDGE ( 'NONE', *, *, #72479, .F. ) ;
#14686 = DIRECTION ( 'NONE',  ( 0.000000000000000000, 0.000000000000000000, 1.000000000000000000 ) ) ;
#14687 = CARTESIAN_POINT ( 'NONE',  ( -13.54999999999999005, 12.50000000000000000, -1.883746621131361376 ) ) ;
#14688 = CARTESIAN_POINT ( 'NONE',  ( -9.600000000000008527, 12.50000000000000000, 0.06509327318403504425 ) ) ;
#14689 = DIRECTION ( 'NONE',  ( 0.000000000000000000, 0.000000000000000000, -1.000000000000000000 ) ) ;
#14690 = DIRECTION ( 'NONE',  ( 0.000000000000000000, -0.9999939076577903929, 0.003490651415223739937 ) ) ;
#14691 = EDGE_CURVE ( 'NONE', #84006, #49812, #11892, .T. ) ;
#14692 = EDGE_LOOP ( 'NONE', ( #48349, #107094 ) ) ;
#14693 = EDGE_CURVE ( 'NONE', #81036, #26833, #72422, .T. ) ;
#14694 = DIRECTION ( 'NONE',  ( 0.000000000000000000, -0.9999939076577903929, 0.003490651415223739937 ) ) ;
#14695 = AXIS2_PLACEMENT_3D ( 'NONE', #10507, #40657, #104686 ) ;
#14696 = AXIS2_PLACEMENT_3D ( 'NONE', #101979, #42422, #82351 ) ;
#14697 = ORIENTED_EDGE ( 'NONE', *, *, #23886, .F. ) ;
#14699 = EDGE_CURVE ( 'NONE', #80576, #53696, #93344, .T. ) ;
#14698 = CARTESIAN_POINT ( 'NONE',  ( 87.50000000000002842, 5.708722954879577927, -4.899943752027914101 ) ) ;
#14700 = ORIENTED_EDGE ( 'NONE', *, *, #61244, .F. ) ;
#14701 = CARTESIAN_POINT ( 'NONE',  ( -6.249999999999981348, 12.50000000000000000, 6.430097255199259010 ) ) ;
#14702 = CARTESIAN_POINT ( 'NONE',  ( -1.250000000000001110, 2.500000000000000000, -2.165063509461101710 ) ) ;
#14703 = DIRECTION ( 'NONE',  ( 0.000000000000000000, 0.000000000000000000, 1.000000000000000000 ) ) ;
#14704 = ADVANCED_FACE ( 'NONE', ( #80652 ), #70357, .T. ) ;
#14705 = DIRECTION ( 'NONE',  ( 0.000000000000000000, 1.000000000000000000, 0.000000000000000000 ) ) ;
#14706 = ORIENTED_EDGE ( 'NONE', *, *, #110387, .T. ) ;
#14707 = VECTOR ( 'NONE', #83684, 1000.000000000000000 ) ;
#14708 = ADVANCED_FACE ( 'NONE', ( #65501 ), #11765, .T. ) ;
#14709 = CARTESIAN_POINT ( 'NONE',  ( -13.74999999999998757, 2.500000000000000000, 1.572243186433549544 ) ) ;
#14710 = ADVANCED_FACE ( 'NONE', ( #15748 ), #84932, .T. ) ;
#14711 = EDGE_CURVE ( 'NONE', #107108, #30682, #53632, .T. ) ;
#14712 = CARTESIAN_POINT ( 'NONE',  ( -4.350000000000027178, 2.500000000000000000, -6.841600689897077814 ) ) ;
#14713 = EDGE_LOOP ( 'NONE', ( #95763, #59497, #116777, #90557 ) ) ;
#14714 = ORIENTED_EDGE ( 'NONE', *, *, #14789, .F. ) ;
#14715 = ORIENTED_EDGE ( 'NONE', *, *, #122852, .T. ) ;
#14716 = CARTESIAN_POINT ( 'NONE',  ( 1.899999999999951283, 2.500000000000000000, 0.4464101615137736623 ) ) ;
#14717 = CARTESIAN_POINT ( 'NONE',  ( 2.949999999999946887, 2.500000000000000000, -6.495190528383302464 ) ) ;
#14718 = CARTESIAN_POINT ( 'NONE',  ( 184.4843750003414016, -8.734944146203032389, -1.604583208406768146E-15 ) ) ;
#14719 = DIRECTION ( 'NONE',  ( 0.000000000000000000, 0.000000000000000000, 1.000000000000000000 ) ) ;
#14720 = ADVANCED_FACE ( 'NONE', ( #74688 ), #74475, .T. ) ;
#14721 = CONICAL_SURFACE ( 'NONE', #69016, 0.09999999999999982514, 0.003490658503988666988 ) ;
#14722 = CARTESIAN_POINT ( 'NONE',  ( 17.10613367507962224, 2.036230694789155304, -5.376205058613481746 ) ) ;
#14723 = CARTESIAN_POINT ( 'NONE',  ( -1.450000000000036371, 2.500000000000000000, 2.511473670974873507 ) ) ;
#14724 = CIRCLE ( 'NONE', #4259, 0.06509327318403745899 ) ;
#14725 = ORIENTED_EDGE ( 'NONE', *, *, #112539, .T. ) ;
#14726 = DIRECTION ( 'NONE',  ( 0.000000000000000000, 0.000000000000000000, -1.000000000000000000 ) ) ;
#14727 = ORIENTED_EDGE ( 'NONE', *, *, #38522, .F. ) ;
#14728 = DIRECTION ( 'NONE',  ( 0.000000000000000000, 0.000000000000000000, 1.000000000000000000 ) ) ;
#14729 = EDGE_CURVE ( 'NONE', #114625, #3837, #13817, .T. ) ;
#14730 = CARTESIAN_POINT ( 'NONE',  ( -4.350000000000023626, 2.500000000000000000, 1.918653347947321564 ) ) ;
#14731 = LINE ( 'NONE', #105054, #2062 ) ;
#14732 = ORIENTED_EDGE ( 'NONE', *, *, #9950, .T. ) ;
#14733 = CYLINDRICAL_SURFACE ( 'NONE', #101479, 3.000000000000000000 ) ;
#14734 = FACE_OUTER_BOUND ( 'NONE', #38299, .T. ) ;
#14735 = VERTEX_POINT ( 'NONE', #25567 ) ;
#14736 = CARTESIAN_POINT ( 'NONE',  ( -10.60000000000000142, 2.500000000000000000, 3.983716857408420964 ) ) ;
#14737 = EDGE_CURVE ( 'NONE', #32850, #31560, #83851, .T. ) ;
#14738 = ORIENTED_EDGE ( 'NONE', *, *, #102751, .T. ) ;
#14739 = VERTEX_POINT ( 'NONE', #63586 ) ;
#14740 = DIRECTION ( 'NONE',  ( -0.000000000000000000, 1.000000000000000000, -0.000000000000000000 ) ) ;
#14741 = CONICAL_SURFACE ( 'NONE', #117242, 0.1000000000000002554, 0.003490658503988666988 ) ;
#14742 = AXIS2_PLACEMENT_3D ( 'NONE', #90039, #29850, #109706 ) ;
#14743 = ORIENTED_EDGE ( 'NONE', *, *, #89732, .T. ) ;
#14744 = CARTESIAN_POINT ( 'NONE',  ( 15.24415751722852086, 2.474878586408646441, -4.460068884075279350 ) ) ;
#14745 = DIRECTION ( 'NONE',  ( 0.000000000000000000, 1.000000000000000000, 0.000000000000000000 ) ) ;
#14746 = FACE_OUTER_BOUND ( 'NONE', #63807, .T. ) ;
#14747 = ORIENTED_EDGE ( 'NONE', *, *, #87837, .T. ) ;
#14749 = FACE_BOUND ( 'NONE', #6346, .T. ) ;
#14748 = AXIS2_PLACEMENT_3D ( 'NONE', #57765, #7347, #97674 ) ;
#14750 = CARTESIAN_POINT ( 'NONE',  ( -3.550000000000031797, 2.500000000000000000, -6.048780366869526581 ) ) ;
#14752 = EDGE_LOOP ( 'NONE', ( #95595, #71011 ) ) ;
#14751 = DIRECTION ( 'NONE',  ( -0.000000000000000000, 1.000000000000000000, -0.000000000000000000 ) ) ;
#14753 = CONICAL_SURFACE ( 'NONE', #33666, 0.1000000000000002554, 0.003490658503988666988 ) ;
#14754 = CARTESIAN_POINT ( 'NONE',  ( 2.099999999999949463, 2.500000000000000000, -3.537306695894649966 ) ) ;
#14755 = ADVANCED_FACE ( 'NONE', ( #105443 ), #24297, .T. ) ;
#14756 = CARTESIAN_POINT ( 'NONE',  ( -9.600000000000008527, 12.50000000000000000, 4.395220292106234439 ) ) ;
#14757 = ORIENTED_EDGE ( 'NONE', *, *, #25210, .F. ) ;
#14758 = ORIENTED_EDGE ( 'NONE', *, *, #92576, .F. ) ;
#14759 = ORIENTED_EDGE ( 'NONE', *, *, #65628, .F. ) ;
#14760 = CARTESIAN_POINT ( 'NONE',  ( 15.59999999999988951, 2.500000000000000000, 0.3464101615137735735 ) ) ;
#14761 = CARTESIAN_POINT ( 'NONE',  ( 4.913542845204887044, 2.499999999999490630, 9.942462991356222801 ) ) ;
#14762 = CARTESIAN_POINT ( 'NONE',  ( 12.04999999999990479, 2.500000000000000000, 2.065063509461097624 ) ) ;
#14763 = FACE_BOUND ( 'NONE', #115835, .T. ) ;
#14764 = ORIENTED_EDGE ( 'NONE', *, *, #111177, .T. ) ;
#14765 = CARTESIAN_POINT ( 'NONE',  ( 185.4427083336747160, -6.551208109652278289, 3.782341765624995134 ) ) ;
#14766 = LINE ( 'NONE', #5601, #128469 ) ;
#14767 = DIRECTION ( 'NONE',  ( 0.000000000000000000, 0.000000000000000000, -1.000000000000000000 ) ) ;
#14768 = DIRECTION ( 'NONE',  ( 0.000000000000000000, 0.000000000000000000, 1.000000000000000000 ) ) ;
#14769 = DIRECTION ( 'NONE',  ( -4.274815082592931898E-19, -0.9999939076577903929, -0.003490651415223739937 ) ) ;
#14770 = CARTESIAN_POINT ( 'NONE',  ( 179.5000000000000000, -1.375000000000000000, 7.634788798650553154 ) ) ;
#14771 = DIRECTION ( 'NONE',  ( 0.000000000000000000, 0.000000000000000000, 1.000000000000000000 ) ) ;
#14772 = AXIS2_PLACEMENT_3D ( 'NONE', #95565, #103455, #83175 ) ;
#14773 = CIRCLE ( 'NONE', #21062, 0.1000000000000002554 ) ;
#14774 = DIRECTION ( 'NONE',  ( 0.000000000000000000, -0.9999939076577903929, 0.003490651415223739937 ) ) ;
#14775 = EDGE_CURVE ( 'NONE', #31372, #88700, #61956, .T. ) ;
#14776 = ORIENTED_EDGE ( 'NONE', *, *, #41068, .T. ) ;
#14777 = EDGE_LOOP ( 'NONE', ( #97360, #96448, #42090, #18338 ) ) ;
#14778 = ORIENTED_EDGE ( 'NONE', *, *, #87307, .T. ) ;
#14779 = ORIENTED_EDGE ( 'NONE', *, *, #4938, .T. ) ;
#14780 = VERTEX_POINT ( 'NONE', #34129 ) ;
#14781 = CARTESIAN_POINT ( 'NONE',  ( -12.09999999999999432, 12.50000000000000000, 3.637306695894644726 ) ) ;
#14782 = DIRECTION ( 'NONE',  ( -0.000000000000000000, -1.000000000000000000, -0.000000000000000000 ) ) ;
#14783 = ORIENTED_EDGE ( 'NONE', *, *, #68147, .F. ) ;
#14784 = FACE_BOUND ( 'NONE', #115359, .T. ) ;
#14785 = CONICAL_SURFACE ( 'NONE', #104606, 0.1000000000000002554, 0.003490658503988666988 ) ;
#14786 = CARTESIAN_POINT ( 'NONE',  ( -2.950000000000033484, 2.500000000000000000, -6.495190528383302464 ) ) ;
#14787 = DIRECTION ( 'NONE',  ( 0.000000000000000000, 1.000000000000000000, 0.000000000000000000 ) ) ;
#14788 = VERTEX_POINT ( 'NONE', #15085 ) ;
#14789 = EDGE_CURVE ( 'NONE', #105063, #14247, #55684, .T. ) ;
#14790 = CARTESIAN_POINT ( 'NONE',  ( 7.049999999999928768, 2.500000000000000000, 6.495190528383297135 ) ) ;
#14791 = ADVANCED_FACE ( 'NONE', ( #106083 ), #3548, .T. ) ;
#14792 = LINE ( 'NONE', #54736, #17684 ) ;
#14793 = EDGE_CURVE ( 'NONE', #103547, #125357, #128970, .T. ) ;
#14794 = FACE_OUTER_BOUND ( 'NONE', #44310, .T. ) ;
#14795 = EDGE_CURVE ( 'NONE', #47117, #51312, #122677, .T. ) ;
#14796 = ORIENTED_EDGE ( 'NONE', *, *, #9119, .F. ) ;
#14797 = DIRECTION ( 'NONE',  ( 0.000000000000000000, 0.000000000000000000, 1.000000000000000000 ) ) ;
#14798 = VERTEX_POINT ( 'NONE', #94311 ) ;
#14799 = VECTOR ( 'NONE', #25238, 1000.000000000000000 ) ;
#14800 = ADVANCED_FACE ( 'NONE', ( #85143 ), #80925, .T. ) ;
#14801 = ORIENTED_EDGE ( 'NONE', *, *, #119379, .T. ) ;
#14802 = ORIENTED_EDGE ( 'NONE', *, *, #66433, .T. ) ;
#14803 = DIRECTION ( 'NONE',  ( 0.000000000000000000, 0.000000000000000000, 1.000000000000000000 ) ) ;
#14804 = DIRECTION ( 'NONE',  ( 0.000000000000000000, 0.000000000000000000, 1.000000000000000000 ) ) ;
#14805 = DIRECTION ( 'NONE',  ( 0.000000000000000000, -0.9999939076577903929, 0.003490651415223739937 ) ) ;
#14806 = ORIENTED_EDGE ( 'NONE', *, *, #66418, .T. ) ;
#14807 = EDGE_CURVE ( 'NONE', #88198, #7615, #24942, .T. ) ;
#14808 = CARTESIAN_POINT ( 'NONE',  ( 4.848431875657850831, 2.499999999999999556, -8.943854603572997775 ) ) ;
#14809 = AXIS2_PLACEMENT_3D ( 'NONE', #35253, #54863, #5122 ) ;
#14810 = EDGE_CURVE ( 'NONE', #34747, #62008, #64855, .T. ) ;
#14811 = CARTESIAN_POINT ( 'NONE',  ( 5.849999999999933031, 2.500000000000000000, 7.288010851410849256 ) ) ;
#14812 = EDGE_CURVE ( 'NONE', #95681, #93842, #125074, .T. ) ;
#14813 = CARTESIAN_POINT ( 'NONE',  ( 6.849999999999927702, 2.500000000000000000, 1.918653347947321564 ) ) ;
#14814 = CIRCLE ( 'NONE', #64999, 0.06509327318403745899 ) ;
#14815 = CARTESIAN_POINT ( 'NONE',  ( 185.2395833340161175, 4.445597072760117285, 7.699999999999999289 ) ) ;
#14817 = ORIENTED_EDGE ( 'NONE', *, *, #57080, .F. ) ;
#14816 = CARTESIAN_POINT ( 'NONE',  ( 11.24999999999994316, 2.500000000000000000, -6.395190528383301931 ) ) ;
#14818 = PRODUCT_DEFINITION ( 'UNKNOWN', '', #92276, #105660 ) ;
#14819 = DIRECTION ( 'NONE',  ( 0.000000000000000000, 1.000000000000000000, 0.000000000000000000 ) ) ;
#14820 = EDGE_CURVE ( 'NONE', #3679, #59594, #110169, .T. ) ;
#14821 = VERTEX_POINT ( 'NONE', #55687 ) ;
#14822 = CARTESIAN_POINT ( 'NONE',  ( 7.099999999999928590, 2.500000000000000000, 3.537306695894645081 ) ) ;
#14823 = ORIENTED_EDGE ( 'NONE', *, *, #20146, .T. ) ;
#14824 = VERTEX_POINT ( 'NONE', #116536 ) ;
#14825 = DIRECTION ( 'NONE',  ( 0.000000000000000000, 1.000000000000000000, 0.000000000000000000 ) ) ;
#14826 = CARTESIAN_POINT ( 'NONE',  ( -7.100000000000013856, 2.500000000000000000, 3.737306695894644371 ) ) ;
#14827 = DIRECTION ( 'NONE',  ( -0.000000000000000000, -1.000000000000000000, -0.000000000000000000 ) ) ;
#14828 = DIRECTION ( 'NONE',  ( -4.274815082592931898E-19, -0.9999939076577903929, -0.003490651415223739937 ) ) ;
#14829 = LINE ( 'NONE', #5026, #26702 ) ;
#14830 = ORIENTED_EDGE ( 'NONE', *, *, #105595, .F. ) ;
#14831 = ORIENTED_EDGE ( 'NONE', *, *, #41235, .T. ) ;
#14832 = DIRECTION ( 'NONE',  ( 0.000000000000000000, 1.000000000000000000, 0.000000000000000000 ) ) ;
#14833 = DIRECTION ( 'NONE',  ( 0.000000000000000000, 1.000000000000000000, 0.000000000000000000 ) ) ;
#14835 = DIRECTION ( 'NONE',  ( -0.000000000000000000, -1.000000000000000000, -0.000000000000000000 ) ) ;
#14834 = CONICAL_SURFACE ( 'NONE', #19050, 0.1000000000000000472, 0.003490658503988666988 ) ;
#14836 = EDGE_LOOP ( 'NONE', ( #119214, #127360 ) ) ;
#14837 = ORIENTED_EDGE ( 'NONE', *, *, #53286, .F. ) ;
#14838 = CONICAL_SURFACE ( 'NONE', #98469, 0.1000000000000000472, 0.003490658503988666988 ) ;
#14839 = VECTOR ( 'NONE', #57875, 1000.000000000000000 ) ;
#14840 = CARTESIAN_POINT ( 'NONE',  ( -6.050000000000022027, 2.500000000000000000, -1.918653347947326004 ) ) ;
#14841 = VERTEX_POINT ( 'NONE', #17687 ) ;
#14842 = DIRECTION ( 'NONE',  ( 0.000000000000000000, 0.000000000000000000, -1.000000000000000000 ) ) ;
#14843 = AXIS2_PLACEMENT_3D ( 'NONE', #87045, #16353, #96865 ) ;
#14844 = FACE_OUTER_BOUND ( 'NONE', #122753, .T. ) ;
#14845 = EDGE_LOOP ( 'NONE', ( #67908, #105755, #105138, #9713 ) ) ;
#14846 = FACE_OUTER_BOUND ( 'NONE', #31651, .T. ) ;
#14847 = FACE_OUTER_BOUND ( 'NONE', #35619, .T. ) ;
#14848 = CARTESIAN_POINT ( 'NONE',  ( 2.699999999999944666, 2.500000000000000000, 4.676537180435972552 ) ) ;
#14849 = CONICAL_SURFACE ( 'NONE', #106898, 0.1000000000000002554, 0.003490658503988666988 ) ;
#14850 = CARTESIAN_POINT ( 'NONE',  ( 0.4499999999999552136, 2.500000000000000000, 6.495190528383297135 ) ) ;
#14851 = ORIENTED_EDGE ( 'NONE', *, *, #51179, .F. ) ;
#14852 = EDGE_CURVE ( 'NONE', #31487, #85147, #16045, .T. ) ;
#14853 = DIRECTION ( 'NONE',  ( 0.000000000000000000, 0.000000000000000000, 1.000000000000000000 ) ) ;
#14855 = ADVANCED_FACE ( 'NONE', ( #57632 ), #20274, .T. ) ;
#14854 = DIRECTION ( 'NONE',  ( 0.000000000000000000, 1.000000000000000000, 0.000000000000000000 ) ) ;
#14856 = EDGE_LOOP ( 'NONE', ( #42196, #40888, #100993, #102917 ) ) ;
#14857 = ORIENTED_EDGE ( 'NONE', *, *, #12751, .T. ) ;
#14858 = CARTESIAN_POINT ( 'NONE',  ( 185.7135416670080588, 4.367472073101518859, -7.564683531249999149 ) ) ;
#14859 = LINE ( 'NONE', #35196, #65774 ) ;
#14860 = DIRECTION ( 'NONE',  ( 0.000000000000000000, 0.000000000000000000, 1.000000000000000000 ) ) ;
#14861 = DIRECTION ( 'NONE',  ( 0.000000000000000000, 1.000000000000000000, 0.000000000000000000 ) ) ;
#14862 = EDGE_CURVE ( 'NONE', #82663, #30237, #47166, .T. ) ;
#14863 = DIRECTION ( 'NONE',  ( -0.000000000000000000, -1.000000000000000000, -0.000000000000000000 ) ) ;
#14864 = AXIS2_PLACEMENT_3D ( 'NONE', #117695, #126906, #38548 ) ;
#14865 = DIRECTION ( 'NONE',  ( 0.000000000000000000, 1.000000000000000000, 0.000000000000000000 ) ) ;
#14866 = DIRECTION ( 'NONE',  ( 0.000000000000000000, 0.000000000000000000, -1.000000000000000000 ) ) ;
#14867 = DIRECTION ( 'NONE',  ( 0.000000000000000000, 0.000000000000000000, 1.000000000000000000 ) ) ;
#14868 = CARTESIAN_POINT ( 'NONE',  ( -12.49999999999999467, 12.50000000000000000, -3.572213422710609709 ) ) ;
#14869 = DIRECTION ( 'NONE',  ( 0.000000000000000000, 1.000000000000000000, 0.000000000000000000 ) ) ;
#14870 = AXIS2_PLACEMENT_3D ( 'NONE', #37297, #97492, #18280 ) ;
#14871 = ORIENTED_EDGE ( 'NONE', *, *, #96525, .T. ) ;
#14872 = EDGE_LOOP ( 'NONE', ( #45782, #50244, #91802, #34045 ) ) ;
#14873 = VERTEX_POINT ( 'NONE', #97541 ) ;
#14874 = ORIENTED_EDGE ( 'NONE', *, *, #50573, .F. ) ;
#14875 = CARTESIAN_POINT ( 'NONE',  ( -2.499999999999996003, 2.500000000000000000, -4.430127018922202176 ) ) ;
#14876 = DIRECTION ( 'NONE',  ( -0.000000000000000000, -1.000000000000000000, -0.000000000000000000 ) ) ;
#14877 = CARTESIAN_POINT ( 'NONE',  ( 6.249999999999934275, 2.500000000000000000, -7.288010851410854585 ) ) ;
#14878 = AXIS2_PLACEMENT_3D ( 'NONE', #64831, #106052, #4590 ) ;
#14879 = AXIS2_PLACEMENT_3D ( 'NONE', #120353, #60156, #100062 ) ;
#14880 = EDGE_LOOP ( 'NONE', ( #73963, #96755 ) ) ;
#14881 = DIRECTION ( 'NONE',  ( 0.000000000000000000, 1.000000000000000000, 0.000000000000000000 ) ) ;
#14882 = DIRECTION ( 'NONE',  ( 0.000000000000000000, 0.000000000000000000, 1.000000000000000000 ) ) ;
#14884 = ORIENTED_EDGE ( 'NONE', *, *, #57969, .F. ) ;
#14883 = DIRECTION ( 'NONE',  ( 0.000000000000000000, 0.000000000000000000, 1.000000000000000000 ) ) ;
#14885 = DIRECTION ( 'NONE',  ( 0.000000000000000000, 0.000000000000000000, 1.000000000000000000 ) ) ;
#14886 = CIRCLE ( 'NONE', #2378, 0.1000000000000000472 ) ;
#14887 = VERTEX_POINT ( 'NONE', #68726 ) ;
#14888 = AXIS2_PLACEMENT_3D ( 'NONE', #37669, #118792, #127967 ) ;
#14889 = EDGE_LOOP ( 'NONE', ( #89922, #83309 ) ) ;
#14890 = ORIENTED_EDGE ( 'NONE', *, *, #50963, .T. ) ;
#14892 = VERTEX_POINT ( 'NONE', #48445 ) ;
#14891 = CIRCLE ( 'NONE', #63053, 0.09999999999999982514 ) ;
#14893 = DIRECTION ( 'NONE',  ( 0.000000000000000000, 0.000000000000000000, -1.000000000000000000 ) ) ;
#14894 = AXIS2_PLACEMENT_3D ( 'NONE', #28655, #108481, #118950 ) ;
#14895 = CARTESIAN_POINT ( 'NONE',  ( 0.5999999999999621192, 2.500000000000000000, 0.4464101615137758272 ) ) ;
#14896 = DIRECTION ( 'NONE',  ( -0.000000000000000000, 1.000000000000000000, -0.000000000000000000 ) ) ;
#14897 = DIRECTION ( 'NONE',  ( 0.000000000000000000, 0.000000000000000000, 1.000000000000000000 ) ) ;
#14898 = ORIENTED_EDGE ( 'NONE', *, *, #70668, .F. ) ;
#14899 = AXIS2_PLACEMENT_3D ( 'NONE', #101600, #63609, #11915 ) ;
#14900 = AXIS2_PLACEMENT_3D ( 'NONE', #96019, #6318, #8270 ) ;
#14901 = CARTESIAN_POINT ( 'NONE',  ( 15.19999999999989271, 12.50000000000000000, -0.3464101615137783474 ) ) ;
#14903 = EDGE_LOOP ( 'NONE', ( #90595, #63160, #58820, #2268 ) ) ;
#14902 = EDGE_CURVE ( 'NONE', #31023, #63981, #60013, .T. ) ;
#14904 = CARTESIAN_POINT ( 'NONE',  ( -0.8500000000000390576, 2.500000000000000000, -6.495190528383302464 ) ) ;
#14905 = DIRECTION ( 'NONE',  ( -4.274815082592931898E-19, -0.9999939076577903929, -0.003490651415223739937 ) ) ;
#14906 = DIRECTION ( 'NONE',  ( 0.000000000000000000, 0.000000000000000000, 1.000000000000000000 ) ) ;
#14907 = DIRECTION ( 'NONE',  ( 0.000000000000000000, -0.9999939076577903929, 0.003490651415223739937 ) ) ;
#14908 = EDGE_CURVE ( 'NONE', #89282, #111058, #53721, .T. ) ;
#14909 = ORIENTED_EDGE ( 'NONE', *, *, #41056, .T. ) ;
#14910 = ORIENTED_EDGE ( 'NONE', *, *, #126436, .F. ) ;
#14911 = EDGE_LOOP ( 'NONE', ( #46141, #8446, #129296, #29986 ) ) ;
#14912 = CARTESIAN_POINT ( 'NONE',  ( -8.749999999999971578, 2.500000000000000000, 6.595190528383296780 ) ) ;
#14913 = CARTESIAN_POINT ( 'NONE',  ( -10.40000000000000213, 12.50000000000000000, -0.6277270498435166823 ) ) ;
#14914 = ADVANCED_FACE ( 'NONE', ( #39310, #6544 ), #67409, .F. ) ;
#14915 = CARTESIAN_POINT ( 'NONE',  ( -12.09999999999999609, 2.500000000000000000, -0.6928203230275501445 ) ) ;
#14916 = FACE_BOUND ( 'NONE', #34306, .T. ) ;
#14917 = CARTESIAN_POINT ( 'NONE',  ( -0.8500000000000390576, 12.50000000000000000, -6.495190528383302464 ) ) ;
#14918 = CARTESIAN_POINT ( 'NONE',  ( 7.099999999999926814, 2.500000000000000000, -0.6928203230275541413 ) ) ;
#14919 = DIRECTION ( 'NONE',  ( 0.000000000000000000, 1.000000000000000000, 0.000000000000000000 ) ) ;
#14920 = AXIS2_PLACEMENT_3D ( 'NONE', #30113, #41860, #109951 ) ;
#14921 = CIRCLE ( 'NONE', #117423, 0.06509327318403745899 ) ;
#14923 = CONICAL_SURFACE ( 'NONE', #50544, 0.1000000000000002554, 0.003490658503988666988 ) ;
#14922 = CARTESIAN_POINT ( 'NONE',  ( 186.5885416670080872, -6.551208109652273848, -3.782341765625003571 ) ) ;
#14924 = DIRECTION ( 'NONE',  ( 0.000000000000000000, 0.000000000000000000, 1.000000000000000000 ) ) ;
#14925 = CARTESIAN_POINT ( 'NONE',  ( -1.050000000000038236, 12.50000000000000000, -6.148780366869526226 ) ) ;
#14926 = ORIENTED_EDGE ( 'NONE', *, *, #120422, .F. ) ;
#14927 = DIRECTION ( 'NONE',  ( 0.000000000000000000, 0.000000000000000000, 1.000000000000000000 ) ) ;
#14929 = EDGE_CURVE ( 'NONE', #48260, #79022, #128318, .T. ) ;
#14928 = AXIS2_PLACEMENT_3D ( 'NONE', #116263, #43697, #94060 ) ;
#14930 = ORIENTED_EDGE ( 'NONE', *, *, #99140, .F. ) ;
#14931 = EDGE_LOOP ( 'NONE', ( #118999, #104730, #51864, #56684 ) ) ;
#14932 = EDGE_LOOP ( 'NONE', ( #114353, #114710, #47308, #38871 ) ) ;
#14933 = ORIENTED_EDGE ( 'NONE', *, *, #110387, .F. ) ;
#14934 = CIRCLE ( 'NONE', #127837, 0.1000000000000002554 ) ;
#14935 = CARTESIAN_POINT ( 'NONE',  ( -8.350000000000012079, 2.500000000000000000, 2.757883832488649656 ) ) ;
#14936 = FACE_BOUND ( 'NONE', #77908, .T. ) ;
#14937 = DIRECTION ( 'NONE',  ( 0.000000000000000000, -0.9999939076577903929, 0.003490651415223739937 ) ) ;
#14938 = ADVANCED_FACE ( 'NONE', ( #88349 ), #26876, .T. ) ;
#14939 = ORIENTED_EDGE ( 'NONE', *, *, #32757, .T. ) ;
#14940 = ADVANCED_FACE ( 'NONE', ( #86429 ), #70453, .T. ) ;
#14941 = CARTESIAN_POINT ( 'NONE',  ( 48.83465639036802486, 3.619824997320591820, 4.313881469043760575 ) ) ;
#14942 = ADVANCED_FACE ( 'NONE', ( #79213 ), #45334, .T. ) ;
#14943 = CARTESIAN_POINT ( 'NONE',  ( -11.44999999999999751, 12.50000000000000000, -6.841600689897074261 ) ) ;
#14944 = ADVANCED_FACE ( 'NONE', ( #49113 ), #30764, .T. ) ;
#14945 = EDGE_CURVE ( 'NONE', #92060, #3076, #118466, .T. ) ;
#14946 = EDGE_LOOP ( 'NONE', ( #57425, #15279 ) ) ;
#14947 = DIRECTION ( 'NONE',  ( 0.000000000000000000, -0.000000000000000000, 1.000000000000000000 ) ) ;
#14948 = DIRECTION ( 'NONE',  ( 0.000000000000000000, 0.000000000000000000, 1.000000000000000000 ) ) ;
#14949 = ADVANCED_FACE ( 'NONE', ( #89025 ), #114263, .T. ) ;
#14950 = ORIENTED_EDGE ( 'NONE', *, *, #45039, .T. ) ;
#14951 = FACE_OUTER_BOUND ( 'NONE', #48685, .T. ) ;
#14952 = ADVANCED_FACE ( 'NONE', ( #77894 ), #47465, .T. ) ;
#14953 = DIRECTION ( 'NONE',  ( -0.000000000000000000, -1.000000000000000000, -0.000000000000000000 ) ) ;
#14954 = CIRCLE ( 'NONE', #58824, 0.06509327318403745899 ) ;
#14956 = ADVANCED_FACE ( 'NONE', ( #68079 ), #49536, .T. ) ;
#14955 = CONICAL_SURFACE ( 'NONE', #25434, 0.1000000000000000472, 0.003490658503988666988 ) ;
#14957 = EDGE_LOOP ( 'NONE', ( #80212, #110968 ) ) ;
#14958 = FACE_OUTER_BOUND ( 'NONE', #72790, .T. ) ;
#14959 = EDGE_CURVE ( 'NONE', #9531, #34777, #78791, .T. ) ;
#14960 = DIRECTION ( 'NONE',  ( 0.000000000000000000, 0.000000000000000000, -1.000000000000000000 ) ) ;
#14961 = CARTESIAN_POINT ( 'NONE',  ( 14.54999999999989591, 2.500000000000000000, 2.065063509461097624 ) ) ;
#14962 = ORIENTED_EDGE ( 'NONE', *, *, #38950, .F. ) ;
#14963 = VERTEX_POINT ( 'NONE', #60849 ) ;
#14964 = DIRECTION ( 'NONE',  ( 0.000000000000000000, 1.000000000000000000, 0.000000000000000000 ) ) ;
#14966 = EDGE_CURVE ( 'NONE', #12831, #99549, #110588, .T. ) ;
#14965 = CONICAL_SURFACE ( 'NONE', #79757, 0.1000000000000002554, 0.003490658503988666988 ) ;
#14967 = VERTEX_POINT ( 'NONE', #30121 ) ;
#14968 = PLANE ( 'NONE',  #63728 ) ;
#14969 = CONICAL_SURFACE ( 'NONE', #96552, 0.09999999999999982514, 0.003490658503988666988 ) ;
#14970 = DIRECTION ( 'NONE',  ( -0.000000000000000000, 1.000000000000000000, -0.000000000000000000 ) ) ;
#14971 = CONICAL_SURFACE ( 'NONE', #121606, 0.09999999999999982514, 0.003490658503988666988 ) ;
#14972 = ORIENTED_EDGE ( 'NONE', *, *, #106059, .T. ) ;
#14973 = VECTOR ( 'NONE', #50191, 1000.000000000000000 ) ;
#14974 = AXIS2_PLACEMENT_3D ( 'NONE', #25616, #74737, #83276 ) ;
#14975 = CARTESIAN_POINT ( 'NONE',  ( 108.3418390382325924, 5.855766388782937426, -5.000000000000004441 ) ) ;
#14976 = DIRECTION ( 'NONE',  ( 0.000000000000000000, 0.000000000000000000, -1.000000000000000000 ) ) ;
#14977 = DIRECTION ( 'NONE',  ( 0.000000000000000000, 1.000000000000000000, 0.000000000000000000 ) ) ;
#14978 =( BOUNDED_SURFACE ( )  B_SPLINE_SURFACE ( 3, 2, ( 
 ( #119151, #37385, #58318 ),
 ( #127051, #76653, #116563 ),
 ( #77291, #117183, #98214 ),
 ( #89054, #17712, #70056 ) ),
 .UNSPECIFIED., .F., .F., .F. ) 
 B_SPLINE_SURFACE_WITH_KNOTS ( ( 4, 4 ),
 ( 3, 3 ),
 ( 0.02228103309872373275, 0.02393870366795243856 ),
 ( 0.000000000000000000, 1.000000000000000000 ),
 .UNSPECIFIED. ) 
 GEOMETRIC_REPRESENTATION_ITEM ( )  RATIONAL_B_SPLINE_SURFACE ( (
 ( 1.000000000000000000, 0.9066952437723005964, 1.000000000000000000),
 ( 1.000000000000000000, 0.9065452688549086036, 1.000000000000000000),
 ( 1.000000000000000000, 0.9065452844449171099, 1.000000000000000000),
 ( 1.000000000000000000, 0.9066952434955798390, 1.000000000000000000) ) ) 
 REPRESENTATION_ITEM ( '' )  SURFACE ( )  );
#14979 = CARTESIAN_POINT ( 'NONE',  ( 9.999999999999911182, 2.500000000000000000, 5.122947341949749323 ) ) ;
#14980 = CARTESIAN_POINT ( 'NONE',  ( -7.950000000000012612, 12.50000000000000000, 2.165063509461097713 ) ) ;
#14981 = AXIS2_PLACEMENT_3D ( 'NONE', #101875, #21373, #63236 ) ;
#14982 = ORIENTED_EDGE ( 'NONE', *, *, #56022, .F. ) ;
#14983 = PRODUCT_DEFINITION_FORMATION_WITH_SPECIFIED_SOURCE ( 'ANY', '', #38744, .NOT_KNOWN. ) ;
#14984 = AXIS2_PLACEMENT_3D ( 'NONE', #87230, #78741, #36870 ) ;
#14985 = ORIENTED_EDGE ( 'NONE', *, *, #121339, .T. ) ;
#14986 = FACE_OUTER_BOUND ( 'NONE', #19590, .T. ) ;
#14988 = CONICAL_SURFACE ( 'NONE', #63139, 0.1000000000000002554, 0.003490658503988666988 ) ;
#14987 = CARTESIAN_POINT ( 'NONE',  ( -5.000000000000022204, 12.50000000000000000, -0.6277270498435166823 ) ) ;
#14989 = AXIS2_PLACEMENT_3D ( 'NONE', #125775, #44026, #65581 ) ;
#14990 = CIRCLE ( 'NONE', #42227, 0.09999999999999982514 ) ;
#14991 = CARTESIAN_POINT ( 'NONE',  ( 8.949999999999917577, 12.50000000000000000, 6.083687093685482772 ) ) ;
#14993 = ORIENTED_EDGE ( 'NONE', *, *, #55470, .T. ) ;
#14992 = ORIENTED_EDGE ( 'NONE', *, *, #82605, .T. ) ;
#14994 = ORIENTED_EDGE ( 'NONE', *, *, #74001, .T. ) ;
#14995 = DIRECTION ( 'NONE',  ( 0.000000000000000000, -0.9999939076577903929, 0.003490651415223739937 ) ) ;
#14996 = CIRCLE ( 'NONE', #79778, 0.06509327318403745899 ) ;
#14997 = LINE ( 'NONE', #95530, #65315 ) ;
#14998 = LINE ( 'NONE', #35327, #122894 ) ;
#14999 = CARTESIAN_POINT ( 'NONE',  ( 3.349999999999941025, 2.500000000000000000, 7.288010851410849256 ) ) ;
#15000 = VECTOR ( 'NONE', #111392, 1000.000000000000000 ) ;
#15001 = CARTESIAN_POINT ( 'NONE',  ( -7.700000000000016165, 2.500000000000000000, 0.4464101615137735513 ) ) ;
#15002 = CARTESIAN_POINT ( 'NONE',  ( 9.999999999999912959, 12.50000000000000000, -5.022947341949754119 ) ) ;
#15003 = DIRECTION ( 'NONE',  ( -0.000000000000000000, -1.000000000000000000, -0.000000000000000000 ) ) ;
#15004 = CARTESIAN_POINT ( 'NONE',  ( 3.149999999999946176, 2.500000000000000000, -2.511473670974877948 ) ) ;
#15005 = B_SPLINE_CURVE_WITH_KNOTS ( 'NONE', 3,
 ( #727, #60327, #58389, #47919, #89760, #88458, #90384, #38761, #29554, #117925 ),
 .UNSPECIFIED., .F., .F.,
 ( 4, 2, 2, 2, 4 ),
 ( 0.003751885956794874175, 0.02035553200375762178, 0.03695917805072037460, 0.05356282409768312047, 0.07016647014464587329 ),
 .UNSPECIFIED. ) ;
#15006 = DIRECTION ( 'NONE',  ( 0.000000000000000000, 1.000000000000000000, 0.000000000000000000 ) ) ;
#15007 = ORIENTED_EDGE ( 'NONE', *, *, #22573, .F. ) ;
#15008 = EDGE_CURVE ( 'NONE', #24288, #3310, #9812, .T. ) ;
#15009 = ADVANCED_FACE ( 'NONE', ( #99496 ), #39083, .T. ) ;
#15010 = DIRECTION ( 'NONE',  ( -0.000000000000000000, 1.000000000000000000, -0.000000000000000000 ) ) ;
#15011 = EDGE_LOOP ( 'NONE', ( #127142, #24221, #124261, #78270 ) ) ;
#15012 = ORIENTED_EDGE ( 'NONE', *, *, #35686, .F. ) ;
#15013 = DIRECTION ( 'NONE',  ( 0.000000000000000000, 0.000000000000000000, -1.000000000000000000 ) ) ;
#15014 = DIRECTION ( 'NONE',  ( 0.000000000000000000, 0.000000000000000000, -1.000000000000000000 ) ) ;
#15015 = DIRECTION ( 'NONE',  ( 0.000000000000000000, 0.000000000000000000, 1.000000000000000000 ) ) ;
#15016 = CARTESIAN_POINT ( 'NONE',  ( 129.5000000000000000, 0.000000000000000000, -6.000000000000000000 ) ) ;
#15017 = DIRECTION ( 'NONE',  ( -0.000000000000000000, 1.000000000000000000, -0.000000000000000000 ) ) ;
#15018 = DIRECTION ( 'NONE',  ( 0.000000000000000000, -0.000000000000000000, 1.000000000000000000 ) ) ;
#15019 = AXIS2_PLACEMENT_3D ( 'NONE', #14145, #103837, #84178 ) ;
#15020 = CARTESIAN_POINT ( 'NONE',  ( -6.450000000000014388, 12.50000000000000000, 6.148780366869520897 ) ) ;
#15021 = ORIENTED_EDGE ( 'NONE', *, *, #50913, .T. ) ;
#15022 = CARTESIAN_POINT ( 'NONE',  ( 4.999999999999935163, 2.500000000000000000, 0.6928203230275494784 ) ) ;
#15023 = CIRCLE ( 'NONE', #10905, 0.09999999999999982514 ) ;
#15024 = DIRECTION ( 'NONE',  ( -0.000000000000000000, -1.000000000000000000, -0.000000000000000000 ) ) ;
#15025 = ORIENTED_EDGE ( 'NONE', *, *, #3449, .F. ) ;
#15026 = CONICAL_SURFACE ( 'NONE', #90350, 0.1000000000000000056, 0.003490658503988666988 ) ;
#15027 = ORIENTED_EDGE ( 'NONE', *, *, #60916, .F. ) ;
#15028 = CIRCLE ( 'NONE', #115375, 0.06509327318403745899 ) ;
#15029 = ORIENTED_EDGE ( 'NONE', *, *, #21019, .T. ) ;
#15030 = AXIS2_PLACEMENT_3D ( 'NONE', #2946, #71036, #99857 ) ;
#15031 = AXIS2_PLACEMENT_3D ( 'NONE', #57108, #67556, #77400 ) ;
#15032 = ORIENTED_EDGE ( 'NONE', *, *, #118281, .F. ) ;
#15033 = CARTESIAN_POINT ( 'NONE',  ( 8.099999999999923261, 2.500000000000000000, -4.576537180435978236 ) ) ;
#15034 = DIRECTION ( 'NONE',  ( 0.000000000000000000, -0.000000000000000000, 1.000000000000000000 ) ) ;
#15035 = DIRECTION ( 'NONE',  ( -0.000000000000000000, 1.000000000000000000, -0.000000000000000000 ) ) ;
#15036 = DIRECTION ( 'NONE',  ( 0.000000000000000000, 0.000000000000000000, 1.000000000000000000 ) ) ;
#15037 = CARTESIAN_POINT ( 'NONE',  ( -10.40000000000000391, 2.500000000000000000, -3.537306695894645969 ) ) ;
#15038 = EDGE_LOOP ( 'NONE', ( #120793, #121108 ) ) ;
#15039 = CARTESIAN_POINT ( 'NONE',  ( 10.64999999999991331, 2.500000000000000000, -2.511473670974877948 ) ) ;
#15040 = CARTESIAN_POINT ( 'NONE',  ( 6.849999999999929479, 2.500000000000000000, -1.718653347947326049 ) ) ;
#15041 = DIRECTION ( 'NONE',  ( 0.000000000000000000, 0.000000000000000000, -1.000000000000000000 ) ) ;
#15042 = EDGE_CURVE ( 'NONE', #90838, #110412, #95486, .T. ) ;
#15043 = ORIENTED_EDGE ( 'NONE', *, *, #5543, .F. ) ;
#15044 = ORIENTED_EDGE ( 'NONE', *, *, #82837, .F. ) ;
#15045 = ORIENTED_EDGE ( 'NONE', *, *, #30758, .T. ) ;
#15046 = CARTESIAN_POINT ( 'NONE',  ( -1.450000000000035039, 2.500000000000000000, -2.511473670974877948 ) ) ;
#15047 = PLANE ( 'NONE',  #73867 ) ;
#15048 = AXIS2_PLACEMENT_3D ( 'NONE', #4918, #3013, #33128 ) ;
#15049 = DIRECTION ( 'NONE',  ( 0.000000000000000000, 1.000000000000000000, 0.000000000000000000 ) ) ;
#15051 = ORIENTED_EDGE ( 'NONE', *, *, #122780, .T. ) ;
#15050 = EDGE_CURVE ( 'NONE', #85840, #25440, #109957, .T. ) ;
#15052 = DIRECTION ( 'NONE',  ( -0.000000000000000000, -1.000000000000000000, -0.000000000000000000 ) ) ;
#15053 = LINE ( 'NONE', #65471, #1424 ) ;
#15054 = CARTESIAN_POINT ( 'NONE',  ( 184.5000000000000000, -7.430520870378829024, -1.418378131116527108 ) ) ;
#15055 = DIRECTION ( 'NONE',  ( 0.000000000000000000, 0.000000000000000000, -1.000000000000000000 ) ) ;
#15056 = EDGE_CURVE ( 'NONE', #51917, #43890, #55782, .T. ) ;
#15057 = LINE ( 'NONE', #94290, #26886 ) ;
#15058 = CIRCLE ( 'NONE', #35931, 0.06509327318403741736 ) ;
#15059 = VECTOR ( 'NONE', #93792, 1000.000000000000000 ) ;
#15060 = ORIENTED_EDGE ( 'NONE', *, *, #18086, .T. ) ;
#15061 = DIRECTION ( 'NONE',  ( 0.000000000000000000, 1.000000000000000000, 0.000000000000000000 ) ) ;
#15062 = AXIS2_PLACEMENT_3D ( 'NONE', #5559, #16022, #106352 ) ;
#15063 = ORIENTED_EDGE ( 'NONE', *, *, #30562, .F. ) ;
#15064 = ORIENTED_EDGE ( 'NONE', *, *, #78435, .T. ) ;
#15065 = ADVANCED_FACE ( 'NONE', ( #119764 ), #7738, .T. ) ;
#15066 = CARTESIAN_POINT ( 'NONE',  ( 9.349999999999919709, 2.500000000000000000, 1.918653347947321564 ) ) ;
#15067 = FACE_BOUND ( 'NONE', #47752, .T. ) ;
#15068 = DIRECTION ( 'NONE',  ( -0.000000000000000000, 1.000000000000000000, -0.000000000000000000 ) ) ;
#15070 = VECTOR ( 'NONE', #123134, 1000.000000000000000 ) ;
#15069 = CARTESIAN_POINT ( 'NONE',  ( -4.999999999999986677, 12.50000000000000000, -2.276824562219559311E-15 ) ) ;
#15072 = CARTESIAN_POINT ( 'NONE',  ( 2.699999999999946443, 2.500000000000000000, 0.3464101615137735735 ) ) ;
#15071 = CIRCLE ( 'NONE', #10875, 0.06509327318403745899 ) ;
#15073 = EDGE_LOOP ( 'NONE', ( #57311, #27207, #97407, #33798 ) ) ;
#15074 = CONICAL_SURFACE ( 'NONE', #10877, 0.09999999999999982514, 0.003490658503988666988 ) ;
#15075 = VECTOR ( 'NONE', #28897, 1000.000000000000000 ) ;
#15076 = CIRCLE ( 'NONE', #6766, 0.1000000000000002554 ) ;
#15077 = ORIENTED_EDGE ( 'NONE', *, *, #102182, .F. ) ;
#15078 = CARTESIAN_POINT ( 'NONE',  ( 7.049999999999930544, 2.500000000000000000, -6.395190528383301931 ) ) ;
#15079 = CARTESIAN_POINT ( 'NONE',  ( 5.649999999999932854, 2.500000000000000000, 2.411473670974873862 ) ) ;
#15080 = DIRECTION ( 'NONE',  ( 0.000000000000000000, -0.9999939076577903929, 0.003490651415223739937 ) ) ;
#15081 = CONICAL_SURFACE ( 'NONE', #8840, 0.1000000000000000472, 0.003490658503988666988 ) ;
#15082 = DIRECTION ( 'NONE',  ( 0.000000000000000000, 0.000000000000000000, 1.000000000000000000 ) ) ;
#15083 = ORIENTED_EDGE ( 'NONE', *, *, #74094, .F. ) ;
#15084 = DIRECTION ( 'NONE',  ( 0.000000000000000000, 0.000000000000000000, 1.000000000000000000 ) ) ;
#15085 = CARTESIAN_POINT ( 'NONE',  ( 4.349999999999937472, 2.500000000000000000, 6.741600689897071952 ) ) ;
#15086 = AXIS2_PLACEMENT_3D ( 'NONE', #105309, #33993, #25431 ) ;
#15087 = ORIENTED_EDGE ( 'NONE', *, *, #113141, .T. ) ;
#15088 = DIRECTION ( 'NONE',  ( 0.000000000000000000, 1.000000000000000000, 0.000000000000000000 ) ) ;
#15089 = VERTEX_POINT ( 'NONE', #129614 ) ;
#15090 = FACE_BOUND ( 'NONE', #83099, .T. ) ;
#15091 = CARTESIAN_POINT ( 'NONE',  ( 8.749999999999920064, 2.500000000000000000, 5.902370205355745192 ) ) ;
#15092 = EDGE_CURVE ( 'NONE', #105669, #32860, #76711, .T. ) ;
#15093 = ORIENTED_EDGE ( 'NONE', *, *, #16743, .F. ) ;
#15094 = CARTESIAN_POINT ( 'NONE',  ( -14.54999999999998472, 2.500000000000000000, 2.065063509461101621 ) ) ;
#15095 = DIRECTION ( 'NONE',  ( -0.000000000000000000, 1.000000000000000000, -0.000000000000000000 ) ) ;
#15096 = ORIENTED_EDGE ( 'NONE', *, *, #61719, .T. ) ;
#15097 = EDGE_LOOP ( 'NONE', ( #81038, #41334 ) ) ;
#15098 = EDGE_CURVE ( 'NONE', #86875, #69479, #72610, .T. ) ;
#15099 = CARTESIAN_POINT ( 'NONE',  ( 186.2968750003414584, 8.734944146203032389, 5.348610694689227483E-16 ) ) ;
#15100 = EDGE_CURVE ( 'NONE', #78428, #81254, #87249, .T. ) ;
#15101 = ORIENTED_EDGE ( 'NONE', *, *, #107527, .T. ) ;
#15102 = DIRECTION ( 'NONE',  ( 0.000000000000000000, 0.000000000000000000, 1.000000000000000000 ) ) ;
#15103 = DIRECTION ( 'NONE',  ( 0.000000000000000000, 1.000000000000000000, -1.224646799147353207E-16 ) ) ;
#15104 = AXIS2_PLACEMENT_3D ( 'NONE', #41556, #98501, #110904 ) ;
#15105 = DIRECTION ( 'NONE',  ( 0.000000000000000000, -0.9999939076577903929, 0.003490651415223739937 ) ) ;
#15106 = CARTESIAN_POINT ( 'NONE',  ( -12.04999999999999716, 2.500000000000000000, -6.495190528383298911 ) ) ;
#15107 = EDGE_CURVE ( 'NONE', #123328, #12341, #39932, .T. ) ;
#15108 = VECTOR ( 'NONE', #64787, 1000.000000000000000 ) ;
#15109 = EDGE_CURVE ( 'NONE', #21310, #79729, #21569, .T. ) ;
#15110 = CARTESIAN_POINT ( 'NONE',  ( -8.950000000000009948, 2.500000000000000000, -6.841600689897072485 ) ) ;
#15111 = CARTESIAN_POINT ( 'NONE',  ( -4.600000000000028955, 2.500000000000000000, -4.330127018922201643 ) ) ;
#15112 = EDGE_CURVE ( 'NONE', #55936, #105517, #79836, .T. ) ;
#15113 = ADVANCED_FACE ( 'NONE', ( #61511 ), #90282, .T. ) ;
#15114 = AXIS2_PLACEMENT_3D ( 'NONE', #51760, #82519, #120497 ) ;
#15116 = EDGE_LOOP ( 'NONE', ( #28966, #121107, #63819, #28717 ) ) ;
#15115 = CONICAL_SURFACE ( 'NONE', #4648, 0.1000000000000002554, 0.003490658503988666988 ) ;
#15118 = ORIENTED_EDGE ( 'NONE', *, *, #99724, .F. ) ;
#15117 = AXIS2_PLACEMENT_3D ( 'NONE', #43864, #121113, #32111 ) ;
#15119 = DIRECTION ( 'NONE',  ( 0.000000000000000000, 0.000000000000000000, 1.000000000000000000 ) ) ;
#15120 = ADVANCED_FACE ( 'NONE', ( #71973 ), #122774, .T. ) ;
#15121 = CARTESIAN_POINT ( 'NONE',  ( -12.49999999999999289, 12.50000000000000000, 3.637306695894644726 ) ) ;
#15122 = DIRECTION ( 'NONE',  ( 0.000000000000000000, -0.000000000000000000, 1.000000000000000000 ) ) ;
#15123 = AXIS2_PLACEMENT_3D ( 'NONE', #21281, #61215, #3579 ) ;
#15124 = FACE_OUTER_BOUND ( 'NONE', #8430, .T. ) ;
#15127 = EDGE_LOOP ( 'NONE', ( #69130, #40975, #12201, #29535 ) ) ;
#15126 = EDGE_LOOP ( 'NONE', ( #24841, #568, #100651, #95291 ) ) ;
#15125 = AXIS2_PLACEMENT_3D ( 'NONE', #39212, #79121, #69267 ) ;
#15128 = FACE_BOUND ( 'NONE', #96406, .T. ) ;
#15129 = VERTEX_POINT ( 'NONE', #11082 ) ;
#15130 = DIRECTION ( 'NONE',  ( -4.274815082592931898E-19, -0.9999939076577903929, -0.003490651415223739937 ) ) ;
#15131 = DIRECTION ( 'NONE',  ( 1.000000000000000000, 0.000000000000000000, -1.776356839400246520E-15 ) ) ;
#15132 = EDGE_CURVE ( 'NONE', #53696, #80576, #116212, .T. ) ;
#15133 = CIRCLE ( 'NONE', #65227, 0.09999999999999982514 ) ;
#15134 = ORIENTED_EDGE ( 'NONE', *, *, #92242, .T. ) ;
#15135 = DIRECTION ( 'NONE',  ( 0.000000000000000000, 0.000000000000000000, -1.000000000000000000 ) ) ;
#15136 = LINE ( 'NONE', #54433, #3411 ) ;
#15137 = CARTESIAN_POINT ( 'NONE',  ( 7.049999999999930544, 12.50000000000000000, -6.430097255199264339 ) ) ;
#15138 = CARTESIAN_POINT ( 'NONE',  ( 0.3999999999999563904, 2.500000000000000000, 3.537306695894645081 ) ) ;
#15139 = DIRECTION ( 'NONE',  ( 0.000000000000000000, 0.000000000000000000, 1.000000000000000000 ) ) ;
#15140 = DIRECTION ( 'NONE',  ( -0.000000000000000000, -1.000000000000000000, -0.000000000000000000 ) ) ;
#15141 = CARTESIAN_POINT ( 'NONE',  ( 4.149999999999939959, 2.500000000000000000, -6.495190528383302464 ) ) ;
#15142 = CARTESIAN_POINT ( 'NONE',  ( 1.049999999999953637, 2.500000000000000000, 2.611473670974873151 ) ) ;
#15143 = CARTESIAN_POINT ( 'NONE',  ( 8.149999999999920419, 12.50000000000000000, -2.511473670974877948 ) ) ;
#15144 = CIRCLE ( 'NONE', #61446, 0.09999999999999982514 ) ;
#15145 = ORIENTED_EDGE ( 'NONE', *, *, #21835, .T. ) ;
#15146 = VERTEX_POINT ( 'NONE', #1278 ) ;
#15147 = CARTESIAN_POINT ( 'NONE',  ( 7.099999999999926814, 2.500000000000000000, -0.7928203230275542301 ) ) ;
#15148 = ORIENTED_EDGE ( 'NONE', *, *, #110622, .T. ) ;
#15149 = CARTESIAN_POINT ( 'NONE',  ( 20.80940928220344688, 0.7000174339600965245, 4.161255421338325711 ) ) ;
#15151 = ORIENTED_EDGE ( 'NONE', *, *, #93511, .F. ) ;
#15150 = ORIENTED_EDGE ( 'NONE', *, *, #76831, .T. ) ;
#15152 = ORIENTED_EDGE ( 'NONE', *, *, #12458, .T. ) ;
#15153 = FACE_OUTER_BOUND ( 'NONE', #105076, .T. ) ;
#15154 = AXIS2_PLACEMENT_3D ( 'NONE', #89297, #48742, #70949 ) ;
#15155 = VECTOR ( 'NONE', #115245, 1000.000000000000000 ) ;
#15156 = CARTESIAN_POINT ( 'NONE',  ( 14.79999999999989413, 2.500000000000000000, -0.3464101615137782364 ) ) ;
#15157 = CARTESIAN_POINT ( 'NONE',  ( -3.750000000000025757, 2.500000000000000000, 1.372243186433545370 ) ) ;
#15158 = CARTESIAN_POINT ( 'NONE',  ( 11.24999999999990941, 2.500000000000000000, 7.288010851410849256 ) ) ;
#15159 = CARTESIAN_POINT ( 'NONE',  ( 1.899999999999951283, 12.50000000000000000, -0.3464101615137782364 ) ) ;
#15160 = EDGE_LOOP ( 'NONE', ( #99157, #30438, #126273, #51123 ) ) ;
#15161 = AXIS2_PLACEMENT_3D ( 'NONE', #124741, #15412, #85454 ) ;
#15162 = MECHANICAL_DESIGN_GEOMETRIC_PRESENTATION_REPRESENTATION (  '', ( #56927 ), #17210 ) ;
#15163 = DIRECTION ( 'NONE',  ( -0.000000000000000000, 1.000000000000000000, -0.000000000000000000 ) ) ;
#15164 = EDGE_LOOP ( 'NONE', ( #42159, #97596, #5935, #80424 ) ) ;
#15165 = CONICAL_SURFACE ( 'NONE', #59117, 0.1000000000000002554, 0.003490658503988666988 ) ;
#15166 = VERTEX_POINT ( 'NONE', #101422 ) ;
#15167 = AXIS2_PLACEMENT_3D ( 'NONE', #83968, #123895, #112806 ) ;
#15168 = ADVANCED_FACE ( 'NONE', ( #51686 ), #47567, .T. ) ;
#15169 = EDGE_LOOP ( 'NONE', ( #30768, #69915 ) ) ;
#15170 = DIRECTION ( 'NONE',  ( 0.000000000000000000, 1.000000000000000000, 0.000000000000000000 ) ) ;
#15171 = ORIENTED_EDGE ( 'NONE', *, *, #118530, .T. ) ;
#15172 = ORIENTED_EDGE ( 'NONE', *, *, #19447, .F. ) ;
#15173 = ORIENTED_EDGE ( 'NONE', *, *, #34342, .F. ) ;
#15174 = CIRCLE ( 'NONE', #61172, 0.1000000000000002554 ) ;
#15175 = DIRECTION ( 'NONE',  ( 0.000000000000000000, 0.000000000000000000, 1.000000000000000000 ) ) ;
#15176 = AXIS2_PLACEMENT_3D ( 'NONE', #55693, #5930, #66154 ) ;
#15177 = ADVANCED_FACE ( 'NONE', ( #113820 ), #28692, .T. ) ;
#15178 = CARTESIAN_POINT ( 'NONE',  ( 6.849999999999929479, 2.500000000000000000, -1.818653347947326138 ) ) ;
#15179 = CARTESIAN_POINT ( 'NONE',  ( 9.599999999999914380, 2.500000000000000000, 3.537306695894645081 ) ) ;
#15180 = CARTESIAN_POINT ( 'NONE',  ( 9.599999999999914380, 12.50000000000000000, -3.637306695894650055 ) ) ;
#15181 = CIRCLE ( 'NONE', #88338, 0.06509327318403741736 ) ;
#15182 = DIRECTION ( 'NONE',  ( -0.000000000000000000, 1.000000000000000000, -0.000000000000000000 ) ) ;
#15183 = AXIS2_PLACEMENT_3D ( 'NONE', #42267, #1673, #69279 ) ;
#15184 = DIRECTION ( 'NONE',  ( 0.000000000000000000, 0.000000000000000000, 1.000000000000000000 ) ) ;
#15185 = ORIENTED_EDGE ( 'NONE', *, *, #12195, .F. ) ;
#15186 = AXIS2_PLACEMENT_3D ( 'NONE', #3230, #54257, #112545 ) ;
#15187 = DIRECTION ( 'NONE',  ( 0.000000000000000000, 0.000000000000000000, 1.000000000000000000 ) ) ;
#15188 = EDGE_LOOP ( 'NONE', ( #95930, #9057 ) ) ;
#15189 = LINE ( 'NONE', #66239, #96540 ) ;
#15190 = ORIENTED_EDGE ( 'NONE', *, *, #88462, .F. ) ;
#15191 = DIRECTION ( 'NONE',  ( 0.000000000000000000, 0.000000000000000000, -1.000000000000000000 ) ) ;
#15192 = VERTEX_POINT ( 'NONE', #115076 ) ;
#15193 = ORIENTED_EDGE ( 'NONE', *, *, #103053, .F. ) ;
#15194 = CARTESIAN_POINT ( 'NONE',  ( -8.749999999999971578, 12.50000000000000000, 6.495190528383297135 ) ) ;
#15195 = CARTESIAN_POINT ( 'NONE',  ( -10.00000000000000533, 2.500000000000000000, -5.022947341949749678 ) ) ;
#15196 = DIRECTION ( 'NONE',  ( 0.000000000000000000, 0.000000000000000000, 1.000000000000000000 ) ) ;
#15197 = CARTESIAN_POINT ( 'NONE',  ( -1.850000000000033840, 12.50000000000000000, 1.818653347947321475 ) ) ;
#15198 = VERTEX_POINT ( 'NONE', #24150 ) ;
#15199 = DIRECTION ( 'NONE',  ( -0.000000000000000000, 1.000000000000000000, -0.000000000000000000 ) ) ;
#15201 = AXIS2_PLACEMENT_3D ( 'NONE', #20351, #120482, #60300 ) ;
#15200 = CARTESIAN_POINT ( 'NONE',  ( 3.749999999999976907, 12.50000000000000000, 2.165063509461097713 ) ) ;
#15202 = AXIS2_PLACEMENT_3D ( 'NONE', #49062, #38601, #16334 ) ;
#15203 = CARTESIAN_POINT ( 'NONE',  ( 0.7999999999999548583, 2.500000000000000000, 4.230127018922196669 ) ) ;
#15204 = CARTESIAN_POINT ( 'NONE',  ( -1.850000000000033840, 12.50000000000000000, 6.841600689897072485 ) ) ;
#15205 = CARTESIAN_POINT ( 'NONE',  ( -0.8500000000000382805, 2.500000000000000000, -1.572243186433550211 ) ) ;
#15206 = ADVANCED_FACE ( 'NONE', ( #104625 ), #16135, .T. ) ;
#15207 = EDGE_LOOP ( 'NONE', ( #71, #111091, #100800, #90692 ) ) ;
#15208 = CIRCLE ( 'NONE', #8860, 0.06509327318403745899 ) ;
#15209 = ORIENTED_EDGE ( 'NONE', *, *, #117889, .T. ) ;
#15210 = AXIS2_PLACEMENT_3D ( 'NONE', #56843, #125592, #96775 ) ;
#15211 = CIRCLE ( 'NONE', #84282, 0.06509327318403745899 ) ;
#15212 = ORIENTED_EDGE ( 'NONE', *, *, #94242, .F. ) ;
#15213 = CARTESIAN_POINT ( 'NONE',  ( -2.499999999999996003, 2.500000000000000000, -4.330127018922201643 ) ) ;
#15215 = EDGE_CURVE ( 'NONE', #50751, #100973, #120716, .T. ) ;
#15214 = LINE ( 'NONE', #85900, #35589 ) ;
#15216 = AXIS2_PLACEMENT_3D ( 'NONE', #67332, #28749, #17614 ) ;
#15217 = AXIS2_PLACEMENT_3D ( 'NONE', #26675, #66587, #16183 ) ;
#15218 = CIRCLE ( 'NONE', #63265, 0.06509327318403745899 ) ;
#15219 = AXIS2_PLACEMENT_3D ( 'NONE', #88237, #19519, #9052 ) ;
#15220 = ADVANCED_FACE ( 'NONE', ( #105286 ), #9612, .T. ) ;
#15221 = CARTESIAN_POINT ( 'NONE',  ( 184.6718750003414016, 9.264065473108010111E-16, -7.564683531250000925 ) ) ;
#15222 = CARTESIAN_POINT ( 'NONE',  ( -5.000000000000026645, 2.500000000000000000, -3.537306695894649966 ) ) ;
#15223 = DIRECTION ( 'NONE',  ( 0.000000000000000000, 1.000000000000000000, 0.000000000000000000 ) ) ;
#15224 = CARTESIAN_POINT ( 'NONE',  ( -3.100000000000028511, 12.50000000000000000, -4.676537180435977881 ) ) ;
#15225 = EDGE_CURVE ( 'NONE', #40372, #127950, #76806, .T. ) ;
#15226 = FACE_OUTER_BOUND ( 'NONE', #39324, .T. ) ;
#15227 = ORIENTED_EDGE ( 'NONE', *, *, #73936, .F. ) ;
#15228 = CONICAL_SURFACE ( 'NONE', #69527, 0.09999999999999982514, 0.003490658503988666988 ) ;
#15229 = LINE ( 'NONE', #47301, #48522 ) ;
#15230 = DIRECTION ( 'NONE',  ( -4.274815082592931898E-19, -0.9999939076577903929, -0.003490651415223739937 ) ) ;
#15231 = ADVANCED_FACE ( 'NONE', ( #3853 ), #57938, .T. ) ;
#15232 = ORIENTED_EDGE ( 'NONE', *, *, #122870, .T. ) ;
#15233 = ADVANCED_FACE ( 'NONE', ( #84985 ), #53817, .T. ) ;
#15234 = DIRECTION ( 'NONE',  ( 0.000000000000000000, 1.000000000000000000, 0.000000000000000000 ) ) ;
#15235 = LINE ( 'NONE', #112179, #94985 ) ;
#15236 = CIRCLE ( 'NONE', #32006, 0.06509327318403745899 ) ;
#15237 = ORIENTED_EDGE ( 'NONE', *, *, #99515, .F. ) ;
#15238 = DIRECTION ( 'NONE',  ( 0.000000000000000000, 0.000000000000000000, -1.000000000000000000 ) ) ;
#15239 = ORIENTED_EDGE ( 'NONE', *, *, #53878, .F. ) ;
#15240 = DIRECTION ( 'NONE',  ( -0.000000000000000000, -1.000000000000000000, -0.000000000000000000 ) ) ;
#15241 = CARTESIAN_POINT ( 'NONE',  ( -1.650000000000034772, 2.500000000000000000, 1.472243186433545459 ) ) ;
#15242 = CARTESIAN_POINT ( 'NONE',  ( -4.350000000000027178, 2.500000000000000000, -6.941600689897077459 ) ) ;
#15243 = AXIS2_PLACEMENT_3D ( 'NONE', #86560, #26370, #17142 ) ;
#15244 = VERTEX_POINT ( 'NONE', #4473 ) ;
#15245 = CONICAL_SURFACE ( 'NONE', #117647, 0.09999999999999999167, 0.003490658503988666988 ) ;
#15246 = DIRECTION ( 'NONE',  ( 0.000000000000000000, 0.000000000000000000, -1.000000000000000000 ) ) ;
#15247 = DIRECTION ( 'NONE',  ( -0.000000000000000000, 1.000000000000000000, -0.000000000000000000 ) ) ;
#15248 = AXIS2_PLACEMENT_3D ( 'NONE', #17681, #26233, #106076 ) ;
#15249 = VERTEX_POINT ( 'NONE', #43165 ) ;
#15250 = VECTOR ( 'NONE', #83001, 1000.000000000000000 ) ;
#15251 = DIRECTION ( 'NONE',  ( -4.274815082592931898E-19, -0.9999939076577903929, -0.003490651415223739937 ) ) ;
#15252 = CONICAL_SURFACE ( 'NONE', #88433, 0.1000000000000002554, 0.003490658503988666988 ) ;
#15253 = ORIENTED_EDGE ( 'NONE', *, *, #113422, .F. ) ;
#15254 = ORIENTED_EDGE ( 'NONE', *, *, #42005, .T. ) ;
#15255 = DIRECTION ( 'NONE',  ( 0.000000000000000000, 0.000000000000000000, 1.000000000000000000 ) ) ;
#15256 = DIRECTION ( 'NONE',  ( 0.000000000000000000, -0.9999939076577903929, 0.003490651415223739937 ) ) ;
#15257 = VERTEX_POINT ( 'NONE', #35897 ) ;
#15258 = DIRECTION ( 'NONE',  ( -0.000000000000000000, 1.000000000000000000, -0.000000000000000000 ) ) ;
#15259 = CARTESIAN_POINT ( 'NONE',  ( -12.69999999999999396, 2.500000000000000000, 0.3464101615137776813 ) ) ;
#15260 = AXIS2_PLACEMENT_3D ( 'NONE', #45717, #105920, #26713 ) ;
#15261 = ORIENTED_EDGE ( 'NONE', *, *, #41673, .T. ) ;
#15262 = ADVANCED_FACE ( 'NONE', ( #94817 ), #20373, .T. ) ;
#15263 = FACE_OUTER_BOUND ( 'NONE', #108302, .T. ) ;
#15264 = CARTESIAN_POINT ( 'NONE',  ( 1.049999999999953637, 2.500000000000000000, 2.411473670974873862 ) ) ;
#15265 = CIRCLE ( 'NONE', #25664, 0.1000000000000000472 ) ;
#15266 = CIRCLE ( 'NONE', #57152, 0.06509327318403745899 ) ;
#15267 = AXIS2_PLACEMENT_3D ( 'NONE', #52854, #41121, #70551 ) ;
#15268 = EDGE_CURVE ( 'NONE', #111073, #80386, #103362, .T. ) ;
#15269 = CARTESIAN_POINT ( 'NONE',  ( -9.600000000000008527, 2.500000000000000000, -2.385244779468109755E-15 ) ) ;
#15270 = CARTESIAN_POINT ( 'NONE',  ( -14.39999999999998614, 2.500000000000000000, 0.3464101615137758494 ) ) ;
#15271 = EDGE_CURVE ( 'NONE', #57444, #51769, #93529, .T. ) ;
#15272 = DIRECTION ( 'NONE',  ( 0.000000000000000000, 0.000000000000000000, -1.000000000000000000 ) ) ;
#15273 = AXIS2_PLACEMENT_3D ( 'NONE', #100608, #98675, #69879 ) ;
#15274 = CARTESIAN_POINT ( 'NONE',  ( -2.500000000000030642, 12.50000000000000000, -0.6928203230275541413 ) ) ;
#15275 = EDGE_CURVE ( 'NONE', #120157, #43219, #62792, .T. ) ;
#15276 = EDGE_CURVE ( 'NONE', #46240, #124608, #78877, .T. ) ;
#15277 = ORIENTED_EDGE ( 'NONE', *, *, #85786, .F. ) ;
#15278 = CIRCLE ( 'NONE', #105186, 0.1000000000000002554 ) ;
#15279 = ORIENTED_EDGE ( 'NONE', *, *, #70280, .T. ) ;
#15281 = ORIENTED_EDGE ( 'NONE', *, *, #23589, .T. ) ;
#15280 = ADVANCED_FACE ( 'NONE', ( #124924 ), #49631, .T. ) ;
#15282 = EDGE_LOOP ( 'NONE', ( #56569, #6183 ) ) ;
#15283 = LINE ( 'NONE', #74877, #120630 ) ;
#15284 = DIRECTION ( 'NONE',  ( 0.000000000000000000, -0.000000000000000000, 1.000000000000000000 ) ) ;
#15285 = LINE ( 'NONE', #25770, #44741 ) ;
#15286 = VERTEX_POINT ( 'NONE', #34632 ) ;
#15287 = FACE_BOUND ( 'NONE', #95974, .T. ) ;
#15288 = CARTESIAN_POINT ( 'NONE',  ( 11.64999999999990798, 2.500000000000000000, -1.372243186433550033 ) ) ;
#15289 = FACE_OUTER_BOUND ( 'NONE', #97125, .T. ) ;
#15290 = ADVANCED_FACE ( 'NONE', ( #125553 ), #13666, .T. ) ;
#15291 = DIRECTION ( 'NONE',  ( 0.000000000000000000, -0.000000000000000000, 1.000000000000000000 ) ) ;
#15292 = EDGE_CURVE ( 'NONE', #40372, #96407, #3226, .T. ) ;
#15293 = DIRECTION ( 'NONE',  ( 0.000000000000000000, 0.000000000000000000, -1.000000000000000000 ) ) ;
#15294 = CARTESIAN_POINT ( 'NONE',  ( -9.400000000000007461, 12.50000000000000000, -0.2813168883297409439 ) ) ;
#15295 = DIRECTION ( 'NONE',  ( 0.000000000000000000, 1.000000000000000000, 0.000000000000000000 ) ) ;
#15296 = CARTESIAN_POINT ( 'NONE',  ( -12.29999999999999538, 2.500000000000000000, -0.3464101615137741841 ) ) ;
#15297 = DIRECTION ( 'NONE',  ( 0.000000000000000000, 0.000000000000000000, 1.000000000000000000 ) ) ;
#15298 = CIRCLE ( 'NONE', #2799, 0.06509327318403745899 ) ;
#15299 = DIRECTION ( 'NONE',  ( 0.000000000000000000, 1.000000000000000000, 0.000000000000000000 ) ) ;
#15300 = CARTESIAN_POINT ( 'NONE',  ( 1.649999999999951950, 2.500000000000000000, -7.188010851410854052 ) ) ;
#15301 = AXIS2_PLACEMENT_3D ( 'NONE', #126004, #38963, #118774 ) ;
#15302 = ORIENTED_EDGE ( 'NONE', *, *, #34273, .T. ) ;
#15303 = EDGE_LOOP ( 'NONE', ( #56884, #81256, #73255, #99373 ) ) ;
#15304 = ORIENTED_EDGE ( 'NONE', *, *, #26978, .F. ) ;
#15305 = ORIENTED_EDGE ( 'NONE', *, *, #27110, .F. ) ;
#15307 = CONICAL_SURFACE ( 'NONE', #38326, 0.09999999999999982514, 0.003490658503988666988 ) ;
#15306 = DIRECTION ( 'NONE',  ( 0.000000000000000000, 0.000000000000000000, 1.000000000000000000 ) ) ;
#15308 = EDGE_LOOP ( 'NONE', ( #54296, #93829, #36769, #124835 ) ) ;
#15309 = CIRCLE ( 'NONE', #121833, 0.06509327318403745899 ) ;
#15310 = DIRECTION ( 'NONE',  ( 0.000000000000000000, 0.000000000000000000, -1.000000000000000000 ) ) ;
#15311 = EDGE_LOOP ( 'NONE', ( #97665, #24979, #41018, #117569 ) ) ;
#15312 = EDGE_CURVE ( 'NONE', #69366, #60185, #112315, .T. ) ;
#15313 = EDGE_LOOP ( 'NONE', ( #85251, #17848, #51457, #1203 ) ) ;
#15314 = FACE_OUTER_BOUND ( 'NONE', #78462, .T. ) ;
#15315 = CIRCLE ( 'NONE', #11213, 0.06509327318403741736 ) ;
#15316 = CIRCLE ( 'NONE', #38334, 0.09999999999999982514 ) ;
#15317 = AXIS2_PLACEMENT_3D ( 'NONE', #61835, #32391, #33649 ) ;
#15318 = CARTESIAN_POINT ( 'NONE',  ( 7.099999999999926814, 2.500000000000000000, -0.6928203230275541413 ) ) ;
#15319 = DIRECTION ( 'NONE',  ( 0.000000000000000000, 0.000000000000000000, -1.000000000000000000 ) ) ;
#15320 = DIRECTION ( 'NONE',  ( -0.000000000000000000, 1.000000000000000000, -0.000000000000000000 ) ) ;
#15321 = CIRCLE ( 'NONE', #82247, 0.06509327318403745899 ) ;
#15322 = DIRECTION ( 'NONE',  ( 0.000000000000000000, -0.000000000000000000, 1.000000000000000000 ) ) ;
#15323 = CONICAL_SURFACE ( 'NONE', #57099, 0.1000000000000002554, 0.003490658503988666988 ) ;
#15324 = ORIENTED_EDGE ( 'NONE', *, *, #121060, .F. ) ;
#15325 = ORIENTED_EDGE ( 'NONE', *, *, #89636, .F. ) ;
#15326 = ORIENTED_EDGE ( 'NONE', *, *, #41302, .T. ) ;
#15328 = VERTEX_POINT ( 'NONE', #74534 ) ;
#15327 = DIRECTION ( 'NONE',  ( 0.000000000000000000, 1.000000000000000000, 0.000000000000000000 ) ) ;
#15329 = CARTESIAN_POINT ( 'NONE',  ( 7.499999999999925393, 2.500000000000000000, -3.637306695894650055 ) ) ;
#15330 = ORIENTED_EDGE ( 'NONE', *, *, #3427, .T. ) ;
#15331 = ORIENTED_EDGE ( 'NONE', *, *, #60760, .T. ) ;
#15332 = CIRCLE ( 'NONE', #88501, 0.06509327318403745899 ) ;
#15333 = DIRECTION ( 'NONE',  ( 0.000000000000000000, -0.9999939076577903929, 0.003490651415223739937 ) ) ;
#15334 = EDGE_CURVE ( 'NONE', #99444, #80386, #72608, .T. ) ;
#15335 = CARTESIAN_POINT ( 'NONE',  ( -4.200000000000025935, 2.500000000000000000, 4.430127018922196847 ) ) ;
#15336 = DIRECTION ( 'NONE',  ( 0.000000000000000000, 0.000000000000000000, 1.000000000000000000 ) ) ;
#15337 = PLANE ( 'NONE',  #100624 ) ;
#15338 = PLANE ( 'NONE',  #50370 ) ;
#15340 = EDGE_LOOP ( 'NONE', ( #23330, #24525, #121737, #113567 ) ) ;
#15339 = CONICAL_SURFACE ( 'NONE', #111500, 0.1000000000000002554, 0.003490658503988666988 ) ;
#15341 = CARTESIAN_POINT ( 'NONE',  ( -1.450000000000036371, 2.500000000000000000, 6.741600689897071952 ) ) ;
#15342 = AXIS2_PLACEMENT_3D ( 'NONE', #101595, #49938, #89831 ) ;
#15343 = AXIS2_PLACEMENT_3D ( 'NONE', #87380, #27821, #38977 ) ;
#15344 = VERTEX_POINT ( 'NONE', #18827 ) ;
#15345 = FACE_OUTER_BOUND ( 'NONE', #2121, .T. ) ;
#15346 = EDGE_LOOP ( 'NONE', ( #60463, #50607, #74559, #69992 ) ) ;
#15347 = DIRECTION ( 'NONE',  ( 1.000000000000000000, -0.000000000000000000, -0.000000000000000000 ) ) ;
#15348 = DIRECTION ( 'NONE',  ( 0.000000000000000000, 1.000000000000000000, 0.000000000000000000 ) ) ;
#15349 = CARTESIAN_POINT ( 'NONE',  ( -3.350000000000028955, 2.500000000000000000, 7.288010851410849256 ) ) ;
#15350 = LINE ( 'NONE', #62557, #58483 ) ;
#15351 = ORIENTED_EDGE ( 'NONE', *, *, #105276, .T. ) ;
#15352 = CIRCLE ( 'NONE', #84328, 0.09999999999999982514 ) ;
#15353 = AXIS2_PLACEMENT_3D ( 'NONE', #8877, #96609, #9550 ) ;
#15354 = CARTESIAN_POINT ( 'NONE',  ( -4.400000000000025224, 2.500000000000000000, -0.3464101615137783474 ) ) ;
#15355 = VECTOR ( 'NONE', #79020, 1000.000000000000000 ) ;
#15356 = DIRECTION ( 'NONE',  ( 0.000000000000000000, 0.000000000000000000, -1.000000000000000000 ) ) ;
#15357 = ORIENTED_EDGE ( 'NONE', *, *, #34308, .F. ) ;
#15358 = VERTEX_POINT ( 'NONE', #58762 ) ;
#15359 = VERTEX_POINT ( 'NONE', #39149 ) ;
#15360 = CARTESIAN_POINT ( 'NONE',  ( 9.599999999999914380, 2.500000000000000000, -4.922947341949753586 ) ) ;
#15361 = DIRECTION ( 'NONE',  ( 0.000000000000000000, 0.000000000000000000, 1.000000000000000000 ) ) ;
#15362 = CARTESIAN_POINT ( 'NONE',  ( 185.4010416670080588, -4.367472073101519747, 7.564683531249999149 ) ) ;
#15363 = AXIS2_PLACEMENT_3D ( 'NONE', #105801, #44956, #84865 ) ;
#15364 = FACE_OUTER_BOUND ( 'NONE', #107830, .T. ) ;
#15365 = DIRECTION ( 'NONE',  ( 0.000000000000000000, 1.000000000000000000, 0.000000000000000000 ) ) ;
#15366 = CIRCLE ( 'NONE', #4908, 0.1000000000000002554 ) ;
#15367 = CIRCLE ( 'NONE', #52960, 0.1000000000000002554 ) ;
#15368 = AXIS2_PLACEMENT_3D ( 'NONE', #73768, #96002, #115623 ) ;
#15369 = DIRECTION ( 'NONE',  ( 0.000000000000000000, 0.000000000000000000, 1.000000000000000000 ) ) ;
#15370 = AXIS2_PLACEMENT_3D ( 'NONE', #58626, #39647, #120115 ) ;
#15371 = ORIENTED_EDGE ( 'NONE', *, *, #106319, .T. ) ;
#15372 = AXIS2_PLACEMENT_3D ( 'NONE', #3535, #76148, #26412 ) ;
#15373 = CARTESIAN_POINT ( 'NONE',  ( -12.49999999999999289, 2.500000000000000000, -5.022947341949751454 ) ) ;
#15374 = ADVANCED_FACE ( 'NONE', ( #48296 ), #126980, .T. ) ;
#15375 = ORIENTED_EDGE ( 'NONE', *, *, #125426, .F. ) ;
#15376 = EDGE_CURVE ( 'NONE', #48300, #107800, #14088, .T. ) ;
#15377 = DIRECTION ( 'NONE',  ( 0.000000000000000000, -0.9999939076577903929, 0.003490651415223739937 ) ) ;
#15378 = DIRECTION ( 'NONE',  ( 0.000000000000000000, 1.000000000000000000, 0.000000000000000000 ) ) ;
#15379 = DIRECTION ( 'NONE',  ( 0.000000000000000000, 1.000000000000000000, 0.000000000000000000 ) ) ;
#15380 = EDGE_CURVE ( 'NONE', #96527, #117477, #3356, .T. ) ;
#15381 = ORIENTED_EDGE ( 'NONE', *, *, #70847, .T. ) ;
#15382 = DIRECTION ( 'NONE',  ( 0.000000000000000000, 1.000000000000000000, 0.000000000000000000 ) ) ;
#15383 = DIRECTION ( 'NONE',  ( 0.000000000000000000, 0.000000000000000000, -1.000000000000000000 ) ) ;
#15384 = EDGE_CURVE ( 'NONE', #119064, #124197, #91376, .T. ) ;
#15385 = EDGE_CURVE ( 'NONE', #84066, #41827, #26723, .T. ) ;
#15386 = CONICAL_SURFACE ( 'NONE', #7068, 0.09999999999999982514, 0.003490658503988666988 ) ;
#15387 = CIRCLE ( 'NONE', #27930, 0.06509327318403745899 ) ;
#15388 = ADVANCED_FACE ( 'NONE', ( #46348 ), #97439, .T. ) ;
#15389 = EDGE_CURVE ( 'NONE', #69025, #56716, #41033, .T. ) ;
#15390 = EDGE_LOOP ( 'NONE', ( #38042, #68883, #117598, #127860 ) ) ;
#15391 = DIRECTION ( 'NONE',  ( 0.000000000000000000, 0.000000000000000000, 1.000000000000000000 ) ) ;
#15392 = AXIS2_PLACEMENT_3D ( 'NONE', #13962, #5432, #114109 ) ;
#15393 = AXIS2_PLACEMENT_3D ( 'NONE', #124211, #70758, #114378 ) ;
#15394 = ORIENTED_EDGE ( 'NONE', *, *, #42028, .F. ) ;
#15395 = ORIENTED_EDGE ( 'NONE', *, *, #86931, .F. ) ;
#15396 = DIRECTION ( 'NONE',  ( -0.000000000000000000, 1.000000000000000000, -0.000000000000000000 ) ) ;
#15397 = CIRCLE ( 'NONE', #50943, 0.06509327318403745899 ) ;
#15398 = VECTOR ( 'NONE', #10687, 1000.000000000000000 ) ;
#15399 = EDGE_CURVE ( 'NONE', #2985, #107746, #7706, .T. ) ;
#15400 = ORIENTED_EDGE ( 'NONE', *, *, #83395, .T. ) ;
#15401 = CARTESIAN_POINT ( 'NONE',  ( 17.29982614915083161, 2.489966891809608285, -2.989943721782188479 ) ) ;
#15402 = CARTESIAN_POINT ( 'NONE',  ( 179.5000000000000000, 0.000000000000000000, 0.000000000000000000 ) ) ;
#15403 = CARTESIAN_POINT ( 'NONE',  ( 4.799999999999937650, 2.500000000000000000, -0.3464101615137782364 ) ) ;
#15405 = ORIENTED_EDGE ( 'NONE', *, *, #12849, .T. ) ;
#15404 = AXIS2_PLACEMENT_3D ( 'NONE', #19601, #57599, #48410 ) ;
#15406 = AXIS2_PLACEMENT_3D ( 'NONE', #46566, #75379, #14522 ) ;
#15407 = CIRCLE ( 'NONE', #67650, 0.09999999999999982514 ) ;
#15408 = FACE_BOUND ( 'NONE', #123628, .T. ) ;
#15410 = EDGE_LOOP ( 'NONE', ( #88311, #103083, #97618, #129414 ) ) ;
#15409 = DIRECTION ( 'NONE',  ( 0.000000000000000000, 0.000000000000000000, 1.000000000000000000 ) ) ;
#15411 = AXIS2_PLACEMENT_3D ( 'NONE', #41314, #72057, #111978 ) ;
#15412 = DIRECTION ( 'NONE',  ( 0.000000000000000000, 1.000000000000000000, 0.000000000000000000 ) ) ;
#15413 = CARTESIAN_POINT ( 'NONE',  ( 1.049999999999954969, 12.50000000000000000, -6.906693963081115051 ) ) ;
#15414 = ORIENTED_EDGE ( 'NONE', *, *, #45858, .F. ) ;
#15415 = ORIENTED_EDGE ( 'NONE', *, *, #101197, .F. ) ;
#15416 = ORIENTED_EDGE ( 'NONE', *, *, #118594, .F. ) ;
#15417 = DIRECTION ( 'NONE',  ( 0.000000000000000000, 0.000000000000000000, 1.000000000000000000 ) ) ;
#15418 = CARTESIAN_POINT ( 'NONE',  ( -11.24999999999996270, 2.500000000000000000, 2.165063509461097713 ) ) ;
#15419 = CARTESIAN_POINT ( 'NONE',  ( 0.5999999999999612310, 2.500000000000000000, -0.2464101615137760659 ) ) ;
#15420 = ADVANCED_FACE ( 'NONE', ( #108493 ), #93250, .T. ) ;
#15421 = FACE_BOUND ( 'NONE', #73247, .T. ) ;
#15422 = EDGE_LOOP ( 'NONE', ( #50693, #82002 ) ) ;
#15423 = CARTESIAN_POINT ( 'NONE',  ( 185.3177083336747160, 4.367472073101515306, 7.564683531250000925 ) ) ;
#15424 = DIRECTION ( 'NONE',  ( -4.274815082592931898E-19, -0.9999939076577903929, -0.003490651415223739937 ) ) ;
#15425 = DIRECTION ( 'NONE',  ( 0.000000000000000000, 0.000000000000000000, 1.000000000000000000 ) ) ;
#15426 = CONICAL_SURFACE ( 'NONE', #65617, 0.1000000000000002554, 0.003490658503988666988 ) ;
#15427 = DIRECTION ( 'NONE',  ( 0.000000000000000000, 0.000000000000000000, 1.000000000000000000 ) ) ;
#15428 = CARTESIAN_POINT ( 'NONE',  ( 4.549999999999939426, 12.50000000000000000, -2.165063509461101710 ) ) ;
#15429 = FACE_OUTER_BOUND ( 'NONE', #121425, .T. ) ;
#15430 = ADVANCED_FACE ( 'NONE', ( #47661 ), #16860, .T. ) ;
#15431 = CARTESIAN_POINT ( 'NONE',  ( -11.89999999999999680, 2.500000000000000000, 0.3464101615137776813 ) ) ;
#15432 = DIRECTION ( 'NONE',  ( -0.000000000000000000, 1.000000000000000000, -0.000000000000000000 ) ) ;
#15433 = CONICAL_SURFACE ( 'NONE', #54870, 0.1000000000000002554, 0.003490658503988666988 ) ;
#15434 = ADVANCED_FACE ( 'NONE', ( #86919 ), #49440, .T. ) ;
#15435 = DIRECTION ( 'NONE',  ( 0.000000000000000000, 0.000000000000000000, -1.000000000000000000 ) ) ;
#15436 = ADVANCED_FACE ( 'NONE', ( #28665 ), #30569, .T. ) ;
#15437 = ORIENTED_EDGE ( 'NONE', *, *, #28941, .F. ) ;
#15438 = VERTEX_POINT ( 'NONE', #38500 ) ;
#15439 = ORIENTED_EDGE ( 'NONE', *, *, #68784, .F. ) ;
#15440 = VERTEX_POINT ( 'NONE', #107207 ) ;
#15441 = ORIENTED_EDGE ( 'NONE', *, *, #77361, .T. ) ;
#15442 = FACE_OUTER_BOUND ( 'NONE', #32424, .T. ) ;
#15443 = CARTESIAN_POINT ( 'NONE',  ( 15.79999999999989058, 2.500000000000000000, -2.385244779468109755E-15 ) ) ;
#15445 = EDGE_CURVE ( 'NONE', #20339, #37854, #86975, .T. ) ;
#15444 = ORIENTED_EDGE ( 'NONE', *, *, #100439, .F. ) ;
#15446 = FACE_BOUND ( 'NONE', #123537, .T. ) ;
#15447 = AXIS2_PLACEMENT_3D ( 'NONE', #85479, #56006, #6890 ) ;
#15448 = DIRECTION ( 'NONE',  ( 0.000000000000000000, 0.000000000000000000, 1.000000000000000000 ) ) ;
#15449 = ADVANCED_FACE ( 'NONE', ( #96100 ), #91188, .T. ) ;
#15450 = AXIS2_PLACEMENT_3D ( 'NONE', #123362, #84072, #73605 ) ;
#15451 = ADVANCED_FACE ( 'NONE', ( #58126 ), #98034, .T. ) ;
#15452 = CIRCLE ( 'NONE', #57236, 0.09999999999999982514 ) ;
#15453 = EDGE_CURVE ( 'NONE', #40839, #83875, #126699, .T. ) ;
#15454 = CARTESIAN_POINT ( 'NONE',  ( 187.5000000000000000, 0.000000000000000000, 0.000000000000000000 ) ) ;
#15455 = ORIENTED_EDGE ( 'NONE', *, *, #54293, .F. ) ;
#15456 = DIRECTION ( 'NONE',  ( -0.000000000000000000, 1.000000000000000000, -0.000000000000000000 ) ) ;
#15457 = CARTESIAN_POINT ( 'NONE',  ( 186.9583333333332860, 4.445597072760133273, 7.699999999999975309 ) ) ;
#15458 = CARTESIAN_POINT ( 'NONE',  ( 129.5000000000000000, 1.500000000000000000, -2.598076211353316900 ) ) ;
#15459 = ORIENTED_EDGE ( 'NONE', *, *, #16281, .F. ) ;
#15460 = DIRECTION ( 'NONE',  ( -0.000000000000000000, 1.000000000000000000, -0.000000000000000000 ) ) ;
#15461 = EDGE_CURVE ( 'NONE', #11368, #88940, #121528, .T. ) ;
#15462 = ORIENTED_EDGE ( 'NONE', *, *, #58466, .F. ) ;
#15463 = AXIS2_PLACEMENT_3D ( 'NONE', #76131, #34292, #116050 ) ;
#15464 = CONICAL_SURFACE ( 'NONE', #13316, 0.1000000000000000056, 0.003490658503988666988 ) ;
#15465 = AXIS2_PLACEMENT_3D ( 'NONE', #51431, #80234, #31776 ) ;
#15466 = ORIENTED_EDGE ( 'NONE', *, *, #36312, .F. ) ;
#15467 = ORIENTED_EDGE ( 'NONE', *, *, #43250, .F. ) ;
#15468 = LINE ( 'NONE', #55412, #59242 ) ;
#15469 = DIRECTION ( 'NONE',  ( 0.000000000000000000, 1.000000000000000000, 0.000000000000000000 ) ) ;
#15471 = AXIS2_PLACEMENT_3D ( 'NONE', #97730, #89841, #8056 ) ;
#15470 = CARTESIAN_POINT ( 'NONE',  ( -6.650000000000014566, 12.50000000000000000, 2.165063509461097713 ) ) ;
#15472 = ORIENTED_EDGE ( 'NONE', *, *, #69313, .T. ) ;
#15473 = CARTESIAN_POINT ( 'NONE',  ( 13.80955901302282030, 2.500000000000000444, -7.955427456728518365 ) ) ;
#15474 = CIRCLE ( 'NONE', #105375, 0.1000000000000002554 ) ;
#15475 = CARTESIAN_POINT ( 'NONE',  ( 1.449999999999952660, 2.500000000000000000, -6.741600689897078169 ) ) ;
#15476 = CARTESIAN_POINT ( 'NONE',  ( 6.849999999999929479, 12.50000000000000000, 6.148780366869520009 ) ) ;
#15477 = CARTESIAN_POINT ( 'NONE',  ( 185.3229166673494888, -4.445597072760122614, 7.699999999999998401 ) ) ;
#15478 = CARTESIAN_POINT ( 'NONE',  ( 8.549999999999924327, 2.500000000000000000, 1.818653347947321475 ) ) ;
#15479 = DIRECTION ( 'NONE',  ( -0.000000000000000000, -1.000000000000000000, -0.000000000000000000 ) ) ;
#15480 = ORIENTED_EDGE ( 'NONE', *, *, #26098, .T. ) ;
#15481 = CARTESIAN_POINT ( 'NONE',  ( -0.2000000000000399791, 2.500000000000000000, -4.676537180435977881 ) ) ;
#15482 = VERTEX_POINT ( 'NONE', #31244 ) ;
#15483 = ORIENTED_EDGE ( 'NONE', *, *, #108359, .F. ) ;
#15484 = DIRECTION ( 'NONE',  ( 0.000000000000000000, 0.000000000000000000, 1.000000000000000000 ) ) ;
#15485 = CARTESIAN_POINT ( 'NONE',  ( -6.250000000000021316, 2.500000000000000000, -5.802370205355749988 ) ) ;
#15486 = AXIS2_PLACEMENT_3D ( 'NONE', #122288, #33892, #32640 ) ;
#15487 = CONICAL_SURFACE ( 'NONE', #2991, 0.09999999999999982514, 0.003490658503988666988 ) ;
#15488 = DIRECTION ( 'NONE',  ( 0.000000000000000000, 0.000000000000000000, 1.000000000000000000 ) ) ;
#15489 = AXIS2_PLACEMENT_3D ( 'NONE', #58160, #98060, #41749 ) ;
#15490 = DIRECTION ( 'NONE',  ( -0.000000000000000000, -1.000000000000000000, -0.000000000000000000 ) ) ;
#15491 = CARTESIAN_POINT ( 'NONE',  ( -4.150000000000025224, 2.500000000000000000, 7.288010851410849256 ) ) ;
#15492 = ORIENTED_EDGE ( 'NONE', *, *, #20761, .T. ) ;
#15493 = ORIENTED_EDGE ( 'NONE', *, *, #55022, .T. ) ;
#15494 = CARTESIAN_POINT ( 'NONE',  ( 0.000000000000000000, 0.000000000000000000, -5.000000000000004441 ) ) ;
#15495 = CONICAL_SURFACE ( 'NONE', #122136, 0.1000000000000002554, 0.003490658503988666988 ) ;
#15496 = EDGE_CURVE ( 'NONE', #23794, #82143, #89506, .T. ) ;
#15497 = VECTOR ( 'NONE', #110228, 1000.000000000000000 ) ;
#15498 = CARTESIAN_POINT ( 'NONE',  ( -11.84999999999999609, 12.50000000000000000, 1.883746621131358934 ) ) ;
#15499 = DIRECTION ( 'NONE',  ( -0.000000000000000000, -1.000000000000000000, -0.000000000000000000 ) ) ;
#15500 = ORIENTED_EDGE ( 'NONE', *, *, #110002, .F. ) ;
#15501 = ORIENTED_EDGE ( 'NONE', *, *, #105579, .F. ) ;
#15502 = DIRECTION ( 'NONE',  ( 0.000000000000000000, 0.000000000000000000, -1.000000000000000000 ) ) ;
#15503 = VERTEX_POINT ( 'NONE', #19469 ) ;
#15504 = DIRECTION ( 'NONE',  ( 0.000000000000000000, 1.000000000000000000, 0.000000000000000000 ) ) ;
#15505 = AXIS2_PLACEMENT_3D ( 'NONE', #109088, #107161, #118277 ) ;
#15506 = AXIS2_PLACEMENT_3D ( 'NONE', #98111, #89593, #87003 ) ;
#15507 = CARTESIAN_POINT ( 'NONE',  ( 6.649999999999930189, 2.500000000000000000, 7.188010851410848723 ) ) ;
#15508 = VERTEX_POINT ( 'NONE', #120268 ) ;
#15509 = DIRECTION ( 'NONE',  ( -0.000000000000000000, 1.000000000000000000, -0.000000000000000000 ) ) ;
#15510 = DIRECTION ( 'NONE',  ( 0.000000000000000000, 0.000000000000000000, -1.000000000000000000 ) ) ;
#15511 = DIRECTION ( 'NONE',  ( 0.000000000000000000, 0.000000000000000000, 1.000000000000000000 ) ) ;
#15512 = AXIS2_PLACEMENT_3D ( 'NONE', #3793, #84927, #34566 ) ;
#15513 = EDGE_CURVE ( 'NONE', #90471, #55194, #38992, .T. ) ;
#15514 = DIRECTION ( 'NONE',  ( 0.000000000000000000, 1.000000000000000000, 0.000000000000000000 ) ) ;
#15515 = EDGE_LOOP ( 'NONE', ( #14678, #21355 ) ) ;
#15516 = CARTESIAN_POINT ( 'NONE',  ( 5.599999999999934808, 2.500000000000000000, -3.883716857408426648 ) ) ;
#15517 = FACE_OUTER_BOUND ( 'NONE', #37686, .T. ) ;
#15518 = ORIENTED_EDGE ( 'NONE', *, *, #45440, .T. ) ;
#15519 = ORIENTED_EDGE ( 'NONE', *, *, #15550, .F. ) ;
#15520 = CARTESIAN_POINT ( 'NONE',  ( 185.8802083336747444, 4.367472073101515306, 7.564683531250000925 ) ) ;
#15521 = CARTESIAN_POINT ( 'NONE',  ( -10.80000000000000071, 12.50000000000000000, 4.330127018922196314 ) ) ;
#15522 = CARTESIAN_POINT ( 'NONE',  ( 0.6499999999999561684, 12.50000000000000000, -2.511473670974877948 ) ) ;
#15523 = DIRECTION ( 'NONE',  ( 0.000000000000000000, 1.000000000000000000, 0.000000000000000000 ) ) ;
#15524 = AXIS2_PLACEMENT_3D ( 'NONE', #47586, #37124, #86850 ) ;
#15525 = CARTESIAN_POINT ( 'NONE',  ( 1.049999999999954525, 12.50000000000000000, 1.753560074763284016 ) ) ;
#15526 = DIRECTION ( 'NONE',  ( -0.000000000000000000, 1.000000000000000000, -0.000000000000000000 ) ) ;
#15527 = DIRECTION ( 'NONE',  ( -4.274815082592931898E-19, -0.9999939076577903929, -0.003490651415223739937 ) ) ;
#15528 = DIRECTION ( 'NONE',  ( -0.000000000000000000, -1.000000000000000000, -0.000000000000000000 ) ) ;
#15529 = CARTESIAN_POINT ( 'NONE',  ( -11.69999999999999574, 2.500000000000000000, 4.430127018922196847 ) ) ;
#15530 = DIRECTION ( 'NONE',  ( 0.000000000000000000, 1.000000000000000000, 0.000000000000000000 ) ) ;
#15532 = VECTOR ( 'NONE', #80995, 1000.000000000000000 ) ;
#15531 = CARTESIAN_POINT ( 'NONE',  ( -4.400000000000025224, 12.50000000000000000, 0.3464101615137735735 ) ) ;
#15533 = EDGE_LOOP ( 'NONE', ( #126270, #14600, #52581, #124186 ) ) ;
#15534 = CIRCLE ( 'NONE', #113848, 0.1000000000000002554 ) ;
#15535 = EDGE_CURVE ( 'NONE', #110459, #35601, #118963, .T. ) ;
#15536 = VERTEX_POINT ( 'NONE', #30608 ) ;
#15537 = ORIENTED_EDGE ( 'NONE', *, *, #82821, .F. ) ;
#15538 = CARTESIAN_POINT ( 'NONE',  ( 10.64999999999991331, 2.500000000000000000, -2.411473670974877859 ) ) ;
#15539 = CARTESIAN_POINT ( 'NONE',  ( -3.100000000000028955, 2.500000000000000000, 4.083716857408421497 ) ) ;
#15540 = ADVANCED_FACE ( 'NONE', ( #10912 ), #26444, .T. ) ;
#15541 = VERTEX_POINT ( 'NONE', #111723 ) ;
#15542 = CARTESIAN_POINT ( 'NONE',  ( -11.05000000000000249, 12.50000000000000000, -6.083687093685485436 ) ) ;
#15543 = AXIS2_PLACEMENT_3D ( 'NONE', #27164, #116180, #86062 ) ;
#15544 = LINE ( 'NONE', #22825, #122326 ) ;
#15546 = ORIENTED_EDGE ( 'NONE', *, *, #28290, .F. ) ;
#15545 = DIRECTION ( 'NONE',  ( -0.000000000000000000, -0.000000000000000000, -1.000000000000000000 ) ) ;
#15547 = EDGE_CURVE ( 'NONE', #124884, #87296, #112128, .T. ) ;
#15548 = EDGE_CURVE ( 'NONE', #35541, #14887, #124642, .T. ) ;
#15549 = ADVANCED_FACE ( 'NONE', ( #40431 ), #61341, .T. ) ;
#15550 = EDGE_CURVE ( 'NONE', #63288, #101710, #64000, .T. ) ;
#15551 = FACE_OUTER_BOUND ( 'NONE', #52146, .T. ) ;
#15552 = ORIENTED_EDGE ( 'NONE', *, *, #34939, .F. ) ;
#15553 = AXIS2_PLACEMENT_3D ( 'NONE', #43947, #44584, #15084 ) ;
#15554 = CONICAL_SURFACE ( 'NONE', #107609, 0.1000000000000002554, 0.003490658503988666988 ) ;
#15555 = ORIENTED_EDGE ( 'NONE', *, *, #125216, .F. ) ;
#15556 = ORIENTED_EDGE ( 'NONE', *, *, #73947, .T. ) ;
#15557 = VERTEX_POINT ( 'NONE', #69207 ) ;
#15558 = DIRECTION ( 'NONE',  ( 0.000000000000000000, 0.000000000000000000, -1.000000000000000000 ) ) ;
#15559 = AXIS2_PLACEMENT_3D ( 'NONE', #50556, #102874, #21101 ) ;
#15560 = EDGE_CURVE ( 'NONE', #110183, #128448, #68189, .T. ) ;
#15561 = DIRECTION ( 'NONE',  ( 0.000000000000000000, 1.000000000000000000, 0.000000000000000000 ) ) ;
#15562 = CARTESIAN_POINT ( 'NONE',  ( 127.5000000000000000, -5.000000000000000000, -4.999999999999998224 ) ) ;
#15563 = AXIS2_PLACEMENT_3D ( 'NONE', #70995, #30444, #31089 ) ;
#15564 = ADVANCED_FACE ( 'NONE', ( #92071 ), #39785, .T. ) ;
#15565 = FACE_OUTER_BOUND ( 'NONE', #103951, .T. ) ;
#15567 = ORIENTED_EDGE ( 'NONE', *, *, #58729, .T. ) ;
#15566 = EDGE_CURVE ( 'NONE', #108298, #121302, #128870, .T. ) ;
#15568 = LINE ( 'NONE', #95438, #41847 ) ;
#15569 = ORIENTED_EDGE ( 'NONE', *, *, #116488, .T. ) ;
#15570 = CARTESIAN_POINT ( 'NONE',  ( 6.249999999999967137, 2.500000000000000000, 6.495190528383297135 ) ) ;
#15571 = CARTESIAN_POINT ( 'NONE',  ( 8.949999999999915801, 2.500000000000000000, 6.741600689897071952 ) ) ;
#15572 = DIRECTION ( 'NONE',  ( -4.274815082592931898E-19, -0.9999939076577903929, -0.003490651415223739937 ) ) ;
#15573 = CARTESIAN_POINT ( 'NONE',  ( 15.24415751722998635, -2.474878586408709058, 4.460068884076466844 ) ) ;
#15574 = ORIENTED_EDGE ( 'NONE', *, *, #53512, .F. ) ;
#15575 = VECTOR ( 'NONE', #33424, 1000.000000000000000 ) ;
#15576 = VERTEX_POINT ( 'NONE', #60702 ) ;
#15577 = EDGE_LOOP ( 'NONE', ( #90002, #79765, #115077, #58619 ) ) ;
#15578 = LINE ( 'NONE', #55529, #77436 ) ;
#15580 = AXIS2_PLACEMENT_3D ( 'NONE', #65750, #84099, #25182 ) ;
#15579 = DIRECTION ( 'NONE',  ( 0.000000000000000000, 1.000000000000000000, 0.000000000000000000 ) ) ;
#15581 = CONICAL_SURFACE ( 'NONE', #19804, 0.1000000000000002554, 0.003490658503988666988 ) ;
#15582 = DIRECTION ( 'NONE',  ( 0.000000000000000000, 1.000000000000000000, 0.000000000000000000 ) ) ;
#15583 = FACE_BOUND ( 'NONE', #6587, .T. ) ;
#15584 = FACE_OUTER_BOUND ( 'NONE', #111287, .T. ) ;
#15585 = DIRECTION ( 'NONE',  ( -0.000000000000000000, -1.000000000000000000, -0.000000000000000000 ) ) ;
#15586 = CARTESIAN_POINT ( 'NONE',  ( -0.4000000000000331624, 2.500000000000000000, -0.5928203230275518321 ) ) ;
#15587 = DIRECTION ( 'NONE',  ( -0.000000000000000000, -1.000000000000000000, -0.000000000000000000 ) ) ;
#15588 = AXIS2_PLACEMENT_3D ( 'NONE', #20191, #81054, #79124 ) ;
#15589 = CIRCLE ( 'NONE', #117997, 0.09999999999999999167 ) ;
#15590 = CIRCLE ( 'NONE', #63644, 0.09999999999999982514 ) ;
#15591 = DIRECTION ( 'NONE',  ( 0.000000000000000000, 0.000000000000000000, 1.000000000000000000 ) ) ;
#15592 = CONICAL_SURFACE ( 'NONE', #124566, 0.1000000000000002554, 0.003490658503988666988 ) ;
#15593 = CARTESIAN_POINT ( 'NONE',  ( -5.450000000000023270, 12.50000000000000000, -6.495190528383302464 ) ) ;
#15594 = CARTESIAN_POINT ( 'NONE',  ( 14.14999999999989733, 12.50000000000000000, 1.407149913249508000 ) ) ;
#15595 = AXIS2_PLACEMENT_3D ( 'NONE', #82458, #22247, #41886 ) ;
#15596 = CARTESIAN_POINT ( 'NONE',  ( -2.900000000000030109, 2.500000000000000000, -3.737306695894649700 ) ) ;
#15597 = ORIENTED_EDGE ( 'NONE', *, *, #10115, .T. ) ;
#15598 = VERTEX_POINT ( 'NONE', #41077 ) ;
#15599 = ORIENTED_EDGE ( 'NONE', *, *, #84487, .T. ) ;
#15600 = ORIENTED_EDGE ( 'NONE', *, *, #71510, .F. ) ;
#15601 = CIRCLE ( 'NONE', #28140, 0.09999999999999982514 ) ;
#15602 = CARTESIAN_POINT ( 'NONE',  ( 1.649999999999951950, 2.500000000000000000, -7.088010851410853519 ) ) ;
#15603 = EDGE_CURVE ( 'NONE', #84188, #62406, #41712, .T. ) ;
#15604 = FACE_BOUND ( 'NONE', #95795, .T. ) ;
#15605 = PLANE ( 'NONE',  #22298 ) ;
#15606 = EDGE_CURVE ( 'NONE', #16422, #128537, #5487, .T. ) ;
#15607 = EDGE_CURVE ( 'NONE', #11040, #126889, #59911, .T. ) ;
#15608 = ORIENTED_EDGE ( 'NONE', *, *, #31755, .F. ) ;
#15609 = CARTESIAN_POINT ( 'NONE',  ( 35.04009662963678551, 1.562391656599548373, 4.793251516053341099 ) ) ;
#15610 = DIRECTION ( 'NONE',  ( 0.000000000000000000, 1.000000000000000000, 0.000000000000000000 ) ) ;
#15612 = ORIENTED_EDGE ( 'NONE', *, *, #46582, .T. ) ;
#15611 = AXIS2_PLACEMENT_3D ( 'NONE', #123872, #54494, #115995 ) ;
#15613 = DIRECTION ( 'NONE',  ( -0.000000000000000000, 1.000000000000000000, -0.000000000000000000 ) ) ;
#15614 = DIRECTION ( 'NONE',  ( -0.000000000000000000, 1.000000000000000000, -0.000000000000000000 ) ) ;
#15615 = EDGE_CURVE ( 'NONE', #101262, #76681, #114177, .T. ) ;
#15616 = ORIENTED_EDGE ( 'NONE', *, *, #62860, .F. ) ;
#15617 = DIRECTION ( 'NONE',  ( -0.000000000000000000, 1.000000000000000000, -0.000000000000000000 ) ) ;
#15618 = DIRECTION ( 'NONE',  ( 0.000000000000000000, -0.000000000000000000, 1.000000000000000000 ) ) ;
#15619 = AXIS2_PLACEMENT_3D ( 'NONE', #107721, #88046, #48160 ) ;
#15620 = CONICAL_SURFACE ( 'NONE', #72093, 0.1000000000000000472, 0.003490658503988666988 ) ;
#15621 = ORIENTED_EDGE ( 'NONE', *, *, #39439, .T. ) ;
#15622 = DIRECTION ( 'NONE',  ( 0.000000000000000000, 1.000000000000000000, 0.000000000000000000 ) ) ;
#15623 = CARTESIAN_POINT ( 'NONE',  ( 13.14999999999990088, 2.500000000000000000, 1.918653347947321564 ) ) ;
#15624 = CARTESIAN_POINT ( 'NONE',  ( 8.749999999999953815, 12.50000000000000000, 6.495190528383297135 ) ) ;
#15625 = EDGE_LOOP ( 'NONE', ( #57211, #65939, #124671, #93586 ) ) ;
#15626 = ORIENTED_EDGE ( 'NONE', *, *, #58628, .T. ) ;
#15627 = DIRECTION ( 'NONE',  ( -4.274815082592931898E-19, -0.9999939076577903929, -0.003490651415223739937 ) ) ;
#15628 = EDGE_CURVE ( 'NONE', #82756, #72150, #457, .T. ) ;
#15629 = VERTEX_POINT ( 'NONE', #113009 ) ;
#15630 = CARTESIAN_POINT ( 'NONE',  ( 9.799999999999913669, 2.500000000000000000, -3.983716857408426293 ) ) ;
#15631 = DIRECTION ( 'NONE',  ( -0.000000000000000000, 1.000000000000000000, -0.000000000000000000 ) ) ;
#15632 = CIRCLE ( 'NONE', #3144, 0.06509327318403741736 ) ;
#15633 = EDGE_LOOP ( 'NONE', ( #49898, #64759, #37792, #71767 ) ) ;
#15634 = DIRECTION ( 'NONE',  ( -4.274815082592931898E-19, -0.9999939076577903929, -0.003490651415223739937 ) ) ;
#15635 = CARTESIAN_POINT ( 'NONE',  ( 6.899999999999928413, 2.500000000000000000, 3.983716857408420964 ) ) ;
#15636 = DIRECTION ( 'NONE',  ( -0.000000000000000000, -1.000000000000000000, -0.000000000000000000 ) ) ;
#15637 = DIRECTION ( 'NONE',  ( 0.000000000000000000, -0.000000000000000000, 1.000000000000000000 ) ) ;
#15638 = DIRECTION ( 'NONE',  ( 0.000000000000000000, 0.000000000000000000, 1.000000000000000000 ) ) ;
#15639 = ORIENTED_EDGE ( 'NONE', *, *, #70950, .T. ) ;
#15640 = ORIENTED_EDGE ( 'NONE', *, *, #127711, .T. ) ;
#15641 = DIRECTION ( 'NONE',  ( 0.000000000000000000, 1.000000000000000000, 0.000000000000000000 ) ) ;
#15642 = AXIS2_PLACEMENT_3D ( 'NONE', #87713, #59591, #127649 ) ;
#15643 = AXIS2_PLACEMENT_3D ( 'NONE', #40275, #30470, #128683 ) ;
#15644 = ADVANCED_FACE ( 'NONE', ( #23326 ), #89130, .T. ) ;
#15645 = LINE ( 'NONE', #66689, #107865 ) ;
#15646 = CARTESIAN_POINT ( 'NONE',  ( -6.650000000000019007, 2.500000000000000000, -5.802370205355749988 ) ) ;
#15648 = ORIENTED_EDGE ( 'NONE', *, *, #19886, .T. ) ;
#15647 = ORIENTED_EDGE ( 'NONE', *, *, #53263, .T. ) ;
#15649 = EDGE_LOOP ( 'NONE', ( #86903, #99261 ) ) ;
#15650 = CARTESIAN_POINT ( 'NONE',  ( -3.150000000000030109, 2.500000000000000000, -2.511473670974877948 ) ) ;
#15651 = CIRCLE ( 'NONE', #55384, 0.06509327318403745899 ) ;
#15652 = CARTESIAN_POINT ( 'NONE',  ( -5.200000000000022382, 12.50000000000000000, 4.741630453620009789 ) ) ;
#15653 = CARTESIAN_POINT ( 'NONE',  ( -10.85000000000000142, 2.500000000000000000, -2.265063509461097802 ) ) ;
#15654 = CARTESIAN_POINT ( 'NONE',  ( 129.5000000000000000, -1.375000000000000000, 7.634788798650553154 ) ) ;
#15655 = DIRECTION ( 'NONE',  ( 0.000000000000000000, 0.000000000000000000, 1.000000000000000000 ) ) ;
#15656 = FACE_OUTER_BOUND ( 'NONE', #129183, .T. ) ;
#15657 = CARTESIAN_POINT ( 'NONE',  ( 14.99999999999989342, 2.500000000000000000, -0.6928203230275541413 ) ) ;
#15658 = DIRECTION ( 'NONE',  ( 0.000000000000000000, 0.000000000000000000, 1.000000000000000000 ) ) ;
#15659 = EDGE_CURVE ( 'NONE', #85940, #56105, #84925, .T. ) ;
#15660 = DIRECTION ( 'NONE',  ( 0.000000000000000000, -0.9999939076577903929, 0.003490651415223739937 ) ) ;
#15661 = VERTEX_POINT ( 'NONE', #84184 ) ;
#15662 = AXIS2_PLACEMENT_3D ( 'NONE', #108589, #89598, #81073 ) ;
#15663 = AXIS2_PLACEMENT_3D ( 'NONE', #42950, #82859, #73648 ) ;
#15664 = DIRECTION ( 'NONE',  ( 0.000000000000000000, 0.000000000000000000, 1.000000000000000000 ) ) ;
#15665 = CIRCLE ( 'NONE', #7355, 0.09999999999999982514 ) ;
#15666 = ORIENTED_EDGE ( 'NONE', *, *, #93447, .F. ) ;
#15667 = ADVANCED_FACE ( 'NONE', ( #4317 ), #76611, .T. ) ;
#15668 = EDGE_LOOP ( 'NONE', ( #128274, #81775 ) ) ;
#15669 = DIRECTION ( 'NONE',  ( 0.000000000000000000, 1.000000000000000000, 0.000000000000000000 ) ) ;
#15670 = DIRECTION ( 'NONE',  ( -0.000000000000000000, 1.000000000000000000, -0.000000000000000000 ) ) ;
#15671 = CARTESIAN_POINT ( 'NONE',  ( 12.69999999999990337, 2.500000000000000000, -4.676537180435978769 ) ) ;
#15672 = CIRCLE ( 'NONE', #74187, 0.1000000000000002554 ) ;
#15673 = CARTESIAN_POINT ( 'NONE',  ( -3.750000000000025757, 2.500000000000000000, -2.857883832488653741 ) ) ;
#15674 = AXIS2_PLACEMENT_3D ( 'NONE', #102101, #82473, #22905 ) ;
#15676 = DIRECTION ( 'NONE',  ( -0.000000000000000000, 1.000000000000000000, -0.000000000000000000 ) ) ;
#15675 = CIRCLE ( 'NONE', #9445, 0.1000000000000002554 ) ;
#15677 = LINE ( 'NONE', #117097, #124357 ) ;
#15678 = DIRECTION ( 'NONE',  ( 0.000000000000000000, 0.000000000000000000, 1.000000000000000000 ) ) ;
#15679 = EDGE_LOOP ( 'NONE', ( #16231, #12473, #72538, #26577 ) ) ;
#15680 = DIRECTION ( 'NONE',  ( 0.000000000000000000, 1.000000000000000000, 0.000000000000000000 ) ) ;
#15681 = AXIS2_PLACEMENT_3D ( 'NONE', #114401, #24098, #103949 ) ;
#15682 = FACE_OUTER_BOUND ( 'NONE', #69945, .T. ) ;
#15684 = ORIENTED_EDGE ( 'NONE', *, *, #82068, .T. ) ;
#15683 = CONICAL_SURFACE ( 'NONE', #97267, 0.09999999999999999167, 0.003490658503988666988 ) ;
#15685 = VECTOR ( 'NONE', #111584, 1000.000000000000000 ) ;
#15686 = EDGE_LOOP ( 'NONE', ( #90829, #39291, #43700, #65240 ) ) ;
#15687 = ADVANCED_FACE ( 'NONE', ( #124114 ), #105859, .T. ) ;
#15688 = EDGE_LOOP ( 'NONE', ( #55524, #35214, #24544, #51695 ) ) ;
#15689 = VECTOR ( 'NONE', #95081, 1000.000000000000000 ) ;
#15690 = ORIENTED_EDGE ( 'NONE', *, *, #23388, .F. ) ;
#15691 = DIRECTION ( 'NONE',  ( 0.000000000000000000, 0.000000000000000000, 1.000000000000000000 ) ) ;
#15692 = CARTESIAN_POINT ( 'NONE',  ( -9.350000000000008527, 2.500000000000000000, -6.048780366869521252 ) ) ;
#15693 = ADVANCED_FACE ( 'NONE', ( #83566 ), #39078, .T. ) ;
#15694 = CARTESIAN_POINT ( 'NONE',  ( -10.20000000000000284, 2.500000000000000000, 4.083716857408421497 ) ) ;
#15695 = CARTESIAN_POINT ( 'NONE',  ( -9.999999999999971578, 2.500000000000000000, -4.330127018922197202 ) ) ;
#15696 = DIRECTION ( 'NONE',  ( -0.000000000000000000, -1.000000000000000000, -0.000000000000000000 ) ) ;
#15697 = VERTEX_POINT ( 'NONE', #64549 ) ;
#15698 = CARTESIAN_POINT ( 'NONE',  ( -14.14999999999998792, 2.500000000000000000, -1.372243186433547812 ) ) ;
#15699 = EDGE_CURVE ( 'NONE', #104225, #83642, #112378, .T. ) ;
#15700 = EDGE_CURVE ( 'NONE', #90750, #72456, #44926, .T. ) ;
#15701 = EDGE_CURVE ( 'NONE', #26026, #108711, #104473, .T. ) ;
#15702 = DIRECTION ( 'NONE',  ( -4.274815082592931898E-19, -0.9999939076577903929, -0.003490651415223739937 ) ) ;
#15703 = EDGE_CURVE ( 'NONE', #74853, #52514, #82920, .T. ) ;
#15704 = AXIS2_PLACEMENT_3D ( 'NONE', #102253, #43340, #64245 ) ;
#15705 = DIRECTION ( 'NONE',  ( 0.000000000000000000, 0.000000000000000000, -1.000000000000000000 ) ) ;
#15706 = ORIENTED_EDGE ( 'NONE', *, *, #39245, .F. ) ;
#15707 = VERTEX_POINT ( 'NONE', #55385 ) ;
#15709 = ORIENTED_EDGE ( 'NONE', *, *, #26631, .T. ) ;
#15708 = ADVANCED_FACE ( 'NONE', ( #95309 ), #12850, .T. ) ;
#15710 = LINE ( 'NONE', #106043, #105216 ) ;
#15711 = EDGE_CURVE ( 'NONE', #56932, #106131, #47369, .T. ) ;
#15712 = AXIS2_PLACEMENT_3D ( 'NONE', #24977, #16413, #33526 ) ;
#15713 = EDGE_CURVE ( 'NONE', #56340, #19273, #110066, .T. ) ;
#15714 = AXIS2_PLACEMENT_3D ( 'NONE', #8221, #19996, #128004 ) ;
#15715 = FACE_OUTER_BOUND ( 'NONE', #36806, .T. ) ;
#15716 = DIRECTION ( 'NONE',  ( 0.000000000000000000, 1.000000000000000000, 0.000000000000000000 ) ) ;
#15717 = CONICAL_SURFACE ( 'NONE', #97305, 0.09999999999999982514, 0.003490658503988666988 ) ;
#15718 = EDGE_CURVE ( 'NONE', #128284, #57396, #93376, .T. ) ;
#15719 = EDGE_CURVE ( 'NONE', #2171, #66080, #68281, .T. ) ;
#15720 = EDGE_LOOP ( 'NONE', ( #42680, #116032, #58088, #74123 ) ) ;
#15721 = DIRECTION ( 'NONE',  ( 0.000000000000000000, 0.000000000000000000, 1.000000000000000000 ) ) ;
#15722 = FACE_OUTER_BOUND ( 'NONE', #1280, .T. ) ;
#15723 = DIRECTION ( 'NONE',  ( 0.000000000000000000, 1.000000000000000000, 0.000000000000000000 ) ) ;
#15724 = DIRECTION ( 'NONE',  ( 0.000000000000000000, 1.000000000000000000, 0.000000000000000000 ) ) ;
#15725 = DIRECTION ( 'NONE',  ( 0.000000000000000000, 0.000000000000000000, 1.000000000000000000 ) ) ;
#15726 = ADVANCED_FACE ( 'NONE', ( #5614 ), #33185, .T. ) ;
#15727 = AXIS2_PLACEMENT_3D ( 'NONE', #91734, #2050, #52445 ) ;
#15728 = EDGE_LOOP ( 'NONE', ( #126427, #27391, #49551, #43110 ) ) ;
#15729 = CARTESIAN_POINT ( 'NONE',  ( -2.950000000000029932, 12.50000000000000000, 2.165063509461097713 ) ) ;
#15730 = CIRCLE ( 'NONE', #36691, 0.06509327318403745899 ) ;
#15731 = ORIENTED_EDGE ( 'NONE', *, *, #85065, .F. ) ;
#15732 = ORIENTED_EDGE ( 'NONE', *, *, #50306, .T. ) ;
#15733 = EDGE_LOOP ( 'NONE', ( #89097, #97240, #94497, #29643 ) ) ;
#15734 = CARTESIAN_POINT ( 'NONE',  ( -5.400000000000019895, 12.50000000000000000, -0.6928203230275541413 ) ) ;
#15735 = FACE_BOUND ( 'NONE', #15188, .T. ) ;
#15736 = DIRECTION ( 'NONE',  ( -0.000000000000000000, -1.000000000000000000, -0.000000000000000000 ) ) ;
#15737 = DIRECTION ( 'NONE',  ( 0.000000000000000000, 0.000000000000000000, -1.000000000000000000 ) ) ;
#15738 = CARTESIAN_POINT ( 'NONE',  ( -9.550000000000007816, 2.500000000000000000, -6.495190528383297135 ) ) ;
#15739 = CIRCLE ( 'NONE', #109757, 0.1000000000000000472 ) ;
#15740 = VECTOR ( 'NONE', #44791, 1000.000000000000000 ) ;
#15741 = ORIENTED_EDGE ( 'NONE', *, *, #102292, .T. ) ;
#15742 = CARTESIAN_POINT ( 'NONE',  ( 6.849999999999929479, 2.500000000000000000, -2.511473670974877948 ) ) ;
#15743 = DIRECTION ( 'NONE',  ( 0.000000000000000000, 1.000000000000000000, 0.000000000000000000 ) ) ;
#15744 = DIRECTION ( 'NONE',  ( 0.000000000000000000, 1.000000000000000000, 0.000000000000000000 ) ) ;
#15745 = FACE_OUTER_BOUND ( 'NONE', #23040, .T. ) ;
#15746 = ORIENTED_EDGE ( 'NONE', *, *, #74394, .F. ) ;
#15747 = CARTESIAN_POINT ( 'NONE',  ( 11.44999999999990514, 2.500000000000000000, -6.248780366869526759 ) ) ;
#15748 = FACE_OUTER_BOUND ( 'NONE', #35338, .T. ) ;
#15749 = AXIS2_PLACEMENT_3D ( 'NONE', #92783, #54141, #53505 ) ;
#15750 = ORIENTED_EDGE ( 'NONE', *, *, #74186, .T. ) ;
#15751 = CARTESIAN_POINT ( 'NONE',  ( 6.649999999999927525, 12.50000000000000000, 2.165063509461097713 ) ) ;
#15752 = CIRCLE ( 'NONE', #88938, 0.09999999999999982514 ) ;
#15753 = ORIENTED_EDGE ( 'NONE', *, *, #100391, .F. ) ;
#15754 = FACE_BOUND ( 'NONE', #90528, .T. ) ;
#15755 = CARTESIAN_POINT ( 'NONE',  ( -8.300000000000011369, 2.500000000000000000, -4.330127018922201643 ) ) ;
#15756 = EDGE_CURVE ( 'NONE', #82926, #120749, #103842, .T. ) ;
#15757 = CIRCLE ( 'NONE', #3173, 0.06509327318403743123 ) ;
#15758 = ORIENTED_EDGE ( 'NONE', *, *, #2345, .F. ) ;
#15759 = FACE_OUTER_BOUND ( 'NONE', #76218, .T. ) ;
#15760 = DIRECTION ( 'NONE',  ( 0.000000000000000000, 1.000000000000000000, 0.000000000000000000 ) ) ;
#15761 = AXIS2_PLACEMENT_3D ( 'NONE', #46621, #15865, #86546 ) ;
#15762 = EDGE_CURVE ( 'NONE', #79929, #24152, #18111, .T. ) ;
#15763 = EDGE_LOOP ( 'NONE', ( #23908, #80187, #59821, #56332 ) ) ;
#15764 =( BOUNDED_CURVE ( )  B_SPLINE_CURVE ( 2, ( #114067, #45339, #24397, #104244, #125176, #13916, #14556 ),
 .UNSPECIFIED., .F., .F. ) 
 B_SPLINE_CURVE_WITH_KNOTS ( ( 3, 2, 2, 3 ),
 ( 0.3571428571428574283, 0.3809523809523812643, 0.4047619047619051003, 0.4285714285714289362 ),
 .UNSPECIFIED. ) 
 CURVE ( )  GEOMETRIC_REPRESENTATION_ITEM ( )  RATIONAL_B_SPLINE_CURVE ( ( 0.9999999999999984457, 0.8660254037844402619, 1.000000000000000000, 0.8660254037844387076, 1.000000000000000000, 0.8660254037844364872, 1.000000000000002220 ) ) 
 REPRESENTATION_ITEM ( '' )  );
#15765 = ORIENTED_EDGE ( 'NONE', *, *, #76416, .T. ) ;
#15766 = CARTESIAN_POINT ( 'NONE',  ( 185.0468750003414016, -8.734944146203032389, -1.604583208406768146E-15 ) ) ;
#15767 = ORIENTED_EDGE ( 'NONE', *, *, #105524, .T. ) ;
#15768 = CARTESIAN_POINT ( 'NONE',  ( 184.7552083336747444, 6.551208109652275624, -3.782341765624998686 ) ) ;
#15769 = CARTESIAN_POINT ( 'NONE',  ( -11.64999999999999858, 2.500000000000000000, -1.372243186433546036 ) ) ;
#15771 = ADVANCED_FACE ( 'NONE', ( #116222 ), #128957, .T. ) ;
#15770 = AXIS2_PLACEMENT_3D ( 'NONE', #82681, #94400, #55774 ) ;
#15772 = CIRCLE ( 'NONE', #76340, 0.1000000000000000472 ) ;
#15773 = CARTESIAN_POINT ( 'NONE',  ( 0.4499999999999569344, 2.500000000000000000, -2.165063509461101710 ) ) ;
#15774 = CARTESIAN_POINT ( 'NONE',  ( 5.849999999999935696, 2.500000000000000000, -7.288010851410854585 ) ) ;
#15775 = AXIS2_PLACEMENT_3D ( 'NONE', #82876, #3018, #42972 ) ;
#15776 = DIRECTION ( 'NONE',  ( 0.000000000000000000, 0.000000000000000000, 1.000000000000000000 ) ) ;
#15777 = VECTOR ( 'NONE', #20063, 1000.000000000000000 ) ;
#15778 = AXIS2_PLACEMENT_3D ( 'NONE', #19157, #69563, #68270 ) ;
#15779 = ORIENTED_EDGE ( 'NONE', *, *, #106575, .F. ) ;
#15780 = ORIENTED_EDGE ( 'NONE', *, *, #95880, .T. ) ;
#15781 = CARTESIAN_POINT ( 'NONE',  ( -9.400000000000009237, 2.500000000000000000, -3.983716857408421852 ) ) ;
#15782 = CARTESIAN_POINT ( 'NONE',  ( -11.44999999999999751, 2.500000000000000000, 2.511473670974873507 ) ) ;
#15783 = DIRECTION ( 'NONE',  ( 0.000000000000000000, 1.000000000000000000, 0.000000000000000000 ) ) ;
#15784 = AXIS2_PLACEMENT_3D ( 'NONE', #72708, #121159, #52415 ) ;
#15785 = LINE ( 'NONE', #55717, #78293 ) ;
#15787 = EDGE_LOOP ( 'NONE', ( #122378, #15044, #12079, #28384 ) ) ;
#15786 = ORIENTED_EDGE ( 'NONE', *, *, #48643, .T. ) ;
#15788 = PLANE ( 'NONE',  #95543 ) ;
#15789 = ORIENTED_EDGE ( 'NONE', *, *, #1251, .F. ) ;
#15790 = CARTESIAN_POINT ( 'NONE',  ( -14.14999999999998614, 2.500000000000000000, 2.165063509461101265 ) ) ;
#15791 = DIRECTION ( 'NONE',  ( 0.000000000000000000, 1.000000000000000000, 0.000000000000000000 ) ) ;
#15792 = VERTEX_POINT ( 'NONE', #6255 ) ;
#15793 = CARTESIAN_POINT ( 'NONE',  ( -14.59999999999998366, 12.50000000000000000, -0.6277270498435145729 ) ) ;
#15794 = CARTESIAN_POINT ( 'NONE',  ( 14.59999999999989484, 12.50000000000000000, -0.6928203230275541413 ) ) ;
#15795 = CARTESIAN_POINT ( 'NONE',  ( -1.050000000000037348, 2.500000000000000000, -2.411473670974877859 ) ) ;
#15796 = LINE ( 'NONE', #97586, #52847 ) ;
#15797 = CARTESIAN_POINT ( 'NONE',  ( 187.5000000000000000, 0.000000000000000000, 0.000000000000000000 ) ) ;
#15798 = FACE_OUTER_BOUND ( 'NONE', #58359, .T. ) ;
#15799 = DIRECTION ( 'NONE',  ( 0.000000000000000000, 0.000000000000000000, 1.000000000000000000 ) ) ;
#15800 = DIRECTION ( 'NONE',  ( 0.000000000000000000, 0.000000000000000000, -1.000000000000000000 ) ) ;
#15801 = DIRECTION ( 'NONE',  ( 0.000000000000000000, 0.000000000000000000, -1.000000000000000000 ) ) ;
#15802 = ADVANCED_FACE ( 'NONE', ( #48627 ), #30295, .T. ) ;
#15803 = ORIENTED_EDGE ( 'NONE', *, *, #124543, .T. ) ;
#15804 = VERTEX_POINT ( 'NONE', #9988 ) ;
#15805 = PLANE ( 'NONE',  #90997 ) ;
#15806 = ORIENTED_EDGE ( 'NONE', *, *, #73936, .T. ) ;
#15807 = LINE ( 'NONE', #7923, #89581 ) ;
#15809 = ORIENTED_EDGE ( 'NONE', *, *, #75036, .T. ) ;
#15808 = EDGE_LOOP ( 'NONE', ( #27171, #52875 ) ) ;
#15810 = VECTOR ( 'NONE', #20956, 1000.000000000000000 ) ;
#15811 = ORIENTED_EDGE ( 'NONE', *, *, #128860, .T. ) ;
#15812 = EDGE_CURVE ( 'NONE', #74379, #89315, #120529, .T. ) ;
#15813 = FACE_OUTER_BOUND ( 'NONE', #4161, .T. ) ;
#15814 = AXIS2_PLACEMENT_3D ( 'NONE', #72929, #42859, #112215 ) ;
#15815 = CONICAL_SURFACE ( 'NONE', #74413, 0.1000000000000000472, 0.003490658503988666988 ) ;
#15816 = FACE_OUTER_BOUND ( 'NONE', #77293, .T. ) ;
#15817 = CONICAL_SURFACE ( 'NONE', #122451, 0.1000000000000002554, 0.003490658503988666988 ) ;
#15818 = CARTESIAN_POINT ( 'NONE',  ( 8.099999999999921485, 2.500000000000000000, 0.4464101615137735513 ) ) ;
#15819 = CARTESIAN_POINT ( 'NONE',  ( 0.6499999999999566125, 12.50000000000000000, -6.906693963081115051 ) ) ;
#15820 = EDGE_CURVE ( 'NONE', #86126, #27663, #112211, .T. ) ;
#15821 = DIRECTION ( 'NONE',  ( -0.000000000000000000, -1.000000000000000000, -0.000000000000000000 ) ) ;
#15822 = VERTEX_POINT ( 'NONE', #9342 ) ;
#15823 = ADVANCED_FACE ( 'NONE', ( #128499 ), #101746, .T. ) ;
#15824 = CARTESIAN_POINT ( 'NONE',  ( 8.749999999999921840, 12.50000000000000000, 2.922977105672686982 ) ) ;
#15825 = ORIENTED_EDGE ( 'NONE', *, *, #129082, .T. ) ;
#15826 = CIRCLE ( 'NONE', #43058, 0.06509327318403745899 ) ;
#15827 = EDGE_LOOP ( 'NONE', ( #36784, #25222, #64296, #33244 ) ) ;
#15828 = ORIENTED_EDGE ( 'NONE', *, *, #83091, .F. ) ;
#15829 = EDGE_LOOP ( 'NONE', ( #849, #79661 ) ) ;
#15831 = AXIS2_PLACEMENT_3D ( 'NONE', #22742, #22097, #11607 ) ;
#15830 = AXIS2_PLACEMENT_3D ( 'NONE', #121743, #104049, #13716 ) ;
#15832 = CARTESIAN_POINT ( 'NONE',  ( 185.0312500006828031, 9.429780353434619030E-16, -7.700000000000000178 ) ) ;
#15833 = ORIENTED_EDGE ( 'NONE', *, *, #52360, .F. ) ;
#15834 = EDGE_CURVE ( 'NONE', #107252, #87657, #97527, .T. ) ;
#15835 = ORIENTED_EDGE ( 'NONE', *, *, #36588, .T. ) ;
#15836 = DIRECTION ( 'NONE',  ( -4.274815082592931898E-19, -0.9999939076577903929, -0.003490651415223739937 ) ) ;
#15838 = AXIS2_PLACEMENT_3D ( 'NONE', #42183, #52634, #2904 ) ;
#15837 = FACE_OUTER_BOUND ( 'NONE', #79505, .T. ) ;
#15839 = CARTESIAN_POINT ( 'NONE',  ( -5.800000000000018474, 2.500000000000000000, -2.276824562219559311E-15 ) ) ;
#15840 = CIRCLE ( 'NONE', #89016, 0.09999999999999982514 ) ;
#15841 = DIRECTION ( 'NONE',  ( 0.000000000000000000, 1.000000000000000000, 0.000000000000000000 ) ) ;
#15842 = CARTESIAN_POINT ( 'NONE',  ( 1.049999999999953637, 2.500000000000000000, 2.411473670974873862 ) ) ;
#15843 = DIRECTION ( 'NONE',  ( -0.000000000000000000, -1.000000000000000000, -0.000000000000000000 ) ) ;
#15844 = EDGE_LOOP ( 'NONE', ( #52282, #62267 ) ) ;
#15845 = CARTESIAN_POINT ( 'NONE',  ( -4.150000000000027889, 2.500000000000000000, -7.288010851410854585 ) ) ;
#15846 = VERTEX_POINT ( 'NONE', #49936 ) ;
#15847 = CARTESIAN_POINT ( 'NONE',  ( -12.89999999999999147, 2.500000000000000000, -0.5928203230275499447 ) ) ;
#15848 = ORIENTED_EDGE ( 'NONE', *, *, #106173, .T. ) ;
#15849 = DIRECTION ( 'NONE',  ( -0.000000000000000000, 1.000000000000000000, -0.000000000000000000 ) ) ;
#15850 = ORIENTED_EDGE ( 'NONE', *, *, #114069, .F. ) ;
#15851 = ORIENTED_EDGE ( 'NONE', *, *, #46651, .F. ) ;
#15852 = DIRECTION ( 'NONE',  ( 0.000000000000000000, -0.9999939076577903929, 0.003490651415223739937 ) ) ;
#15853 = FACE_OUTER_BOUND ( 'NONE', #34533, .T. ) ;
#15854 = ADVANCED_FACE ( 'NONE', ( #60400 ), #28593, .T. ) ;
#15855 = CIRCLE ( 'NONE', #1199, 0.06509327318403745899 ) ;
#15856 = CYLINDRICAL_SURFACE ( 'NONE', #119801, 7.699999999999999289 ) ;
#15858 = DIRECTION ( 'NONE',  ( -0.000000000000000000, -1.000000000000000000, -0.000000000000000000 ) ) ;
#15857 = AXIS2_PLACEMENT_3D ( 'NONE', #108755, #97656, #127137 ) ;
#15859 = CARTESIAN_POINT ( 'NONE',  ( 9.349999999999919709, 2.500000000000000000, 1.818653347947321475 ) ) ;
#15860 = ORIENTED_EDGE ( 'NONE', *, *, #78097, .F. ) ;
#15861 = DIRECTION ( 'NONE',  ( 0.000000000000000000, 0.000000000000000000, 1.000000000000000000 ) ) ;
#15862 = DIRECTION ( 'NONE',  ( 0.000000000000000000, 0.000000000000000000, 1.000000000000000000 ) ) ;
#15863 = EDGE_CURVE ( 'NONE', #98343, #35123, #89829, .T. ) ;
#15864 = CARTESIAN_POINT ( 'NONE',  ( 187.5000000000000000, 0.9999999999999985567, 7.634788798650556707 ) ) ;
#15865 = DIRECTION ( 'NONE',  ( 0.000000000000000000, 1.000000000000000000, 0.000000000000000000 ) ) ;
#15866 = ADVANCED_FACE ( 'NONE', ( #115568 ), #45324, .T. ) ;
#15867 = CARTESIAN_POINT ( 'NONE',  ( -3.350000000000028955, 2.500000000000000000, -2.165063509461101710 ) ) ;
#15868 = ORIENTED_EDGE ( 'NONE', *, *, #50464, .F. ) ;
#15869 = VERTEX_POINT ( 'NONE', #25930 ) ;
#15870 = ADVANCED_FACE ( 'NONE', ( #110121 ), #1384, .T. ) ;
#15871 = CIRCLE ( 'NONE', #7460, 0.06509327318403745899 ) ;
#15872 = EDGE_CURVE ( 'NONE', #111323, #4351, #62046, .T. ) ;
#15873 = ADVANCED_FACE ( 'NONE', ( #40096 ), #87061, .T. ) ;
#15874 = ORIENTED_EDGE ( 'NONE', *, *, #129252, .T. ) ;
#15875 = VECTOR ( 'NONE', #111491, 1000.000000000000000 ) ;
#15876 = LINE ( 'NONE', #56444, #125990 ) ;
#15878 = AXIS2_PLACEMENT_3D ( 'NONE', #112727, #2758, #82629 ) ;
#15877 = DIRECTION ( 'NONE',  ( 0.000000000000000000, 0.000000000000000000, -1.000000000000000000 ) ) ;
#15879 = AXIS2_PLACEMENT_3D ( 'NONE', #6615, #36779, #20347 ) ;
#15880 = ADVANCED_FACE ( 'NONE', ( #95948 ), #114255, .T. ) ;
#15881 = CONICAL_SURFACE ( 'NONE', #91107, 0.1000000000000002554, 0.003490658503988666988 ) ;
#15882 = CARTESIAN_POINT ( 'NONE',  ( 185.3333333333333144, 6.668395609140177704, -3.849999999999998312 ) ) ;
#15883 = DIRECTION ( 'NONE',  ( 0.000000000000000000, 0.000000000000000000, 1.000000000000000000 ) ) ;
#15884 = CARTESIAN_POINT ( 'NONE',  ( 2.699999999999945555, 12.50000000000000000, 3.983716857408420076 ) ) ;
#15885 = CARTESIAN_POINT ( 'NONE',  ( -1.250000000000036193, 2.500000000000000000, 5.802370205355744659 ) ) ;
#15886 = DIRECTION ( 'NONE',  ( -4.274815082592931898E-19, -0.9999939076577903929, -0.003490651415223739937 ) ) ;
#15887 = VERTEX_POINT ( 'NONE', #28995 ) ;
#15888 = ADVANCED_FACE ( 'NONE', ( #99666 ), #34870, .T. ) ;
#15889 = DIRECTION ( 'NONE',  ( 0.000000000000000000, 0.000000000000000000, 1.000000000000000000 ) ) ;
#15890 = CARTESIAN_POINT ( 'NONE',  ( 3.149999999999942624, 12.50000000000000000, 6.906693963081109722 ) ) ;
#15891 = ORIENTED_EDGE ( 'NONE', *, *, #43119, .T. ) ;
#15892 = FACE_OUTER_BOUND ( 'NONE', #100368, .T. ) ;
#15893 = CARTESIAN_POINT ( 'NONE',  ( 2.499999999999948930, 2.500000000000000000, -4.922947341949753586 ) ) ;
#15894 = DIRECTION ( 'NONE',  ( 0.000000000000000000, 1.000000000000000000, 0.000000000000000000 ) ) ;
#15895 = ORIENTED_EDGE ( 'NONE', *, *, #86961, .T. ) ;
#15896 = CARTESIAN_POINT ( 'NONE',  ( 5.399999999999936406, 2.500000000000000000, -5.022947341949754119 ) ) ;
#15897 = CONICAL_SURFACE ( 'NONE', #84954, 0.09999999999999982514, 0.003490658503988666988 ) ;
#15898 = ORIENTED_EDGE ( 'NONE', *, *, #88906, .F. ) ;
#15899 = DIRECTION ( 'NONE',  ( -0.000000000000000000, -1.000000000000000000, -0.000000000000000000 ) ) ;
#15900 = CARTESIAN_POINT ( 'NONE',  ( -6.450000000000017941, 12.50000000000000000, -2.511473670974877948 ) ) ;
#15901 = AXIS2_PLACEMENT_3D ( 'NONE', #43329, #13187, #123168 ) ;
#15902 = AXIS2_PLACEMENT_3D ( 'NONE', #41403, #81314, #23674 ) ;
#15903 = VERTEX_POINT ( 'NONE', #125410 ) ;
#15904 = CARTESIAN_POINT ( 'NONE',  ( -5.650000000000019895, 12.50000000000000000, 1.818653347947321475 ) ) ;
#15905 = AXIS2_PLACEMENT_3D ( 'NONE', #120424, #31409, #30774 ) ;
#15906 = DIRECTION ( 'NONE',  ( 0.000000000000000000, 1.000000000000000000, 0.000000000000000000 ) ) ;
#15907 = VERTEX_POINT ( 'NONE', #58458 ) ;
#15909 = VECTOR ( 'NONE', #67237, 1000.000000000000000 ) ;
#15908 = FACE_OUTER_BOUND ( 'NONE', #41058, .T. ) ;
#15911 = ORIENTED_EDGE ( 'NONE', *, *, #110716, .T. ) ;
#15910 = ADVANCED_FACE ( 'NONE', ( #68899 ), #60007, .T. ) ;
#15912 = ORIENTED_EDGE ( 'NONE', *, *, #5363, .F. ) ;
#15913 = CARTESIAN_POINT ( 'NONE',  ( 3.099999999999945022, 12.50000000000000000, -4.676537180435978769 ) ) ;
#15914 = LINE ( 'NONE', #23163, #62593 ) ;
#15915 = VERTEX_POINT ( 'NONE', #21088 ) ;
#15916 = DIRECTION ( 'NONE',  ( 0.000000000000000000, 1.000000000000000000, 0.000000000000000000 ) ) ;
#15917 = DIRECTION ( 'NONE',  ( 0.000000000000000000, 0.000000000000000000, -1.000000000000000000 ) ) ;
#15918 = ORIENTED_EDGE ( 'NONE', *, *, #125521, .F. ) ;
#15919 = EDGE_CURVE ( 'NONE', #123777, #115296, #105945, .T. ) ;
#15920 = CARTESIAN_POINT ( 'NONE',  ( 10.44999999999991402, 12.50000000000000000, 6.495190528383297135 ) ) ;
#15921 = DIRECTION ( 'NONE',  ( -0.000000000000000000, 1.000000000000000000, -0.000000000000000000 ) ) ;
#15922 = CARTESIAN_POINT ( 'NONE',  ( -3.350000000000028511, 12.50000000000000000, 2.857883832488649301 ) ) ;
#15923 = FACE_OUTER_BOUND ( 'NONE', #89774, .T. ) ;
#15924 = CARTESIAN_POINT ( 'NONE',  ( -6.505213034913026604E-15, 12.50000000000000000, 4.330127018922196314 ) ) ;
#15925 = DIRECTION ( 'NONE',  ( 0.000000000000000000, 0.000000000000000000, 1.000000000000000000 ) ) ;
#15926 = VERTEX_POINT ( 'NONE', #10604 ) ;
#15927 = ORIENTED_EDGE ( 'NONE', *, *, #73766, .F. ) ;
#15928 = EDGE_LOOP ( 'NONE', ( #19221, #52078 ) ) ;
#15929 = ORIENTED_EDGE ( 'NONE', *, *, #94768, .T. ) ;
#15930 = CARTESIAN_POINT ( 'NONE',  ( 76.44220535185989718, 3.905138931494375854, 5.869652189505977447 ) ) ;
#15931 = DIRECTION ( 'NONE',  ( 0.000000000000000000, 1.000000000000000000, 0.000000000000000000 ) ) ;
#15932 = DIRECTION ( 'NONE',  ( -0.000000000000000000, 1.000000000000000000, -0.000000000000000000 ) ) ;
#15933 = VERTEX_POINT ( 'NONE', #21747 ) ;
#15934 = FACE_BOUND ( 'NONE', #23210, .T. ) ;
#15935 = FACE_OUTER_BOUND ( 'NONE', #71650, .T. ) ;
#15936 = DIRECTION ( 'NONE',  ( 0.000000000000000000, -0.000000000000000000, 1.000000000000000000 ) ) ;
#15937 = LINE ( 'NONE', #5476, #32465 ) ;
#15938 = VECTOR ( 'NONE', #21117, 1000.000000000000000 ) ;
#15939 = DIRECTION ( 'NONE',  ( 0.000000000000000000, 1.000000000000000000, 0.000000000000000000 ) ) ;
#15940 = CONICAL_SURFACE ( 'NONE', #91266, 0.09999999999999982514, 0.003490658503988666988 ) ;
#15941 = CARTESIAN_POINT ( 'NONE',  ( 1.449999999999951328, 2.500000000000000000, 2.611473670974873151 ) ) ;
#15942 = LINE ( 'NONE', #108202, #108222 ) ;
#15943 = CARTESIAN_POINT ( 'NONE',  ( 5.199999999999933564, 2.500000000000000000, 0.2464101615137735679 ) ) ;
#15944 = FACE_OUTER_BOUND ( 'NONE', #58506, .T. ) ;
#15945 = DIRECTION ( 'NONE',  ( 0.000000000000000000, 1.000000000000000000, 0.000000000000000000 ) ) ;
#15946 = CARTESIAN_POINT ( 'NONE',  ( -1.250000000000001554, 2.500000000000000000, 2.165063509461097713 ) ) ;
#15948 = AXIS2_PLACEMENT_3D ( 'NONE', #99981, #49603, #59431 ) ;
#15947 = AXIS2_PLACEMENT_3D ( 'NONE', #19924, #22514, #41513 ) ;
#15949 = EDGE_CURVE ( 'NONE', #70884, #78664, #12548, .T. ) ;
#15950 = VERTEX_POINT ( 'NONE', #40763 ) ;
#15951 = ORIENTED_EDGE ( 'NONE', *, *, #6828, .F. ) ;
#15952 = EDGE_LOOP ( 'NONE', ( #40600, #55313 ) ) ;
#15953 = ORIENTED_EDGE ( 'NONE', *, *, #106364, .T. ) ;
#15954 = CARTESIAN_POINT ( 'NONE',  ( 11.24999999999990585, 2.500000000000000000, 2.757883832488649656 ) ) ;
#15955 = VERTEX_POINT ( 'NONE', #1446 ) ;
#15956 = DIRECTION ( 'NONE',  ( 0.000000000000000000, -0.000000000000000000, 1.000000000000000000 ) ) ;
#15957 = ORIENTED_EDGE ( 'NONE', *, *, #81790, .T. ) ;
#15958 = VERTEX_POINT ( 'NONE', #32228 ) ;
#15959 = CARTESIAN_POINT ( 'NONE',  ( 5.649999999999934630, 2.500000000000000000, -2.511473670974877948 ) ) ;
#15961 = AXIS2_PLACEMENT_3D ( 'NONE', #85782, #73387, #55046 ) ;
#15960 = CONICAL_SURFACE ( 'NONE', #9622, 0.1000000000000002554, 0.003490658503988666988 ) ;
#15962 = EDGE_CURVE ( 'NONE', #109761, #55194, #90461, .T. ) ;
#15963 = AXIS2_PLACEMENT_3D ( 'NONE', #54950, #111958, #83771 ) ;
#15964 = DIRECTION ( 'NONE',  ( -0.000000000000000000, -1.000000000000000000, -0.000000000000000000 ) ) ;
#15965 = DIRECTION ( 'NONE',  ( 0.000000000000000000, -0.9999939076577903929, 0.003490651415223739937 ) ) ;
#15966 = CARTESIAN_POINT ( 'NONE',  ( 1.899999999999951283, 12.50000000000000000, 0.3464101615137736845 ) ) ;
#15967 = DIRECTION ( 'NONE',  ( 0.000000000000000000, 1.000000000000000000, 0.000000000000000000 ) ) ;
#15968 = EDGE_CURVE ( 'NONE', #95053, #41415, #122667, .T. ) ;
#15969 = EDGE_CURVE ( 'NONE', #4541, #94964, #99699, .T. ) ;
#15970 = ORIENTED_EDGE ( 'NONE', *, *, #98280, .T. ) ;
#15971 = ORIENTED_EDGE ( 'NONE', *, *, #122295, .T. ) ;
#15972 = ORIENTED_EDGE ( 'NONE', *, *, #114552, .T. ) ;
#15973 = ORIENTED_EDGE ( 'NONE', *, *, #70124, .T. ) ;
#15974 = EDGE_CURVE ( 'NONE', #129526, #40642, #76702, .T. ) ;
#15975 = CARTESIAN_POINT ( 'NONE',  ( -0.8500000000000382805, 12.50000000000000000, -1.472243186433550122 ) ) ;
#15976 = ORIENTED_EDGE ( 'NONE', *, *, #27397, .T. ) ;
#15977 = EDGE_CURVE ( 'NONE', #51555, #104463, #52478, .T. ) ;
#15978 = CIRCLE ( 'NONE', #91220, 0.06509327318403745899 ) ;
#15979 = EDGE_LOOP ( 'NONE', ( #22232, #83040, #67763, #21075 ) ) ;
#15980 = DIRECTION ( 'NONE',  ( -4.274815082592931898E-19, -0.9999939076577903929, -0.003490651415223739937 ) ) ;
#15981 = FACE_OUTER_BOUND ( 'NONE', #127035, .T. ) ;
#15983 = AXIS2_PLACEMENT_3D ( 'NONE', #59892, #107680, #58589 ) ;
#15982 = PLANE ( 'NONE',  #106346 ) ;
#15984 = LINE ( 'NONE', #14049, #106799 ) ;
#15985 = CARTESIAN_POINT ( 'NONE',  ( 1.249999999999953815, 2.500000000000000000, 1.572243186433545548 ) ) ;
#15986 = CIRCLE ( 'NONE', #32758, 0.06509327318403745899 ) ;
#15987 = DIRECTION ( 'NONE',  ( 0.000000000000000000, 0.000000000000000000, 1.000000000000000000 ) ) ;
#15988 = VECTOR ( 'NONE', #4643, 1000.000000000000000 ) ;
#15989 = ORIENTED_EDGE ( 'NONE', *, *, #37928, .F. ) ;
#15991 = CONICAL_SURFACE ( 'NONE', #76560, 0.1000000000000002554, 0.003490658503988666988 ) ;
#15990 = DIRECTION ( 'NONE',  ( -0.000000000000000000, -1.000000000000000000, -0.000000000000000000 ) ) ;
#15992 = VERTEX_POINT ( 'NONE', #100929 ) ;
#15993 = AXIS2_PLACEMENT_3D ( 'NONE', #92236, #23499, #3232 ) ;
#15994 = CARTESIAN_POINT ( 'NONE',  ( 186.0833333333333144, -6.668395609140180369, 3.849999999999994760 ) ) ;
#15995 = ORIENTED_EDGE ( 'NONE', *, *, #45900, .F. ) ;
#15996 = LINE ( 'NONE', #36954, #101692 ) ;
#15997 = ADVANCED_FACE ( 'NONE', ( #81311 ), #62143, .T. ) ;
#15998 = CARTESIAN_POINT ( 'NONE',  ( 4.549999999999939426, 12.50000000000000000, -2.099970236277064473 ) ) ;
#15999 = ORIENTED_EDGE ( 'NONE', *, *, #71459, .T. ) ;
#16000 = DIRECTION ( 'NONE',  ( -4.274815082592931898E-19, -0.9999939076577903929, -0.003490651415223739937 ) ) ;
#16001 = DIRECTION ( 'NONE',  ( 0.000000000000000000, 0.000000000000000000, 1.000000000000000000 ) ) ;
#16002 = ORIENTED_EDGE ( 'NONE', *, *, #63499, .T. ) ;
#16003 = CIRCLE ( 'NONE', #124694, 0.09999999999999982514 ) ;
#16004 =( LENGTH_UNIT ( ) NAMED_UNIT ( * ) SI_UNIT ( .MILLI., .METRE. ) );
#16005 = EDGE_CURVE ( 'NONE', #42689, #83000, #97629, .T. ) ;
#16007 = AXIS2_PLACEMENT_3D ( 'NONE', #53793, #62344, #12571 ) ;
#16006 = CIRCLE ( 'NONE', #1347, 1.000000000000000000 ) ;
#16008 = CARTESIAN_POINT ( 'NONE',  ( 9.549999999999918998, 2.500000000000000000, 2.265063509461097357 ) ) ;
#16009 = ORIENTED_EDGE ( 'NONE', *, *, #69957, .T. ) ;
#16010 = ORIENTED_EDGE ( 'NONE', *, *, #84897, .T. ) ;
#16011 = CARTESIAN_POINT ( 'NONE',  ( 179.5000000000000000, -1.375000000000000000, 7.634788798650553154 ) ) ;
#16012 = CARTESIAN_POINT ( 'NONE',  ( -13.94999999999998685, 12.50000000000000000, 1.818653347947325472 ) ) ;
#16013 = CARTESIAN_POINT ( 'NONE',  ( 187.0468750003414300, -8.734944146203032389, -1.604583208406768146E-15 ) ) ;
#16014 = CARTESIAN_POINT ( 'NONE',  ( 2.949999999999945111, 2.500000000000000000, 2.165063509461097713 ) ) ;
#16015 = EDGE_CURVE ( 'NONE', #76654, #71376, #41222, .T. ) ;
#16016 = CARTESIAN_POINT ( 'NONE',  ( 105.6184301395928031, 9.000000000000001776, 1.375000000000001110 ) ) ;
#16017 = CARTESIAN_POINT ( 'NONE',  ( -3.350000000000028955, 2.500000000000000000, 2.165063509461097713 ) ) ;
#16018 = ADVANCED_FACE ( 'NONE', ( #50540 ), #51855, .T. ) ;
#16019 = ADVANCED_FACE ( 'NONE', ( #91766 ), #92401, .T. ) ;
#16020 = ADVANCED_FACE ( 'NONE', ( #53139 ), #18198, .T. ) ;
#16021 = ORIENTED_EDGE ( 'NONE', *, *, #82925, .T. ) ;
#16022 = DIRECTION ( 'NONE',  ( 0.000000000000000000, 1.000000000000000000, 0.000000000000000000 ) ) ;
#16023 = ORIENTED_EDGE ( 'NONE', *, *, #87266, .F. ) ;
#16024 = EDGE_CURVE ( 'NONE', #107957, #108388, #37093, .T. ) ;
#16025 = CARTESIAN_POINT ( 'NONE',  ( 0.6499999999999566125, 2.500000000000000000, -6.148780366869526226 ) ) ;
#16026 = DIRECTION ( 'NONE',  ( 0.000000000000000000, 0.000000000000000000, 1.000000000000000000 ) ) ;
#16027 = CARTESIAN_POINT ( 'NONE',  ( -9.150000000000005684, 2.500000000000000000, 6.395190528383296602 ) ) ;
#16028 = ORIENTED_EDGE ( 'NONE', *, *, #73669, .F. ) ;
#16029 = EDGE_CURVE ( 'NONE', #117308, #7829, #91371, .T. ) ;
#16030 = ADVANCED_FACE ( 'NONE', ( #40541 ), #18290, .F. ) ;
#16031 = AXIS2_PLACEMENT_3D ( 'NONE', #60279, #111254, #10492 ) ;
#16032 = CIRCLE ( 'NONE', #3442, 0.06509327318403745899 ) ;
#16033 = LINE ( 'NONE', #125361, #88958 ) ;
#16034 = FACE_OUTER_BOUND ( 'NONE', #102411, .T. ) ;
#16035 = VERTEX_POINT ( 'NONE', #69311 ) ;
#16036 = CIRCLE ( 'NONE', #120617, 0.06509327318403745899 ) ;
#16037 = DIRECTION ( 'NONE',  ( 0.000000000000000000, 0.000000000000000000, -1.000000000000000000 ) ) ;
#16038 = VERTEX_POINT ( 'NONE', #127609 ) ;
#16039 = VERTEX_POINT ( 'NONE', #8455 ) ;
#16040 = DIRECTION ( 'NONE',  ( -0.9974916312695812914, -0.05217691604166998370, 0.04783319955355741504 ) ) ;
#16041 = VERTEX_POINT ( 'NONE', #77850 ) ;
#16042 = DIRECTION ( 'NONE',  ( 0.000000000000000000, -0.000000000000000000, 1.000000000000000000 ) ) ;
#16043 = DIRECTION ( 'NONE',  ( 0.000000000000000000, -0.000000000000000000, 1.000000000000000000 ) ) ;
#16045 = CIRCLE ( 'NONE', #91285, 0.06509327318403745899 ) ;
#16044 = AXIS2_PLACEMENT_3D ( 'NONE', #93640, #23603, #2022 ) ;
#16046 = CARTESIAN_POINT ( 'NONE',  ( 5.849999999999933920, 12.50000000000000000, 6.495190528383297135 ) ) ;
#16047 = VERTEX_POINT ( 'NONE', #59546 ) ;
#16048 = VECTOR ( 'NONE', #36250, 1000.000000000000000 ) ;
#16049 = FACE_BOUND ( 'NONE', #43371, .T. ) ;
#16051 = ORIENTED_EDGE ( 'NONE', *, *, #123893, .F. ) ;
#16050 = CARTESIAN_POINT ( 'NONE',  ( 4.149999999999941735, 2.500000000000000000, -2.957883832488653830 ) ) ;
#16052 = CARTESIAN_POINT ( 'NONE',  ( -7.300000000000014921, 2.500000000000000000, 4.776537180435972196 ) ) ;
#16053 = CARTESIAN_POINT ( 'NONE',  ( 187.3203125005121024, 0.000000000000000000, 7.632341765625000107 ) ) ;
#16054 = EDGE_LOOP ( 'NONE', ( #120403, #113981, #7982, #40861 ) ) ;
#16055 = ORIENTED_EDGE ( 'NONE', *, *, #44379, .T. ) ;
#16056 = ORIENTED_EDGE ( 'NONE', *, *, #46150, .F. ) ;
#16057 = CARTESIAN_POINT ( 'NONE',  ( -11.89999999999999680, 2.500000000000000000, -0.2464101615137742063 ) ) ;
#16058 = DIRECTION ( 'NONE',  ( 0.000000000000000000, 0.000000000000000000, 1.000000000000000000 ) ) ;
#16059 = DIRECTION ( 'NONE',  ( -4.274815082592931898E-19, -0.9999939076577903929, -0.003490651415223739937 ) ) ;
#16060 = FACE_BOUND ( 'NONE', #74229, .T. ) ;
#16061 = VERTEX_POINT ( 'NONE', #128928 ) ;
#16062 = AXIS2_PLACEMENT_3D ( 'NONE', #5011, #37077, #46234 ) ;
#16063 = CARTESIAN_POINT ( 'NONE',  ( 184.8177083336747160, 4.367472073101515306, 7.564683531250000925 ) ) ;
#16064 = AXIS2_PLACEMENT_3D ( 'NONE', #29, #109994, #110630 ) ;
#16065 = DIRECTION ( 'NONE',  ( 0.000000000000000000, 0.000000000000000000, 1.000000000000000000 ) ) ;
#16066 = FACE_OUTER_BOUND ( 'NONE', #120, .T. ) ;
#16067 = EDGE_CURVE ( 'NONE', #69354, #53159, #106037, .T. ) ;
#16068 = LINE ( 'NONE', #26563, #103407 ) ;
#16069 = AXIS2_PLACEMENT_3D ( 'NONE', #85929, #56474, #36219 ) ;
#16070 = DIRECTION ( 'NONE',  ( 0.000000000000000000, 0.000000000000000000, 1.000000000000000000 ) ) ;
#16071 = CARTESIAN_POINT ( 'NONE',  ( 12.69999999999990337, 12.50000000000000000, -4.676537180435978769 ) ) ;
#16072 = CARTESIAN_POINT ( 'NONE',  ( 13.74999999999989875, 2.500000000000000000, 1.472243186433545459 ) ) ;
#16073 = AXIS2_PLACEMENT_3D ( 'NONE', #17382, #48159, #57332 ) ;
#16074 = DIRECTION ( 'NONE',  ( 0.000000000000000000, -0.9999939076577903929, 0.003490651415223739937 ) ) ;
#16075 = DIRECTION ( 'NONE',  ( 0.000000000000000000, 0.000000000000000000, -1.000000000000000000 ) ) ;
#16076 = CIRCLE ( 'NONE', #32848, 0.1000000000000000056 ) ;
#16077 = ORIENTED_EDGE ( 'NONE', *, *, #31131, .T. ) ;
#16078 = ORIENTED_EDGE ( 'NONE', *, *, #61721, .F. ) ;
#16079 = VERTEX_POINT ( 'NONE', #99451 ) ;
#16080 = ORIENTED_EDGE ( 'NONE', *, *, #9212, .T. ) ;
#16081 = ORIENTED_EDGE ( 'NONE', *, *, #58613, .T. ) ;
#16082 = DIRECTION ( 'NONE',  ( 0.000000000000000000, 0.000000000000000000, 1.000000000000000000 ) ) ;
#16083 = DIRECTION ( 'NONE',  ( -0.000000000000000000, 1.000000000000000000, -0.000000000000000000 ) ) ;
#16084 = VERTEX_POINT ( 'NONE', #108607 ) ;
#16085 = FACE_BOUND ( 'NONE', #66446, .T. ) ;
#16087 = CARTESIAN_POINT ( 'NONE',  ( -11.25000000000000178, 2.500000000000000000, -5.902370205355746968 ) ) ;
#16086 = CONICAL_SURFACE ( 'NONE', #9574, 0.1000000000000002554, 0.003490658503988666988 ) ;
#16089 = CONICAL_SURFACE ( 'NONE', #53679, 0.1000000000000002554, 0.003490658503988666988 ) ;
#16088 = CONICAL_SURFACE ( 'NONE', #53678, 0.1000000000000002554, 0.003490658503988666988 ) ;
#16090 = CARTESIAN_POINT ( 'NONE',  ( 1.899999999999951283, 2.500000000000000000, -0.2464101615137782308 ) ) ;
#16091 = DIRECTION ( 'NONE',  ( 0.000000000000000000, -0.9999939076577903929, 0.003490651415223739937 ) ) ;
#16092 = DIRECTION ( 'NONE',  ( 0.000000000000000000, 0.000000000000000000, 1.000000000000000000 ) ) ;
#16093 = CARTESIAN_POINT ( 'NONE',  ( -5.200000000000022382, 2.500000000000000000, 4.776537180435972196 ) ) ;
#16094 = VERTEX_POINT ( 'NONE', #100710 ) ;
#16095 = CARTESIAN_POINT ( 'NONE',  ( -0.8500000000000395017, 2.500000000000000000, 2.165063509461097713 ) ) ;
#16096 = VERTEX_POINT ( 'NONE', #28122 ) ;
#16097 = ORIENTED_EDGE ( 'NONE', *, *, #18388, .F. ) ;
#16098 = ORIENTED_EDGE ( 'NONE', *, *, #3017, .F. ) ;
#16099 = DIRECTION ( 'NONE',  ( 0.000000000000000000, 0.000000000000000000, 1.000000000000000000 ) ) ;
#16100 = LINE ( 'NONE', #95977, #127932 ) ;
#16101 = CARTESIAN_POINT ( 'NONE',  ( -8.750000000000012434, 12.50000000000000000, -5.802370205355744659 ) ) ;
#16102 = VERTEX_POINT ( 'NONE', #79792 ) ;
#16103 = CONICAL_SURFACE ( 'NONE', #45389, 0.09999999999999982514, 0.003490658503988666988 ) ;
#16104 = DIRECTION ( 'NONE',  ( 0.000000000000000000, 0.000000000000000000, -1.000000000000000000 ) ) ;
#16105 = ADVANCED_FACE ( 'NONE', ( #88305 ), #32902, .T. ) ;
#16106 = CARTESIAN_POINT ( 'NONE',  ( -10.00000000000000533, 2.500000000000000000, 0.6928203230275494784 ) ) ;
#16107 = LINE ( 'NONE', #86138, #122703 ) ;
#16108 = CARTESIAN_POINT ( 'NONE',  ( 184.8645833340161175, -6.668395609140180369, 3.849999999999994760 ) ) ;
#16109 = DIRECTION ( 'NONE',  ( 0.000000000000000000, -0.000000000000000000, 1.000000000000000000 ) ) ;
#16110 = ADVANCED_FACE ( 'NONE', ( #70619 ), #70448, .T. ) ;
#16111 = DIRECTION ( 'NONE',  ( 0.000000000000000000, -0.000000000000000000, 1.000000000000000000 ) ) ;
#16112 = EDGE_CURVE ( 'NONE', #84287, #112495, #20365, .T. ) ;
#16113 = ORIENTED_EDGE ( 'NONE', *, *, #57729, .F. ) ;
#16114 = DIRECTION ( 'NONE',  ( 0.000000000000000000, 0.000000000000000000, -1.000000000000000000 ) ) ;
#16115 = VERTEX_POINT ( 'NONE', #49712 ) ;
#16116 = AXIS2_PLACEMENT_3D ( 'NONE', #10712, #119391, #79494 ) ;
#16117 = ORIENTED_EDGE ( 'NONE', *, *, #124308, .F. ) ;
#16118 = DIRECTION ( 'NONE',  ( 0.000000000000000000, 0.000000000000000000, 1.000000000000000000 ) ) ;
#16119 = EDGE_CURVE ( 'NONE', #80507, #59940, #57928, .T. ) ;
#16120 = EDGE_CURVE ( 'NONE', #23223, #16380, #39258, .T. ) ;
#16121 = CARTESIAN_POINT ( 'NONE',  ( 3.349999999999943689, 12.50000000000000000, 1.472243186433545459 ) ) ;
#16122 = DIRECTION ( 'NONE',  ( -4.274815082592931898E-19, -0.9999939076577903929, -0.003490651415223739937 ) ) ;
#16123 = EDGE_CURVE ( 'NONE', #1020, #12077, #99783, .T. ) ;
#16124 = ORIENTED_EDGE ( 'NONE', *, *, #120664, .T. ) ;
#16127 = EDGE_LOOP ( 'NONE', ( #72186, #18546, #55572, #73590 ) ) ;
#16126 = AXIS2_PLACEMENT_3D ( 'NONE', #2730, #61011, #121226 ) ;
#16125 = AXIS2_PLACEMENT_3D ( 'NONE', #24122, #114420, #4441 ) ;
#16128 = CARTESIAN_POINT ( 'NONE',  ( 129.5000000000000000, 0.000000000000000000, 0.000000000000000000 ) ) ;
#16129 = DIRECTION ( 'NONE',  ( 0.000000000000000000, 0.000000000000000000, -1.000000000000000000 ) ) ;
#16130 = DIRECTION ( 'NONE',  ( 0.000000000000000000, 0.000000000000000000, 1.000000000000000000 ) ) ;
#16131 = VERTEX_POINT ( 'NONE', #118425 ) ;
#16132 = ORIENTED_EDGE ( 'NONE', *, *, #73588, .T. ) ;
#16133 = FACE_OUTER_BOUND ( 'NONE', #76544, .T. ) ;
#16135 = CONICAL_SURFACE ( 'NONE', #74646, 0.1000000000000002554, 0.003490658503988666988 ) ;
#16134 = CIRCLE ( 'NONE', #129057, 0.06509327318403745899 ) ;
#16136 = VERTEX_POINT ( 'NONE', #129573 ) ;
#16137 = DIRECTION ( 'NONE',  ( 0.000000000000000000, 0.000000000000000000, 1.000000000000000000 ) ) ;
#16138 = AXIS2_PLACEMENT_3D ( 'NONE', #88550, #39488, #16572 ) ;
#16139 = CARTESIAN_POINT ( 'NONE',  ( 3.949999999999938005, 2.500000000000000000, 6.741600689897071952 ) ) ;
#16140 = EDGE_LOOP ( 'NONE', ( #75934, #39401, #77897, #51167 ) ) ;
#16141 = FACE_OUTER_BOUND ( 'NONE', #40512, .T. ) ;
#16142 = DIRECTION ( 'NONE',  ( 0.000000000000000000, 1.000000000000000000, 0.000000000000000000 ) ) ;
#16143 = DIRECTION ( 'NONE',  ( 0.000000000000000000, 0.000000000000000000, 1.000000000000000000 ) ) ;
#16144 = CARTESIAN_POINT ( 'NONE',  ( 10.59999999999991260, 12.50000000000000000, 0.4115034346978109769 ) ) ;
#16145 = ORIENTED_EDGE ( 'NONE', *, *, #75659, .T. ) ;
#16147 = AXIS2_PLACEMENT_3D ( 'NONE', #94107, #122698, #63129 ) ;
#16146 = DIRECTION ( 'NONE',  ( 0.000000000000000000, -0.9999939076577903929, 0.003490651415223739937 ) ) ;
#16148 = DIRECTION ( 'NONE',  ( 0.000000000000000000, 0.000000000000000000, 1.000000000000000000 ) ) ;
#16149 = VERTEX_POINT ( 'NONE', #30066 ) ;
#16150 = ORIENTED_EDGE ( 'NONE', *, *, #22020, .F. ) ;
#16151 = CARTESIAN_POINT ( 'NONE',  ( 184.2552083336747444, 6.551208109652275624, -3.782341765624998686 ) ) ;
#16152 = DIRECTION ( 'NONE',  ( -0.000000000000000000, -1.000000000000000000, -0.000000000000000000 ) ) ;
#16153 = DIRECTION ( 'NONE',  ( -0.000000000000000000, 1.000000000000000000, -0.000000000000000000 ) ) ;
#16154 = DIRECTION ( 'NONE',  ( 0.000000000000000000, -0.9999939076577903929, 0.003490651415223739937 ) ) ;
#16155 = CONICAL_SURFACE ( 'NONE', #45441, 0.1000000000000000472, 0.003490658503988666988 ) ;
#16157 = AXIS2_PLACEMENT_3D ( 'NONE', #47631, #90105, #109102 ) ;
#16156 = DIRECTION ( 'NONE',  ( 0.000000000000000000, 1.000000000000000000, 0.000000000000000000 ) ) ;
#16158 = FACE_OUTER_BOUND ( 'NONE', #1531, .T. ) ;
#16159 = AXIS2_PLACEMENT_3D ( 'NONE', #57925, #106994, #97828 ) ;
#16160 = CARTESIAN_POINT ( 'NONE',  ( 17.50000000000000000, -2.500000000000000000, 0.000000000000000000 ) ) ;
#16161 = DIRECTION ( 'NONE',  ( 0.000000000000000000, 1.000000000000000000, 0.000000000000000000 ) ) ;
#16162 = CARTESIAN_POINT ( 'NONE',  ( 3.349999999999945466, 2.500000000000000000, -2.757883832488654097 ) ) ;
#16163 = EDGE_CURVE ( 'NONE', #17352, #104853, #49066, .T. ) ;
#16164 = EDGE_CURVE ( 'NONE', #11168, #93212, #9895, .T. ) ;
#16165 = AXIS2_PLACEMENT_3D ( 'NONE', #119458, #19994, #39015 ) ;
#16166 = EDGE_CURVE ( 'NONE', #868, #58932, #76797, .T. ) ;
#16167 = FACE_OUTER_BOUND ( 'NONE', #104090, .T. ) ;
#16168 = ORIENTED_EDGE ( 'NONE', *, *, #37887, .F. ) ;
#16169 = AXIS2_PLACEMENT_3D ( 'NONE', #75260, #26171, #96181 ) ;
#16170 = AXIS2_PLACEMENT_3D ( 'NONE', #2676, #47140, #47782 ) ;
#16171 = ORIENTED_EDGE ( 'NONE', *, *, #79246, .F. ) ;
#16172 = FACE_OUTER_BOUND ( 'NONE', #45985, .T. ) ;
#16173 = EDGE_CURVE ( 'NONE', #90210, #81351, #83068, .T. ) ;
#16174 = EDGE_LOOP ( 'NONE', ( #30310, #71322 ) ) ;
#16175 = AXIS2_PLACEMENT_3D ( 'NONE', #57531, #39840, #88246 ) ;
#16176 = EDGE_CURVE ( 'NONE', #96180, #77015, #109240, .T. ) ;
#16177 = PLANE ( 'NONE',  #125299 ) ;
#16178 = CARTESIAN_POINT ( 'NONE',  ( -8.100000000000010303, 2.500000000000000000, 4.676537180435972552 ) ) ;
#16179 = DIRECTION ( 'NONE',  ( 0.000000000000000000, 0.000000000000000000, -1.000000000000000000 ) ) ;
#16180 = EDGE_CURVE ( 'NONE', #88083, #4728, #50998, .T. ) ;
#16181 = VERTEX_POINT ( 'NONE', #83036 ) ;
#16182 = EDGE_CURVE ( 'NONE', #118365, #94166, #26618, .T. ) ;
#16183 = DIRECTION ( 'NONE',  ( 0.000000000000000000, 0.000000000000000000, 1.000000000000000000 ) ) ;
#16186 = EDGE_CURVE ( 'NONE', #22692, #19600, #113774, .T. ) ;
#16185 = CONICAL_SURFACE ( 'NONE', #43318, 0.1000000000000002554, 0.003490658503988666988 ) ;
#16184 = VECTOR ( 'NONE', #54000, 1000.000000000000000 ) ;
#16188 = ORIENTED_EDGE ( 'NONE', *, *, #61739, .T. ) ;
#16187 = DIRECTION ( 'NONE',  ( 0.000000000000000000, -0.9999939076577903929, 0.003490651415223739937 ) ) ;
#16189 = APPLICATION_CONTEXT ( 'automotive_design' ) ;
#16190 = EDGE_CURVE ( 'NONE', #45761, #29933, #110155, .T. ) ;
#16191 = DIRECTION ( 'NONE',  ( 0.000000000000000000, 0.000000000000000000, -1.000000000000000000 ) ) ;
#16192 = ORIENTED_EDGE ( 'NONE', *, *, #90792, .T. ) ;
#16193 = ORIENTED_EDGE ( 'NONE', *, *, #8881, .F. ) ;
#16194 = ORIENTED_EDGE ( 'NONE', *, *, #38037, .T. ) ;
#16195 = ORIENTED_EDGE ( 'NONE', *, *, #80922, .F. ) ;
#16196 = CARTESIAN_POINT ( 'NONE',  ( 9.349999999999916156, 2.500000000000000000, -1.718653347947326049 ) ) ;
#16197 = VECTOR ( 'NONE', #46033, 1000.000000000000000 ) ;
#16198 = CARTESIAN_POINT ( 'NONE',  ( 4.799999999999934097, 2.500000000000000000, 4.676537180435972552 ) ) ;
#16199 = DIRECTION ( 'NONE',  ( 0.000000000000000000, 0.000000000000000000, 1.000000000000000000 ) ) ;
#16200 = DIRECTION ( 'NONE',  ( 0.000000000000000000, 0.000000000000000000, 1.000000000000000000 ) ) ;
#16201 = EDGE_LOOP ( 'NONE', ( #89223, #108455, #3643, #45452 ) ) ;
#16202 = CARTESIAN_POINT ( 'NONE',  ( 1.849999999999950573, 2.500000000000000000, 2.411473670974873862 ) ) ;
#16203 = ORIENTED_EDGE ( 'NONE', *, *, #53619, .F. ) ;
#16204 = CARTESIAN_POINT ( 'NONE',  ( -11.04999999999999893, 12.50000000000000000, 1.753560074763284016 ) ) ;
#16205 = CARTESIAN_POINT ( 'NONE',  ( 15.83209681635555022, -2.499999999999998668, -5.404881881984142211 ) ) ;
#16206 = DIRECTION ( 'NONE',  ( -1.000000000000000000, 0.000000000000000000, 0.000000000000000000 ) ) ;
#16207 = CARTESIAN_POINT ( 'NONE',  ( 19.08853762629153294, -0.5565172524004106114, 4.470057054643206129 ) ) ;
#16208 = ORIENTED_EDGE ( 'NONE', *, *, #83305, .F. ) ;
#16209 = CIRCLE ( 'NONE', #35041, 0.06509327318403745899 ) ;
#16210 = CIRCLE ( 'NONE', #122757, 0.06509327318403745899 ) ;
#16211 = EDGE_LOOP ( 'NONE', ( #51531, #65778, #89267, #114530 ) ) ;
#16212 = ORIENTED_EDGE ( 'NONE', *, *, #6761, .F. ) ;
#16213 = DIRECTION ( 'NONE',  ( 0.000000000000000000, 0.000000000000000000, 1.000000000000000000 ) ) ;
#16214 = DIRECTION ( 'NONE',  ( -0.000000000000000000, 1.000000000000000000, -0.000000000000000000 ) ) ;
#16215 = CARTESIAN_POINT ( 'NONE',  ( -3.750000000000026201, 2.500000000000000000, 5.802370205355744659 ) ) ;
#16216 = FACE_BOUND ( 'NONE', #46063, .T. ) ;
#16217 = DIRECTION ( 'NONE',  ( 0.000000000000000000, -0.9999939076577903929, 0.003490651415223739937 ) ) ;
#16218 = CARTESIAN_POINT ( 'NONE',  ( 2.699999999999945555, 12.50000000000000000, 3.983716857408420076 ) ) ;
#16219 = AXIS2_PLACEMENT_3D ( 'NONE', #57876, #116132, #8112 ) ;
#16220 = FACE_OUTER_BOUND ( 'NONE', #62689, .T. ) ;
#16221 = DIRECTION ( 'NONE',  ( 0.000000000000000000, -0.000000000000000000, 1.000000000000000000 ) ) ;
#16222 = AXIS2_PLACEMENT_3D ( 'NONE', #36781, #66855, #108072 ) ;
#16223 = EDGE_CURVE ( 'NONE', #24379, #80231, #11943, .T. ) ;
#16224 = AXIS2_PLACEMENT_3D ( 'NONE', #37964, #89651, #98164 ) ;
#16225 = CARTESIAN_POINT ( 'NONE',  ( 185.3802083336747444, 4.367472073101515306, 7.564683531250000925 ) ) ;
#16226 = FACE_OUTER_BOUND ( 'NONE', #89756, .T. ) ;
#16227 = PLANE ( 'NONE',  #107589 ) ;
#16228 = CONICAL_SURFACE ( 'NONE', #26722, 0.1000000000000002554, 0.003490658503988666988 ) ;
#16229 = DIRECTION ( 'NONE',  ( 0.000000000000000000, 0.000000000000000000, 1.000000000000000000 ) ) ;
#16230 = ORIENTED_EDGE ( 'NONE', *, *, #14597, .F. ) ;
#16231 = ORIENTED_EDGE ( 'NONE', *, *, #86683, .F. ) ;
#16232 = VERTEX_POINT ( 'NONE', #62747 ) ;
#16233 = ORIENTED_EDGE ( 'NONE', *, *, #92540, .F. ) ;
#16234 = AXIS2_PLACEMENT_3D ( 'NONE', #127284, #29092, #59853 ) ;
#16235 = EDGE_CURVE ( 'NONE', #82540, #27061, #113643, .T. ) ;
#16236 = CARTESIAN_POINT ( 'NONE',  ( -13.94999999999998863, 12.50000000000000000, -1.753560074763286458 ) ) ;
#16237 = FACE_BOUND ( 'NONE', #65695, .T. ) ;
#16238 = CARTESIAN_POINT ( 'NONE',  ( 10.84999999999991260, 2.500000000000000000, -2.165063509461101710 ) ) ;
#16239 = AXIS2_PLACEMENT_3D ( 'NONE', #70176, #80646, #42000 ) ;
#16240 = CIRCLE ( 'NONE', #43389, 0.06509327318403745899 ) ;
#16241 = ORIENTED_EDGE ( 'NONE', *, *, #121972, .F. ) ;
#16242 = DIRECTION ( 'NONE',  ( 0.000000000000000000, 1.000000000000000000, 0.000000000000000000 ) ) ;
#16243 = DIRECTION ( 'NONE',  ( 0.000000000000000000, 0.000000000000000000, 1.000000000000000000 ) ) ;
#16244 = AXIS2_PLACEMENT_3D ( 'NONE', #116416, #75849, #16272 ) ;
#16245 = ORIENTED_EDGE ( 'NONE', *, *, #22980, .F. ) ;
#16246 = DIRECTION ( 'NONE',  ( 0.000000000000000000, 0.000000000000000000, 1.000000000000000000 ) ) ;
#16247 = CONICAL_SURFACE ( 'NONE', #28902, 0.1000000000000002554, 0.003490658503988666988 ) ;
#16248 = DIRECTION ( 'NONE',  ( 0.000000000000000000, 0.000000000000000000, 1.000000000000000000 ) ) ;
#16249 = AXIS2_PLACEMENT_3D ( 'NONE', #264, #30414, #50670 ) ;
#16250 = ORIENTED_EDGE ( 'NONE', *, *, #6157, .F. ) ;
#16251 = CARTESIAN_POINT ( 'NONE',  ( -2.900000000000030553, 12.50000000000000000, 5.022947341949748790 ) ) ;
#16252 = DIRECTION ( 'NONE',  ( -4.274815082592931898E-19, -0.9999939076577903929, -0.003490651415223739937 ) ) ;
#16253 = AXIS2_PLACEMENT_3D ( 'NONE', #114020, #122554, #21777 ) ;
#16254 = AXIS2_PLACEMENT_3D ( 'NONE', #2937, #31749, #63132 ) ;
#16255 = ORIENTED_EDGE ( 'NONE', *, *, #114771, .T. ) ;
#16256 = CONICAL_SURFACE ( 'NONE', #47600, 0.09999999999999982514, 0.003490658503988666988 ) ;
#16257 = EDGE_CURVE ( 'NONE', #114814, #78481, #118552, .T. ) ;
#16258 = CARTESIAN_POINT ( 'NONE',  ( 4.599999999999937472, 2.500000000000000000, 0.6928203230275494784 ) ) ;
#16259 = CARTESIAN_POINT ( 'NONE',  ( 9.599999999999914380, 12.50000000000000000, 4.265033745738159077 ) ) ;
#16260 = ORIENTED_EDGE ( 'NONE', *, *, #122033, .F. ) ;
#16261 = CARTESIAN_POINT ( 'NONE',  ( -8.350000000000008527, 2.500000000000000000, 5.902370205355745192 ) ) ;
#16262 = ORIENTED_EDGE ( 'NONE', *, *, #90837, .T. ) ;
#16263 = ORIENTED_EDGE ( 'NONE', *, *, #9374, .T. ) ;
#16264 = CARTESIAN_POINT ( 'NONE',  ( -6.650000000000018119, 2.500000000000000000, -2.857883832488653741 ) ) ;
#16265 = EDGE_CURVE ( 'NONE', #34182, #89915, #85100, .T. ) ;
#16266 = VERTEX_POINT ( 'NONE', #71255 ) ;
#16267 = CARTESIAN_POINT ( 'NONE',  ( 9.999999999999914735, 2.500000000000000000, 0.5928203230275495006 ) ) ;
#16268 = FACE_BOUND ( 'NONE', #76097, .T. ) ;
#16270 = CIRCLE ( 'NONE', #87300, 0.1000000000000002554 ) ;
#16269 = CIRCLE ( 'NONE', #9944, 0.06509327318403743123 ) ;
#16271 = ORIENTED_EDGE ( 'NONE', *, *, #35531, .F. ) ;
#16272 = DIRECTION ( 'NONE',  ( 0.000000000000000000, 0.000000000000000000, -1.000000000000000000 ) ) ;
#16273 = CARTESIAN_POINT ( 'NONE',  ( 10.59999999999990905, 2.500000000000000000, -4.576537180435978236 ) ) ;
#16274 = DIRECTION ( 'NONE',  ( -0.000000000000000000, -1.000000000000000000, -0.000000000000000000 ) ) ;
#16275 = EDGE_CURVE ( 'NONE', #69623, #73823, #78868, .T. ) ;
#16276 = ADVANCED_FACE ( 'NONE', ( #21523 ), #11693, .F. ) ;
#16277 = CARTESIAN_POINT ( 'NONE',  ( -0.4000000000000396572, 2.500000000000000000, 3.537306695894645081 ) ) ;
#16278 = EDGE_CURVE ( 'NONE', #68489, #37844, #63381, .T. ) ;
#16279 = FACE_OUTER_BOUND ( 'NONE', #77365, .T. ) ;
#16280 = EDGE_CURVE ( 'NONE', #12101, #111595, #24099, .T. ) ;
#16281 = EDGE_CURVE ( 'NONE', #47378, #102405, #108083, .T. ) ;
#16282 = FACE_OUTER_BOUND ( 'NONE', #82879, .T. ) ;
#16283 = VERTEX_POINT ( 'NONE', #92851 ) ;
#16284 = ORIENTED_EDGE ( 'NONE', *, *, #51067, .T. ) ;
#16285 = DIRECTION ( 'NONE',  ( 0.000000000000000000, 1.000000000000000000, 0.000000000000000000 ) ) ;
#16286 = DIRECTION ( 'NONE',  ( 0.000000000000000000, 1.000000000000000000, 0.000000000000000000 ) ) ;
#16287 = DIRECTION ( 'NONE',  ( -0.000000000000000000, -1.000000000000000000, -0.000000000000000000 ) ) ;
#16289 = ORIENTED_EDGE ( 'NONE', *, *, #51288, .F. ) ;
#16288 = ORIENTED_EDGE ( 'NONE', *, *, #115585, .T. ) ;
#16290 = ORIENTED_EDGE ( 'NONE', *, *, #36152, .F. ) ;
#16291 = ADVANCED_FACE ( 'NONE', ( #41189 ), #3811, .T. ) ;
#16292 = DIRECTION ( 'NONE',  ( 0.000000000000000000, 0.000000000000000000, -1.000000000000000000 ) ) ;
#16293 = DIRECTION ( 'NONE',  ( 0.000000000000000000, 0.000000000000000000, -1.000000000000000000 ) ) ;
#16294 = EDGE_CURVE ( 'NONE', #85026, #98404, #45410, .T. ) ;
#16295 = CARTESIAN_POINT ( 'NONE',  ( -13.14999999999999147, 2.500000000000000000, -1.818653347947323917 ) ) ;
#16296 = CARTESIAN_POINT ( 'NONE',  ( 0.000000000000000000, 0.000000000000000000, 0.000000000000000000 ) ) ;
#16297 = DIRECTION ( 'NONE',  ( 0.000000000000000000, 0.000000000000000000, -1.000000000000000000 ) ) ;
#16298 = CARTESIAN_POINT ( 'NONE',  ( 8.099999999999921485, 2.500000000000000000, -0.3464101615137783474 ) ) ;
#16299 = DIRECTION ( 'NONE',  ( 0.000000000000000000, -0.000000000000000000, 1.000000000000000000 ) ) ;
#16300 = CARTESIAN_POINT ( 'NONE',  ( -5.850000000000021849, 2.500000000000000000, -5.802370205355749988 ) ) ;
#16301 = DIRECTION ( 'NONE',  ( 0.000000000000000000, 1.000000000000000000, 0.000000000000000000 ) ) ;
#16302 = VECTOR ( 'NONE', #22749, 1000.000000000000000 ) ;
#16303 = LINE ( 'NONE', #67996, #33262 ) ;
#16305 = EDGE_LOOP ( 'NONE', ( #58859, #82297 ) ) ;
#16304 = CIRCLE ( 'NONE', #43538, 0.1000000000000002554 ) ;
#16306 = CIRCLE ( 'NONE', #79039, 0.1000000000000002554 ) ;
#16307 = CARTESIAN_POINT ( 'NONE',  ( 2.099999999999950351, 2.500000000000000000, -4.330127018922201643 ) ) ;
#16308 = ORIENTED_EDGE ( 'NONE', *, *, #125876, .T. ) ;
#16309 = ORIENTED_EDGE ( 'NONE', *, *, #108668, .F. ) ;
#16310 = CARTESIAN_POINT ( 'NONE',  ( -7.300000000000014921, 12.50000000000000000, 4.676537180435972552 ) ) ;
#16311 = CARTESIAN_POINT ( 'NONE',  ( -10.85000000000000142, 2.500000000000000000, -1.472243186433546125 ) ) ;
#16312 = DIRECTION ( 'NONE',  ( 0.000000000000000000, 1.000000000000000000, 0.000000000000000000 ) ) ;
#16313 = DIRECTION ( 'NONE',  ( 0.000000000000000000, 1.000000000000000000, 0.000000000000000000 ) ) ;
#16314 = AXIS2_PLACEMENT_3D ( 'NONE', #9794, #90267, #127633 ) ;
#16315 = LINE ( 'NONE', #46434, #53168 ) ;
#16316 = CARTESIAN_POINT ( 'NONE',  ( -5.850000000000018296, 2.500000000000000000, 1.472243186433545459 ) ) ;
#16317 = EDGE_LOOP ( 'NONE', ( #103915, #98011, #21148, #25835 ) ) ;
#16318 = DIRECTION ( 'NONE',  ( -0.000000000000000000, -1.000000000000000000, -0.000000000000000000 ) ) ;
#16319 = ADVANCED_FACE ( 'NONE', ( #101376 ), #97714, .T. ) ;
#16320 = DIRECTION ( 'NONE',  ( -4.274815082592931898E-19, -0.9999939076577903929, -0.003490651415223739937 ) ) ;
#16321 = ORIENTED_EDGE ( 'NONE', *, *, #81897, .F. ) ;
#16322 = AXIS2_PLACEMENT_3D ( 'NONE', #24819, #52994, #102714 ) ;
#16323 = ORIENTED_EDGE ( 'NONE', *, *, #94092, .T. ) ;
#16324 = EDGE_CURVE ( 'NONE', #65666, #103825, #70527, .T. ) ;
#16325 = EDGE_LOOP ( 'NONE', ( #85807, #111209, #31255, #6898 ) ) ;
#16326 = CIRCLE ( 'NONE', #12227, 0.06509327318403741736 ) ;
#16327 = EDGE_CURVE ( 'NONE', #116425, #89261, #72568, .T. ) ;
#16328 = ORIENTED_EDGE ( 'NONE', *, *, #70791, .T. ) ;
#16329 = DIRECTION ( 'NONE',  ( 0.000000000000000000, 1.000000000000000000, 0.000000000000000000 ) ) ;
#16330 = CARTESIAN_POINT ( 'NONE',  ( -8.350000000000012079, 12.50000000000000000, 1.407149913249508000 ) ) ;
#16331 = EDGE_CURVE ( 'NONE', #56423, #59088, #12334, .T. ) ;
#16332 = CIRCLE ( 'NONE', #89516, 0.06509327318403745899 ) ;
#16333 = DIRECTION ( 'NONE',  ( 0.000000000000000000, -0.9999939076577903929, 0.003490651415223739937 ) ) ;
#16334 = DIRECTION ( 'NONE',  ( 0.000000000000000000, 0.000000000000000000, 1.000000000000000000 ) ) ;
#16335 = EDGE_CURVE ( 'NONE', #111617, #75922, #84301, .T. ) ;
#16336 = FACE_OUTER_BOUND ( 'NONE', #96187, .T. ) ;
#16337 = EDGE_LOOP ( 'NONE', ( #9326, #34903 ) ) ;
#16338 = DIRECTION ( 'NONE',  ( 0.000000000000000000, 1.000000000000000000, 0.000000000000000000 ) ) ;
#16339 = AXIS2_PLACEMENT_3D ( 'NONE', #100989, #38887, #100358 ) ;
#16340 = VECTOR ( 'NONE', #86333, 1000.000000000000000 ) ;
#16341 = EDGE_CURVE ( 'NONE', #19741, #54151, #74743, .T. ) ;
#16342 = CARTESIAN_POINT ( 'NONE',  ( 13.09999999999989839, 12.50000000000000000, 0.4115034346978109769 ) ) ;
#16343 = ORIENTED_EDGE ( 'NONE', *, *, #9236, .T. ) ;
#16344 = VECTOR ( 'NONE', #12511, 1000.000000000000000 ) ;
#16345 = EDGE_LOOP ( 'NONE', ( #41643, #112515 ) ) ;
#16346 = EDGE_LOOP ( 'NONE', ( #28624, #97760, #97602, #62414 ) ) ;
#16347 = CARTESIAN_POINT ( 'NONE',  ( -7.900000000000011013, 2.500000000000000000, 3.637306695894644726 ) ) ;
#16348 = CARTESIAN_POINT ( 'NONE',  ( -8.750000000000008882, 12.50000000000000000, 1.407149913249508000 ) ) ;
#16349 = ORIENTED_EDGE ( 'NONE', *, *, #8051, .F. ) ;
#16350 = DIRECTION ( 'NONE',  ( -0.000000000000000000, -1.000000000000000000, -0.000000000000000000 ) ) ;
#16352 = AXIS2_PLACEMENT_3D ( 'NONE', #121542, #92084, #111063 ) ;
#16351 = LINE ( 'NONE', #56293, #51709 ) ;
#16353 = DIRECTION ( 'NONE',  ( -0.000000000000000000, 1.000000000000000000, -0.000000000000000000 ) ) ;
#16354 = CARTESIAN_POINT ( 'NONE',  ( -9.150000000000005684, 2.500000000000000000, 7.188010851410848723 ) ) ;
#16355 = EDGE_CURVE ( 'NONE', #82690, #71646, #25365, .T. ) ;
#16356 = CARTESIAN_POINT ( 'NONE',  ( -9.400000000000007461, 12.50000000000000000, 4.741630453620009789 ) ) ;
#16357 = ORIENTED_EDGE ( 'NONE', *, *, #28169, .T. ) ;
#16359 = AXIS2_PLACEMENT_3D ( 'NONE', #74502, #122962, #24763 ) ;
#16358 = AXIS2_PLACEMENT_3D ( 'NONE', #107449, #98265, #26964 ) ;
#16360 = FACE_OUTER_BOUND ( 'NONE', #50189, .T. ) ;
#16361 = ORIENTED_EDGE ( 'NONE', *, *, #96035, .F. ) ;
#16362 = ORIENTED_EDGE ( 'NONE', *, *, #74662, .T. ) ;
#16363 = EDGE_LOOP ( 'NONE', ( #4866, #6904, #106559, #118151 ) ) ;
#16364 = DIRECTION ( 'NONE',  ( 0.000000000000000000, 1.000000000000000000, 0.000000000000000000 ) ) ;
#16365 = FACE_BOUND ( 'NONE', #123643, .T. ) ;
#16366 = DIRECTION ( 'NONE',  ( 0.000000000000000000, 1.000000000000000000, 0.000000000000000000 ) ) ;
#16367 = DIRECTION ( 'NONE',  ( 0.000000000000000000, 0.000000000000000000, -1.000000000000000000 ) ) ;
#16368 = CARTESIAN_POINT ( 'NONE',  ( 0.7999999999999548583, 2.500000000000000000, 4.330127018922196314 ) ) ;
#16369 = EDGE_CURVE ( 'NONE', #28068, #90204, #114436, .T. ) ;
#16370 = CIRCLE ( 'NONE', #64510, 0.06509327318403745899 ) ;
#16371 = ORIENTED_EDGE ( 'NONE', *, *, #108457, .F. ) ;
#16372 = DIRECTION ( 'NONE',  ( 0.000000000000000000, 0.000000000000000000, -1.000000000000000000 ) ) ;
#16373 = DIRECTION ( 'NONE',  ( 0.000000000000000000, 0.000000000000000000, 1.000000000000000000 ) ) ;
#16374 = LINE ( 'NONE', #25561, #59113 ) ;
#16375 = DIRECTION ( 'NONE',  ( -0.000000000000000000, 1.000000000000000000, -0.000000000000000000 ) ) ;
#16376 = ORIENTED_EDGE ( 'NONE', *, *, #82253, .F. ) ;
#16377 = LINE ( 'NONE', #49760, #90784 ) ;
#16378 = CARTESIAN_POINT ( 'NONE',  ( 12.49999999999990585, 2.500000000000000000, -5.022947341949754119 ) ) ;
#16379 = VECTOR ( 'NONE', #16776, 1000.000000000000000 ) ;
#16380 = VERTEX_POINT ( 'NONE', #16817 ) ;
#16381 = DIRECTION ( 'NONE',  ( 0.000000000000000000, 1.000000000000000000, 0.000000000000000000 ) ) ;
#16382 = ADVANCED_FACE ( 'NONE', ( #5087 ), #58024, .T. ) ;
#16383 = FACE_BOUND ( 'NONE', #57436, .T. ) ;
#16384 = DIRECTION ( 'NONE',  ( 0.000000000000000000, 0.000000000000000000, 1.000000000000000000 ) ) ;
#16385 = CIRCLE ( 'NONE', #108353, 0.06509327318403745899 ) ;
#16386 = CIRCLE ( 'NONE', #26885, 0.09999999999999982514 ) ;
#16387 = AXIS2_PLACEMENT_3D ( 'NONE', #75939, #54371, #85117 ) ;
#16388 = VERTEX_POINT ( 'NONE', #94766 ) ;
#16389 = DIRECTION ( 'NONE',  ( -0.000000000000000000, -0.000000000000000000, -1.000000000000000000 ) ) ;
#16390 = CARTESIAN_POINT ( 'NONE',  ( -11.84999999999999787, 2.500000000000000000, -6.841600689897074261 ) ) ;
#16391 = EDGE_LOOP ( 'NONE', ( #38360, #33158, #58479, #24184 ) ) ;
#16392 = ORIENTED_EDGE ( 'NONE', *, *, #72633, .F. ) ;
#16393 = CARTESIAN_POINT ( 'NONE',  ( 184.2968750003414300, 8.734944146203032389, 5.348610694689227483E-16 ) ) ;
#16394 = CONICAL_SURFACE ( 'NONE', #89595, 0.1000000000000000472, 0.003490658503988666988 ) ;
#16395 = ORIENTED_EDGE ( 'NONE', *, *, #82551, .T. ) ;
#16396 = CARTESIAN_POINT ( 'NONE',  ( 184.7968750003414584, 8.734944146203032389, 5.348610694689227483E-16 ) ) ;
#16397 = DIRECTION ( 'NONE',  ( -0.000000000000000000, -1.000000000000000000, -0.000000000000000000 ) ) ;
#16398 = DIRECTION ( 'NONE',  ( 0.000000000000000000, 0.000000000000000000, -1.000000000000000000 ) ) ;
#16399 = DIRECTION ( 'NONE',  ( -0.000000000000000000, 1.000000000000000000, -0.000000000000000000 ) ) ;
#16400 = DIRECTION ( 'NONE',  ( -0.000000000000000000, -1.000000000000000000, -0.000000000000000000 ) ) ;
#16401 = CIRCLE ( 'NONE', #45790, 0.1000000000000002554 ) ;
#16402 = EDGE_LOOP ( 'NONE', ( #20389, #124595 ) ) ;
#16403 = EDGE_CURVE ( 'NONE', #40177, #67175, #120705, .T. ) ;
#16404 = CARTESIAN_POINT ( 'NONE',  ( 4.149999999999938183, 2.500000000000000000, 5.802370205355744659 ) ) ;
#16405 = CARTESIAN_POINT ( 'NONE',  ( 6.649999999999930189, 12.50000000000000000, 7.188010851410848723 ) ) ;
#16406 = AXIS2_PLACEMENT_3D ( 'NONE', #108843, #19162, #36907 ) ;
#16407 = DIRECTION ( 'NONE',  ( 0.000000000000000000, 1.000000000000000000, 0.000000000000000000 ) ) ;
#16408 = DIRECTION ( 'NONE',  ( 0.000000000000000000, 1.000000000000000000, 0.000000000000000000 ) ) ;
#16410 = ORIENTED_EDGE ( 'NONE', *, *, #64843, .T. ) ;
#16409 = ORIENTED_EDGE ( 'NONE', *, *, #8631, .T. ) ;
#16411 = FACE_BOUND ( 'NONE', #9562, .T. ) ;
#16412 = VERTEX_POINT ( 'NONE', #94124 ) ;
#16413 = DIRECTION ( 'NONE',  ( -0.000000000000000000, -1.000000000000000000, -0.000000000000000000 ) ) ;
#16414 = LINE ( 'NONE', #74725, #22751 ) ;
#16415 = ORIENTED_EDGE ( 'NONE', *, *, #25968, .T. ) ;
#16417 = EDGE_CURVE ( 'NONE', #12263, #48527, #18294, .T. ) ;
#16416 = DIRECTION ( 'NONE',  ( 0.000000000000000000, 1.000000000000000000, 0.000000000000000000 ) ) ;
#16418 = AXIS2_PLACEMENT_3D ( 'NONE', #43746, #115015, #94743 ) ;
#16419 = CARTESIAN_POINT ( 'NONE',  ( 5.399999999999934630, 12.50000000000000000, -0.6277270498435167934 ) ) ;
#16420 = CARTESIAN_POINT ( 'NONE',  ( 11.24999999999994493, 12.50000000000000000, -2.165063509461101710 ) ) ;
#16421 = CARTESIAN_POINT ( 'NONE',  ( -0.6000000000000388356, 2.500000000000000000, 3.883716857408421319 ) ) ;
#16422 = VERTEX_POINT ( 'NONE', #96052 ) ;
#16423 =( GEOMETRIC_REPRESENTATION_CONTEXT ( 3 ) GLOBAL_UNCERTAINTY_ASSIGNED_CONTEXT ( ( #128254 ) ) GLOBAL_UNIT_ASSIGNED_CONTEXT ( ( #21635, #43225, #83143 ) ) REPRESENTATION_CONTEXT ( 'NONE', 'WORKASPACE' ) );
#16424 = CARTESIAN_POINT ( 'NONE',  ( 9.349999999999919709, 2.500000000000000000, -6.841600689897078702 ) ) ;
#16425 = LINE ( 'NONE', #57008, #16680 ) ;
#16426 = EDGE_CURVE ( 'NONE', #128319, #41444, #30845, .T. ) ;
#16427 = EDGE_CURVE ( 'NONE', #79210, #16232, #64266, .T. ) ;
#16428 = CARTESIAN_POINT ( 'NONE',  ( 0.3999999999999563904, 2.500000000000000000, 5.122947341949749323 ) ) ;
#16429 = CARTESIAN_POINT ( 'NONE',  ( 127.5000000000000000, -1.500000000000000000, -6.000000000000000000 ) ) ;
#16430 = EDGE_CURVE ( 'NONE', #120997, #4440, #36514, .T. ) ;
#16431 = ADVANCED_FACE ( 'NONE', ( #45042 ), #76425, .T. ) ;
#16432 = AXIS2_PLACEMENT_3D ( 'NONE', #57873, #108246, #55288 ) ;
#16433 = LINE ( 'NONE', #77951, #45213 ) ;
#16435 = EDGE_LOOP ( 'NONE', ( #95201, #103654 ) ) ;
#16434 = CONICAL_SURFACE ( 'NONE', #14388, 0.1000000000000002554, 0.003490658503988666988 ) ;
#16436 = ORIENTED_EDGE ( 'NONE', *, *, #21618, .T. ) ;
#16437 = DIRECTION ( 'NONE',  ( 0.000000000000000000, 1.000000000000000000, 0.000000000000000000 ) ) ;
#16439 = ORIENTED_EDGE ( 'NONE', *, *, #59537, .T. ) ;
#16438 = EDGE_CURVE ( 'NONE', #87504, #19669, #98183, .T. ) ;
#16440 = ADVANCED_FACE ( 'NONE', ( #116968 ), #115037, .T. ) ;
#16441 = DIRECTION ( 'NONE',  ( 0.000000000000000000, -0.000000000000000000, 1.000000000000000000 ) ) ;
#16443 = VERTEX_POINT ( 'NONE', #6355 ) ;
#16442 = ORIENTED_EDGE ( 'NONE', *, *, #27611, .T. ) ;
#16444 = EDGE_LOOP ( 'NONE', ( #77980, #19718 ) ) ;
#16445 = CONICAL_SURFACE ( 'NONE', #85420, 0.09999999999999982514, 0.003490658503988666988 ) ;
#16446 = EDGE_CURVE ( 'NONE', #126127, #68087, #46302, .T. ) ;
#16447 = CARTESIAN_POINT ( 'NONE',  ( 2.099999999999949463, 2.500000000000000000, 0.5928203230275495006 ) ) ;
#16448 = ADVANCED_FACE ( 'NONE', ( #95418 ), #10450, .T. ) ;
#16449 = DIRECTION ( 'NONE',  ( 0.000000000000000000, 0.000000000000000000, -1.000000000000000000 ) ) ;
#16450 = EDGE_CURVE ( 'NONE', #14174, #57147, #94081, .T. ) ;
#16451 = DIRECTION ( 'NONE',  ( 0.000000000000000000, 1.000000000000000000, 0.000000000000000000 ) ) ;
#16452 = DIRECTION ( 'NONE',  ( 0.000000000000000000, 0.000000000000000000, 1.000000000000000000 ) ) ;
#16454 = AXIS2_PLACEMENT_3D ( 'NONE', #124274, #83706, #92890 ) ;
#16453 = AXIS2_PLACEMENT_3D ( 'NONE', #119875, #129081, #20392 ) ;
#16455 = CARTESIAN_POINT ( 'NONE',  ( -0.6500000000000403233, 2.500000000000000000, 1.818653347947321475 ) ) ;
#16456 = DIRECTION ( 'NONE',  ( 0.000000000000000000, 0.000000000000000000, -1.000000000000000000 ) ) ;
#16457 = CARTESIAN_POINT ( 'NONE',  ( 13.74999999999989519, 2.500000000000000000, -2.957883832488653830 ) ) ;
#16458 = CIRCLE ( 'NONE', #1789, 0.06509327318403741736 ) ;
#16459 = EDGE_LOOP ( 'NONE', ( #70195, #121954, #13772, #77318 ) ) ;
#16460 = EDGE_CURVE ( 'NONE', #6759, #14824, #125510, .T. ) ;
#16461 = FACE_OUTER_BOUND ( 'NONE', #64567, .T. ) ;
#16462 = EDGE_LOOP ( 'NONE', ( #21789, #62752, #87963, #105308 ) ) ;
#16464 = AXIS2_PLACEMENT_3D ( 'NONE', #124891, #62759, #115047 ) ;
#16463 = CIRCLE ( 'NONE', #81239, 0.1000000000000002554 ) ;
#16465 = ORIENTED_EDGE ( 'NONE', *, *, #55031, .T. ) ;
#16466 = ORIENTED_EDGE ( 'NONE', *, *, #30221, .T. ) ;
#16467 = EDGE_LOOP ( 'NONE', ( #120300, #68805 ) ) ;
#16468 = PLANE ( 'NONE',  #102829 ) ;
#16469 = ORIENTED_EDGE ( 'NONE', *, *, #30069, .F. ) ;
#16470 = VERTEX_POINT ( 'NONE', #32193 ) ;
#16471 = DIRECTION ( 'NONE',  ( -0.000000000000000000, -1.000000000000000000, -0.000000000000000000 ) ) ;
#16472 = FACE_OUTER_BOUND ( 'NONE', #29634, .T. ) ;
#16473 = CARTESIAN_POINT ( 'NONE',  ( -1.900000000000034994, 12.50000000000000000, -0.3464101615137783474 ) ) ;
#16474 = CARTESIAN_POINT ( 'NONE',  ( -4.150000000000025224, 2.500000000000000000, 7.188010851410848723 ) ) ;
#16476 = AXIS2_PLACEMENT_3D ( 'NONE', #2927, #3560, #128840 ) ;
#16475 = CARTESIAN_POINT ( 'NONE',  ( 12.09999999999990550, 2.500000000000000000, 4.430127018922196847 ) ) ;
#16477 = ORIENTED_EDGE ( 'NONE', *, *, #85736, .T. ) ;
#16478 = FACE_OUTER_BOUND ( 'NONE', #78538, .T. ) ;
#16479 = ORIENTED_EDGE ( 'NONE', *, *, #95772, .T. ) ;
#16481 = DIRECTION ( 'NONE',  ( 0.000000000000000000, 1.000000000000000000, 0.000000000000000000 ) ) ;
#16480 = CONICAL_SURFACE ( 'NONE', #83412, 0.09999999999999999167, 0.003490658503988666988 ) ;
#16483 = ORIENTED_EDGE ( 'NONE', *, *, #93932, .T. ) ;
#16482 = CIRCLE ( 'NONE', #29042, 0.1000000000000002554 ) ;
#16484 = DIRECTION ( 'NONE',  ( -0.000000000000000000, 1.000000000000000000, -0.000000000000000000 ) ) ;
#16485 = VERTEX_POINT ( 'NONE', #44568 ) ;
#16486 = ORIENTED_EDGE ( 'NONE', *, *, #80592, .T. ) ;
#16488 = CIRCLE ( 'NONE', #81375, 0.1000000000000002554 ) ;
#16487 = DIRECTION ( 'NONE',  ( 0.000000000000000000, 0.000000000000000000, -1.000000000000000000 ) ) ;
#16489 = FACE_OUTER_BOUND ( 'NONE', #57641, .T. ) ;
#16490 = CONICAL_SURFACE ( 'NONE', #110595, 0.1000000000000002554, 0.003490658503988666988 ) ;
#16491 = ADVANCED_FACE ( 'NONE', ( #51821 ), #62698, .T. ) ;
#16492 = AXIS2_PLACEMENT_3D ( 'NONE', #7619, #47569, #28567 ) ;
#16493 = CARTESIAN_POINT ( 'NONE',  ( 186.0416666666666572, -4.445597072760079982, 7.700000000000070344 ) ) ;
#16494 = FACE_OUTER_BOUND ( 'NONE', #13130, .T. ) ;
#16495 = EDGE_CURVE ( 'NONE', #100499, #76783, #121174, .T. ) ;
#16496 = CARTESIAN_POINT ( 'NONE',  ( -7.950000000000012612, 2.500000000000000000, -2.065063509461102065 ) ) ;
#16497 = ORIENTED_EDGE ( 'NONE', *, *, #120806, .T. ) ;
#16498 = FACE_OUTER_BOUND ( 'NONE', #4929, .T. ) ;
#16499 = DIRECTION ( 'NONE',  ( 0.000000000000000000, 0.000000000000000000, -1.000000000000000000 ) ) ;
#16500 = DIRECTION ( 'NONE',  ( 0.000000000000000000, -0.9999939076577903929, 0.003490651415223739937 ) ) ;
#16501 = DIRECTION ( 'NONE',  ( 0.000000000000000000, 1.000000000000000000, 0.000000000000000000 ) ) ;
#16502 = AXIS2_PLACEMENT_3D ( 'NONE', #53447, #115548, #44911 ) ;
#16503 = ADVANCED_FACE ( 'NONE', ( #94295 ), #60648, .T. ) ;
#16504 = DIRECTION ( 'NONE',  ( -0.000000000000000000, -1.000000000000000000, -0.000000000000000000 ) ) ;
#16505 = AXIS2_PLACEMENT_3D ( 'NONE', #121637, #121002, #81088 ) ;
#16506 = ORIENTED_EDGE ( 'NONE', *, *, #3445, .T. ) ;
#16507 = ORIENTED_EDGE ( 'NONE', *, *, #22412, .F. ) ;
#16508 = CARTESIAN_POINT ( 'NONE',  ( 5.849999999999932143, 12.50000000000000000, 2.165063509461097713 ) ) ;
#16509 = VERTEX_POINT ( 'NONE', #72743 ) ;
#16510 = CARTESIAN_POINT ( 'NONE',  ( 12.69999999999990337, 12.50000000000000000, -4.741630453620016006 ) ) ;
#16512 = CIRCLE ( 'NONE', #93613, 0.06509327318403745899 ) ;
#16511 = DIRECTION ( 'NONE',  ( 0.000000000000000000, -0.000000000000000000, 1.000000000000000000 ) ) ;
#16513 = CIRCLE ( 'NONE', #27007, 0.09999999999999982514 ) ;
#16514 = ORIENTED_EDGE ( 'NONE', *, *, #84758, .T. ) ;
#16515 = CARTESIAN_POINT ( 'NONE',  ( 186.8750000000000284, 8.891194145520236347, 5.444286225454521982E-16 ) ) ;
#16516 = DIRECTION ( 'NONE',  ( 0.000000000000000000, 0.000000000000000000, 1.000000000000000000 ) ) ;
#16517 = DIRECTION ( 'NONE',  ( -0.000000000000000000, -1.000000000000000000, -0.000000000000000000 ) ) ;
#16518 = CARTESIAN_POINT ( 'NONE',  ( -1.900000000000035438, 2.500000000000000000, 3.883716857408420431 ) ) ;
#16519 = CARTESIAN_POINT ( 'NONE',  ( 133.2169897921533845, 2.500000000000000000, -4.655597831175330548 ) ) ;
#16520 = EDGE_LOOP ( 'NONE', ( #51444, #69183, #81002, #20250 ) ) ;
#16521 = DIRECTION ( 'NONE',  ( 0.000000000000000000, 0.000000000000000000, 1.000000000000000000 ) ) ;
#16522 = LINE ( 'NONE', #74181, #93647 ) ;
#16523 = VECTOR ( 'NONE', #65762, 1000.000000000000000 ) ;
#16524 = ORIENTED_EDGE ( 'NONE', *, *, #7482, .T. ) ;
#16525 = DIRECTION ( 'NONE',  ( 0.000000000000000000, 0.000000000000000000, 1.000000000000000000 ) ) ;
#16526 = CARTESIAN_POINT ( 'NONE',  ( 6.249999999999934275, 2.500000000000000000, -7.188010851410854052 ) ) ;
#16527 = DIRECTION ( 'NONE',  ( 0.000000000000000000, 0.000000000000000000, 1.000000000000000000 ) ) ;
#16528 = VECTOR ( 'NONE', #5586, 1000.000000000000000 ) ;
#16529 = VERTEX_POINT ( 'NONE', #121827 ) ;
#16530 = CARTESIAN_POINT ( 'NONE',  ( -3.750000000000026201, 12.50000000000000000, 5.867463478539781896 ) ) ;
#16531 = VERTEX_POINT ( 'NONE', #11868 ) ;
#16533 = VECTOR ( 'NONE', #65063, 1000.000000000000000 ) ;
#16532 = DIRECTION ( 'NONE',  ( 0.000000000000000000, 1.000000000000000000, 0.000000000000000000 ) ) ;
#16534 = FACE_OUTER_BOUND ( 'NONE', #44425, .T. ) ;
#16535 = CARTESIAN_POINT ( 'NONE',  ( 5.199999999999931788, 12.50000000000000000, 4.676537180435972552 ) ) ;
#16536 = ORIENTED_EDGE ( 'NONE', *, *, #4412, .F. ) ;
#16537 = DIRECTION ( 'NONE',  ( 0.000000000000000000, 0.000000000000000000, 1.000000000000000000 ) ) ;
#16539 = AXIS2_PLACEMENT_3D ( 'NONE', #86256, #18172, #97381 ) ;
#16538 = CIRCLE ( 'NONE', #125322, 0.1000000000000002554 ) ;
#16540 = CARTESIAN_POINT ( 'NONE',  ( 11.64999999999990798, 12.50000000000000000, -2.857883832488653741 ) ) ;
#16541 = EDGE_CURVE ( 'NONE', #125237, #51279, #34108, .T. ) ;
#16542 = CIRCLE ( 'NONE', #20778, 0.06509327318403745899 ) ;
#16543 = VERTEX_POINT ( 'NONE', #52443 ) ;
#16544 = EDGE_CURVE ( 'NONE', #82135, #97220, #55161, .T. ) ;
#16545 = EDGE_LOOP ( 'NONE', ( #95098, #29187, #61582, #6561 ) ) ;
#16546 = DIRECTION ( 'NONE',  ( 0.000000000000000000, 0.000000000000000000, 1.000000000000000000 ) ) ;
#16548 = CONICAL_SURFACE ( 'NONE', #125240, 0.1000000000000002554, 0.003490658503988666988 ) ;
#16547 = AXIS2_PLACEMENT_3D ( 'NONE', #113752, #54184, #124852 ) ;
#16549 = VERTEX_POINT ( 'NONE', #111347 ) ;
#16550 = DIRECTION ( 'NONE',  ( 0.000000000000000000, 0.000000000000000000, 1.000000000000000000 ) ) ;
#16551 = CARTESIAN_POINT ( 'NONE',  ( 6.049999999999932321, 2.500000000000000000, -1.818653347947326138 ) ) ;
#16552 = ORIENTED_EDGE ( 'NONE', *, *, #105207, .T. ) ;
#16553 = EDGE_CURVE ( 'NONE', #122658, #31101, #102207, .T. ) ;
#16554 = ORIENTED_EDGE ( 'NONE', *, *, #30060, .T. ) ;
#16555 = CARTESIAN_POINT ( 'NONE',  ( 7.899999999999924860, 2.500000000000000000, -5.022947341949754119 ) ) ;
#16556 = CARTESIAN_POINT ( 'NONE',  ( -3.300000000000027800, 2.500000000000000000, -0.1000000000000022815 ) ) ;
#16557 = VERTEX_POINT ( 'NONE', #93667 ) ;
#16558 = DIRECTION ( 'NONE',  ( 0.000000000000000000, 1.000000000000000000, 0.000000000000000000 ) ) ;
#16559 = FACE_BOUND ( 'NONE', #42887, .T. ) ;
#16560 = PLANE ( 'NONE',  #7496 ) ;
#16561 = CONICAL_SURFACE ( 'NONE', #45839, 0.1000000000000000472, 0.003490658503988666988 ) ;
#16562 = LINE ( 'NONE', #104324, #48735 ) ;
#16563 = DIRECTION ( 'NONE',  ( 0.000000000000000000, -0.000000000000000000, 1.000000000000000000 ) ) ;
#16564 = CARTESIAN_POINT ( 'NONE',  ( 185.1562500006828031, 8.891194145520236347, 5.444286225454521982E-16 ) ) ;
#16565 = AXIS2_PLACEMENT_3D ( 'NONE', #2502, #11698, #100713 ) ;
#16566 = CIRCLE ( 'NONE', #39610, 0.06509327318403741736 ) ;
#16567 = ORIENTED_EDGE ( 'NONE', *, *, #111498, .T. ) ;
#16569 = ORIENTED_EDGE ( 'NONE', *, *, #29039, .T. ) ;
#16568 = EDGE_CURVE ( 'NONE', #33416, #14153, #125380, .T. ) ;
#16570 = ORIENTED_EDGE ( 'NONE', *, *, #28964, .T. ) ;
#16571 = ORIENTED_EDGE ( 'NONE', *, *, #116165, .T. ) ;
#16572 = DIRECTION ( 'NONE',  ( 0.000000000000000000, 0.000000000000000000, 1.000000000000000000 ) ) ;
#16573 = DIRECTION ( 'NONE',  ( -0.000000000000000000, 1.000000000000000000, -0.000000000000000000 ) ) ;
#16574 = CARTESIAN_POINT ( 'NONE',  ( 10.64999999999991331, 2.500000000000000000, -2.611473670974877592 ) ) ;
#16575 = VERTEX_POINT ( 'NONE', #123130 ) ;
#16576 = FACE_BOUND ( 'NONE', #32379, .T. ) ;
#16577 = DIRECTION ( 'NONE',  ( -0.000000000000000000, 1.000000000000000000, -0.000000000000000000 ) ) ;
#16578 = LINE ( 'NONE', #127215, #66811 ) ;
#16579 = AXIS2_PLACEMENT_3D ( 'NONE', #53876, #43434, #93806 ) ;
#16580 = CIRCLE ( 'NONE', #29141, 0.06509327318403745899 ) ;
#16582 = EDGE_CURVE ( 'NONE', #50154, #72001, #82572, .T. ) ;
#16581 = DIRECTION ( 'NONE',  ( 0.000000000000000000, 0.000000000000000000, 1.000000000000000000 ) ) ;
#16583 = CONICAL_SURFACE ( 'NONE', #81378, 0.1000000000000000472, 0.003490658503988666988 ) ;
#16584 = CARTESIAN_POINT ( 'NONE',  ( 3.549999999999943867, 12.50000000000000000, -6.148780366869526226 ) ) ;
#16585 = DIRECTION ( 'NONE',  ( 0.000000000000000000, 1.000000000000000000, 0.000000000000000000 ) ) ;
#16586 = CARTESIAN_POINT ( 'NONE',  ( 3.749999999999942268, 2.500000000000000000, 1.572243186433545548 ) ) ;
#16587 = CARTESIAN_POINT ( 'NONE',  ( 14.79999999999989235, 2.500000000000000000, 0.4464101615137735513 ) ) ;
#16588 = DIRECTION ( 'NONE',  ( 0.000000000000000000, -0.9999939076577903929, 0.003490651415223739937 ) ) ;
#16589 = ADVANCED_FACE ( 'NONE', ( #21710 ), #106589, .T. ) ;
#16590 = EDGE_CURVE ( 'NONE', #51103, #10534, #23632, .T. ) ;
#16591 = DIRECTION ( 'NONE',  ( -0.000000000000000000, 1.000000000000000000, -0.000000000000000000 ) ) ;
#16592 = EDGE_CURVE ( 'NONE', #46680, #68655, #101558, .T. ) ;
#16594 = EDGE_CURVE ( 'NONE', #35122, #21008, #121273, .T. ) ;
#16593 = AXIS2_PLACEMENT_3D ( 'NONE', #31083, #122024, #41546 ) ;
#16595 = CARTESIAN_POINT ( 'NONE',  ( 4.799999999999935874, 2.500000000000000000, 4.083716857408421497 ) ) ;
#16596 = CIRCLE ( 'NONE', #56311, 0.1000000000000002554 ) ;
#16597 = ORIENTED_EDGE ( 'NONE', *, *, #127995, .T. ) ;
#16598 = ORIENTED_EDGE ( 'NONE', *, *, #37486, .T. ) ;
#16599 = VECTOR ( 'NONE', #121836, 1000.000000000000000 ) ;
#16600 = EDGE_LOOP ( 'NONE', ( #35494, #50085 ) ) ;
#16601 = EDGE_LOOP ( 'NONE', ( #97725, #47242 ) ) ;
#16602 = DIRECTION ( 'NONE',  ( 0.000000000000000000, -0.000000000000000000, 1.000000000000000000 ) ) ;
#16603 = EDGE_CURVE ( 'NONE', #101658, #55263, #43292, .T. ) ;
#16604 = FACE_OUTER_BOUND ( 'NONE', #2201, .T. ) ;
#16606 = ORIENTED_EDGE ( 'NONE', *, *, #32285, .T. ) ;
#16605 = EDGE_CURVE ( 'NONE', #74101, #10308, #73370, .T. ) ;
#16607 = VERTEX_POINT ( 'NONE', #83831 ) ;
#16608 = CARTESIAN_POINT ( 'NONE',  ( 2.499999999999945377, 2.500000000000000000, 5.022947341949748790 ) ) ;
#16609 = EDGE_CURVE ( 'NONE', #85331, #86064, #123747, .T. ) ;
#16610 = CARTESIAN_POINT ( 'NONE',  ( 2.899999999999946620, 2.500000000000000000, -3.637306695894650055 ) ) ;
#16611 = CARTESIAN_POINT ( 'NONE',  ( -7.700000000000012612, 2.500000000000000000, 4.676537180435972552 ) ) ;
#16612 = CARTESIAN_POINT ( 'NONE',  ( 11.89999999999990798, 2.500000000000000000, -4.776537180435977525 ) ) ;
#16613 = AXIS2_PLACEMENT_3D ( 'NONE', #20503, #89233, #19177 ) ;
#16614 = CARTESIAN_POINT ( 'NONE',  ( -2.300000000000033573, 2.500000000000000000, 4.576537180435972019 ) ) ;
#16615 = EDGE_CURVE ( 'NONE', #91437, #111265, #89870, .T. ) ;
#16616 = VERTEX_POINT ( 'NONE', #77249 ) ;
#16617 = EDGE_CURVE ( 'NONE', #1046, #124254, #48115, .T. ) ;
#16618 = ORIENTED_EDGE ( 'NONE', *, *, #58112, .T. ) ;
#16619 = ORIENTED_EDGE ( 'NONE', *, *, #36442, .F. ) ;
#16620 = ORIENTED_EDGE ( 'NONE', *, *, #118428, .T. ) ;
#16621 = LINE ( 'NONE', #56551, #71386 ) ;
#16622 = EDGE_LOOP ( 'NONE', ( #120775, #113843, #72183, #124320 ) ) ;
#16623 = ORIENTED_EDGE ( 'NONE', *, *, #67788, .F. ) ;
#16624 = LINE ( 'NONE', #56554, #128066 ) ;
#16625 = DIRECTION ( 'NONE',  ( 0.000000000000000000, 0.000000000000000000, -1.000000000000000000 ) ) ;
#16626 = CARTESIAN_POINT ( 'NONE',  ( -8.750000000000010658, 2.500000000000000000, -1.372243186433550033 ) ) ;
#16627 = DIRECTION ( 'NONE',  ( 0.000000000000000000, 0.000000000000000000, 1.000000000000000000 ) ) ;
#16628 = PLANE ( 'NONE',  #55950 ) ;
#16629 = CIRCLE ( 'NONE', #54219, 0.06509327318403745899 ) ;
#16630 = VERTEX_POINT ( 'NONE', #36696 ) ;
#16631 = DIRECTION ( 'NONE',  ( 0.000000000000000000, 0.000000000000000000, 1.000000000000000000 ) ) ;
#16632 = VERTEX_POINT ( 'NONE', #45219 ) ;
#16633 = DIRECTION ( 'NONE',  ( 0.000000000000000000, 1.000000000000000000, 0.000000000000000000 ) ) ;
#16635 = AXIS2_PLACEMENT_3D ( 'NONE', #10903, #129457, #69865 ) ;
#16634 = AXIS2_PLACEMENT_3D ( 'NONE', #98456, #29736, #89298 ) ;
#16636 = ORIENTED_EDGE ( 'NONE', *, *, #125113, .T. ) ;
#16637 = CARTESIAN_POINT ( 'NONE',  ( 109.3185023437525132, 7.233626197500669264, -4.834355238544921995 ) ) ;
#16638 = DIRECTION ( 'NONE',  ( 0.000000000000000000, 0.000000000000000000, 1.000000000000000000 ) ) ;
#16639 = ORIENTED_EDGE ( 'NONE', *, *, #50196, .T. ) ;
#16640 = VECTOR ( 'NONE', #27072, 1000.000000000000000 ) ;
#16641 = DIRECTION ( 'NONE',  ( 0.000000000000000000, 1.000000000000000000, 0.000000000000000000 ) ) ;
#16642 = LINE ( 'NONE', #46780, #96108 ) ;
#16643 = ORIENTED_EDGE ( 'NONE', *, *, #57575, .T. ) ;
#16645 = VECTOR ( 'NONE', #11875, 1000.000000000000000 ) ;
#16644 = CIRCLE ( 'NONE', #41729, 0.06509327318403745899 ) ;
#16646 = EDGE_CURVE ( 'NONE', #55594, #41939, #68945, .T. ) ;
#16647 = DIRECTION ( 'NONE',  ( 0.000000000000000000, 0.000000000000000000, 1.000000000000000000 ) ) ;
#16648 = EDGE_CURVE ( 'NONE', #100324, #116919, #58508, .T. ) ;
#16649 = EDGE_LOOP ( 'NONE', ( #10638, #91892 ) ) ;
#16650 = ORIENTED_EDGE ( 'NONE', *, *, #103920, .F. ) ;
#16651 = DIRECTION ( 'NONE',  ( 0.000000000000000000, 1.000000000000000000, -1.846105847067148761E-16 ) ) ;
#16652 = DIRECTION ( 'NONE',  ( -0.000000000000000000, -1.000000000000000000, -0.000000000000000000 ) ) ;
#16653 = CARTESIAN_POINT ( 'NONE',  ( 185.8802083336747444, 4.367472073101515306, 7.564683531250000925 ) ) ;
#16654 = CARTESIAN_POINT ( 'NONE',  ( -8.100000000000013856, 2.500000000000000000, -4.083716857408426826 ) ) ;
#16655 = FACE_OUTER_BOUND ( 'NONE', #70257, .T. ) ;
#16656 = DIRECTION ( 'NONE',  ( 0.000000000000000000, 0.000000000000000000, 1.000000000000000000 ) ) ;
#16657 = ORIENTED_EDGE ( 'NONE', *, *, #44132, .T. ) ;
#16658 = LINE ( 'NONE', #87338, #50692 ) ;
#16659 = CONICAL_SURFACE ( 'NONE', #8354, 0.09999999999999982514, 0.003490658503988666988 ) ;
#16660 = CONICAL_SURFACE ( 'NONE', #2005, 0.1000000000000000472, 0.003490658503988666988 ) ;
#16661 = EDGE_LOOP ( 'NONE', ( #90317, #84106, #126959, #20929 ) ) ;
#16662 = DIRECTION ( 'NONE',  ( 0.000000000000000000, 0.000000000000000000, 1.000000000000000000 ) ) ;
#16663 = CARTESIAN_POINT ( 'NONE',  ( 6.449999999999928235, 2.500000000000000000, 2.611473670974873151 ) ) ;
#16664 = DIRECTION ( 'NONE',  ( -0.000000000000000000, -1.000000000000000000, -0.000000000000000000 ) ) ;
#16665 = CARTESIAN_POINT ( 'NONE',  ( 13.29999999999990301, 2.500000000000000000, -4.230127018922201998 ) ) ;
#16666 = ORIENTED_EDGE ( 'NONE', *, *, #82999, .F. ) ;
#16668 = VECTOR ( 'NONE', #76046, 1000.000000000000000 ) ;
#16667 = CIRCLE ( 'NONE', #112842, 0.06509327318403745899 ) ;
#16669 = DIRECTION ( 'NONE',  ( -0.000000000000000000, 1.000000000000000000, -0.000000000000000000 ) ) ;
#16670 = DIRECTION ( 'NONE',  ( -0.000000000000000000, 1.000000000000000000, -0.000000000000000000 ) ) ;
#16671 = AXIS2_PLACEMENT_3D ( 'NONE', #94989, #5296, #75331 ) ;
#16672 = ORIENTED_EDGE ( 'NONE', *, *, #76784, .T. ) ;
#16673 = DIRECTION ( 'NONE',  ( 0.000000000000000000, 0.000000000000000000, -1.000000000000000000 ) ) ;
#16675 = ADVANCED_FACE ( 'NONE', ( #126999 ), #29253, .T. ) ;
#16674 = AXIS2_PLACEMENT_3D ( 'NONE', #117276, #125200, #75441 ) ;
#16676 = AXIS2_PLACEMENT_3D ( 'NONE', #15742, #63577, #5910 ) ;
#16677 = ORIENTED_EDGE ( 'NONE', *, *, #12461, .T. ) ;
#16678 = ORIENTED_EDGE ( 'NONE', *, *, #113396, .T. ) ;
#16679 = CARTESIAN_POINT ( 'NONE',  ( 13.09999999999989839, 2.500000000000000000, 0.4464101615137735513 ) ) ;
#16680 = VECTOR ( 'NONE', #89069, 1000.000000000000000 ) ;
#16681 = ORIENTED_EDGE ( 'NONE', *, *, #19986, .T. ) ;
#16682 = DIRECTION ( 'NONE',  ( 0.000000000000000000, 1.000000000000000000, 0.000000000000000000 ) ) ;
#16683 = DIRECTION ( 'NONE',  ( -4.274815082592931898E-19, -0.9999939076577903929, -0.003490651415223739937 ) ) ;
#16684 = VECTOR ( 'NONE', #13797, 1000.000000000000000 ) ;
#16685 = CARTESIAN_POINT ( 'NONE',  ( -12.29999999999999361, 2.500000000000000000, 3.983716857408420076 ) ) ;
#16686 = EDGE_CURVE ( 'NONE', #45115, #68393, #37656, .T. ) ;
#16687 = VERTEX_POINT ( 'NONE', #126351 ) ;
#16688 = FACE_BOUND ( 'NONE', #90500, .T. ) ;
#16690 = VERTEX_POINT ( 'NONE', #37340 ) ;
#16689 = CARTESIAN_POINT ( 'NONE',  ( -7.700000000000014388, 12.50000000000000000, -0.2813168883297408329 ) ) ;
#16691 = AXIS2_PLACEMENT_3D ( 'NONE', #104768, #35419, #73389 ) ;
#16692 = EDGE_CURVE ( 'NONE', #102068, #81635, #7849, .T. ) ;
#16693 = CARTESIAN_POINT ( 'NONE',  ( 9.149999999999916866, 2.500000000000000000, 7.088010851410848190 ) ) ;
#16694 = LINE ( 'NONE', #116197, #42580 ) ;
#16695 = ADVANCED_FACE ( 'NONE', ( #87056 ), #25037, .T. ) ;
#16696 = EDGE_LOOP ( 'NONE', ( #90752, #119802, #97487, #87277 ) ) ;
#16697 = ORIENTED_EDGE ( 'NONE', *, *, #3181, .T. ) ;
#16698 = ORIENTED_EDGE ( 'NONE', *, *, #8733, .F. ) ;
#16699 = CARTESIAN_POINT ( 'NONE',  ( 14.59999999999989484, 12.50000000000000000, -0.6928203230275541413 ) ) ;
#16700 = CARTESIAN_POINT ( 'NONE',  ( -6.249999999999984901, 2.500000000000000000, -2.265063509461101798 ) ) ;
#16701 = DIRECTION ( 'NONE',  ( -0.000000000000000000, 1.000000000000000000, -0.000000000000000000 ) ) ;
#16702 = EDGE_CURVE ( 'NONE', #120532, #80728, #54363, .T. ) ;
#16703 = FACE_BOUND ( 'NONE', #29135, .T. ) ;
#16704 = EDGE_LOOP ( 'NONE', ( #22045, #13249, #50877, #119234 ) ) ;
#16705 = CARTESIAN_POINT ( 'NONE',  ( 185.2760416670080588, 6.551208109652274736, 3.782341765625001351 ) ) ;
#16706 = CARTESIAN_POINT ( 'NONE',  ( 9.349999999999919709, 12.50000000000000000, -6.148780366869526226 ) ) ;
#16707 = CARTESIAN_POINT ( 'NONE',  ( -7.100000000000017408, 2.500000000000000000, -5.122947341949753763 ) ) ;
#16708 = DIRECTION ( 'NONE',  ( -0.000000000000000000, -1.000000000000000000, -0.000000000000000000 ) ) ;
#16709 = DIRECTION ( 'NONE',  ( 0.000000000000000000, 0.000000000000000000, 1.000000000000000000 ) ) ;
#16710 = PLANE ( 'NONE',  #92537 ) ;
#16711 = AXIS2_PLACEMENT_3D ( 'NONE', #115123, #96788, #35321 ) ;
#16712 = PLANE ( 'NONE',  #3225 ) ;
#16713 = DIRECTION ( 'NONE',  ( -0.000000000000000000, 1.000000000000000000, -0.000000000000000000 ) ) ;
#16715 = CONICAL_SURFACE ( 'NONE', #2063, 0.1000000000000002554, 0.003490658503988666988 ) ;
#16714 = VECTOR ( 'NONE', #86722, 1000.000000000000000 ) ;
#16716 = ORIENTED_EDGE ( 'NONE', *, *, #62285, .T. ) ;
#16717 = ORIENTED_EDGE ( 'NONE', *, *, #69111, .F. ) ;
#16718 = VERTEX_POINT ( 'NONE', #116517 ) ;
#16719 = ORIENTED_EDGE ( 'NONE', *, *, #27662, .F. ) ;
#16720 = VERTEX_POINT ( 'NONE', #35397 ) ;
#16721 = CARTESIAN_POINT ( 'NONE',  ( -10.00000000000000533, 12.50000000000000000, 5.088040615133786027 ) ) ;
#16722 = CARTESIAN_POINT ( 'NONE',  ( 7.949999999999922018, 2.500000000000000000, -2.265063509461101798 ) ) ;
#16723 = VERTEX_POINT ( 'NONE', #56935 ) ;
#16724 = FACE_BOUND ( 'NONE', #77246, .T. ) ;
#16725 = DIRECTION ( 'NONE',  ( 0.000000000000000000, 1.000000000000000000, 0.000000000000000000 ) ) ;
#16727 = AXIS2_PLACEMENT_3D ( 'NONE', #66773, #106698, #87062 ) ;
#16726 = AXIS2_PLACEMENT_3D ( 'NONE', #57079, #85887, #36175 ) ;
#16728 = ADVANCED_FACE ( 'NONE', ( #96876 ), #47796, .T. ) ;
#16729 = CARTESIAN_POINT ( 'NONE',  ( -2.100000000000033840, 2.500000000000000000, 3.737306695894644371 ) ) ;
#16730 = CARTESIAN_POINT ( 'NONE',  ( 2.500000000000002220, -1.500000000000000000, 10.00000000000000178 ) ) ;
#16731 = DIRECTION ( 'NONE',  ( 0.000000000000000000, 1.000000000000000000, 0.000000000000000000 ) ) ;
#16732 = EDGE_CURVE ( 'NONE', #50402, #113932, #31400, .T. ) ;
#16733 = LINE ( 'NONE', #16093, #83019 ) ;
#16734 = ORIENTED_EDGE ( 'NONE', *, *, #57247, .F. ) ;
#16735 = DIRECTION ( 'NONE',  ( 0.000000000000000000, 1.000000000000000000, 0.000000000000000000 ) ) ;
#16736 = ADVANCED_FACE ( 'NONE', ( #87700 ), #75203, .T. ) ;
#16737 = VERTEX_POINT ( 'NONE', #66769 ) ;
#16738 = EDGE_LOOP ( 'NONE', ( #59294, #4799, #86621, #105705 ) ) ;
#16739 = ORIENTED_EDGE ( 'NONE', *, *, #89317, .F. ) ;
#16740 = EDGE_CURVE ( 'NONE', #10395, #2451, #2035, .T. ) ;
#16741 = LINE ( 'NONE', #39025, #119559 ) ;
#16743 = EDGE_CURVE ( 'NONE', #41301, #52849, #52230, .T. ) ;
#16742 = DIRECTION ( 'NONE',  ( 0.000000000000000000, -0.000000000000000000, 1.000000000000000000 ) ) ;
#16744 = DIRECTION ( 'NONE',  ( 0.000000000000000000, -0.000000000000000000, 1.000000000000000000 ) ) ;
#16746 = EDGE_LOOP ( 'NONE', ( #19005, #23209, #98715, #56108 ) ) ;
#16745 = EDGE_CURVE ( 'NONE', #84287, #53425, #95601, .T. ) ;
#16747 = DIRECTION ( 'NONE',  ( 0.000000000000000000, 0.000000000000000000, -1.000000000000000000 ) ) ;
#16748 = EDGE_CURVE ( 'NONE', #18481, #45029, #48199, .T. ) ;
#16749 = AXIS2_PLACEMENT_3D ( 'NONE', #78487, #107921, #87626 ) ;
#16750 = DIRECTION ( 'NONE',  ( -1.000000000000000000, -0.000000000000000000, -0.000000000000000000 ) ) ;
#16751 = AXIS2_PLACEMENT_3D ( 'NONE', #118673, #88572, #78777 ) ;
#16753 = EDGE_CURVE ( 'NONE', #69211, #27373, #108738, .T. ) ;
#16752 = CARTESIAN_POINT ( 'NONE',  ( 1.649999999999950617, 2.500000000000000000, 2.065063509461097624 ) ) ;
#16754 = CARTESIAN_POINT ( 'NONE',  ( 187.0677083336747444, -4.367472073101514418, -7.564683531250002702 ) ) ;
#16755 = DIRECTION ( 'NONE',  ( 0.000000000000000000, 0.000000000000000000, 1.000000000000000000 ) ) ;
#16756 = DIRECTION ( 'NONE',  ( 0.000000000000000000, 1.000000000000000000, 0.000000000000000000 ) ) ;
#16757 = CARTESIAN_POINT ( 'NONE',  ( 10.64999999999991331, 2.500000000000000000, 6.248780366869521430 ) ) ;
#16758 = ORIENTED_EDGE ( 'NONE', *, *, #126734, .T. ) ;
#16759 = CARTESIAN_POINT ( 'NONE',  ( -12.09999999999999609, 2.500000000000000000, 1.734723475976807094E-15 ) ) ;
#16760 = ADVANCED_FACE ( 'NONE', ( #127634 ), #37965, .T. ) ;
#16761 = EDGE_LOOP ( 'NONE', ( #111456, #11193 ) ) ;
#16762 = ORIENTED_EDGE ( 'NONE', *, *, #65044, .F. ) ;
#16763 = CARTESIAN_POINT ( 'NONE',  ( -6.050000000000018474, 2.500000000000000000, 2.511473670974873507 ) ) ;
#16764 = CARTESIAN_POINT ( 'NONE',  ( -7.100000000000017408, 2.500000000000000000, -4.922947341949753586 ) ) ;
#16765 = LINE ( 'NONE', #95363, #92705 ) ;
#16766 = CIRCLE ( 'NONE', #33538, 0.06509327318403745899 ) ;
#16767 = ORIENTED_EDGE ( 'NONE', *, *, #29954, .T. ) ;
#16768 = EDGE_LOOP ( 'NONE', ( #111242, #28770, #32355, #102578 ) ) ;
#16769 = CONICAL_SURFACE ( 'NONE', #27334, 0.09999999999999982514, 0.003490658503988666988 ) ;
#16770 = CARTESIAN_POINT ( 'NONE',  ( 184.8645833340161175, -6.668395609140180369, 3.849999999999994760 ) ) ;
#16771 = CIRCLE ( 'NONE', #83708, 0.06509327318403745899 ) ;
#16772 = CARTESIAN_POINT ( 'NONE',  ( -10.65000000000000391, 12.50000000000000000, -6.083687093685485436 ) ) ;
#16773 = CARTESIAN_POINT ( 'NONE',  ( 15.39999999999989200, 12.50000000000000000, -0.6928203230275542523 ) ) ;
#16774 = ORIENTED_EDGE ( 'NONE', *, *, #64312, .T. ) ;
#16775 = ORIENTED_EDGE ( 'NONE', *, *, #93254, .T. ) ;
#16776 = DIRECTION ( 'NONE',  ( -4.274815082592931898E-19, -0.9999939076577903929, -0.003490651415223739937 ) ) ;
#16777 = AXIS2_PLACEMENT_3D ( 'NONE', #71282, #43155, #11727 ) ;
#16778 = VERTEX_POINT ( 'NONE', #19621 ) ;
#16779 = FACE_OUTER_BOUND ( 'NONE', #90509, .T. ) ;
#16780 = DIRECTION ( 'NONE',  ( 0.000000000000000000, 0.000000000000000000, 1.000000000000000000 ) ) ;
#16781 = VERTEX_POINT ( 'NONE', #9151 ) ;
#16782 = CARTESIAN_POINT ( 'NONE',  ( 8.149999999999923972, 2.500000000000000000, 1.818653347947321475 ) ) ;
#16783 = LINE ( 'NONE', #96636, #2390 ) ;
#16784 = AXIS2_PLACEMENT_3D ( 'NONE', #93686, #4629, #43951 ) ;
#16785 = DIRECTION ( 'NONE',  ( 0.000000000000000000, -0.000000000000000000, 1.000000000000000000 ) ) ;
#16786 = DIRECTION ( 'NONE',  ( -0.000000000000000000, 1.000000000000000000, -0.000000000000000000 ) ) ;
#16787 = VERTEX_POINT ( 'NONE', #18316 ) ;
#16788 = DIRECTION ( 'NONE',  ( 0.000000000000000000, 0.000000000000000000, 1.000000000000000000 ) ) ;
#16789 = EDGE_CURVE ( 'NONE', #122997, #79131, #29342, .T. ) ;
#16790 = DIRECTION ( 'NONE',  ( -0.000000000000000000, -1.000000000000000000, -0.000000000000000000 ) ) ;
#16791 = ORIENTED_EDGE ( 'NONE', *, *, #56745, .F. ) ;
#16792 = EDGE_LOOP ( 'NONE', ( #96318, #64009 ) ) ;
#16793 = FACE_OUTER_BOUND ( 'NONE', #115796, .T. ) ;
#16794 = CARTESIAN_POINT ( 'NONE',  ( -11.44999999999999751, 2.500000000000000000, 6.741600689897071952 ) ) ;
#16795 = CARTESIAN_POINT ( 'NONE',  ( -4.150000000000025224, 12.50000000000000000, 5.737276932171707422 ) ) ;
#16796 = DIRECTION ( 'NONE',  ( 0.000000000000000000, 0.000000000000000000, -1.000000000000000000 ) ) ;
#16797 = CARTESIAN_POINT ( 'NONE',  ( -7.900000000000014566, 12.50000000000000000, -0.6928203230275541413 ) ) ;
#16798 = DIRECTION ( 'NONE',  ( -0.000000000000000000, -1.000000000000000000, -0.000000000000000000 ) ) ;
#16799 = ADVANCED_FACE ( 'NONE', ( #88330 ), #52315, .T. ) ;
#16800 = CARTESIAN_POINT ( 'NONE',  ( -6.650000000000018119, 12.50000000000000000, -2.857883832488653741 ) ) ;
#16801 = DIRECTION ( 'NONE',  ( 0.000000000000000000, 0.000000000000000000, 1.000000000000000000 ) ) ;
#16802 = CARTESIAN_POINT ( 'NONE',  ( 8.949999999999921130, 12.50000000000000000, -6.776507416713040577 ) ) ;
#16803 = AXIS2_PLACEMENT_3D ( 'NONE', #2300, #2971, #21984 ) ;
#16804 = AXIS2_PLACEMENT_3D ( 'NONE', #38400, #98557, #107099 ) ;
#16805 = CARTESIAN_POINT ( 'NONE',  ( 13.74999999999993427, 12.50000000000000000, 2.165063509461097713 ) ) ;
#16806 = ORIENTED_EDGE ( 'NONE', *, *, #40239, .T. ) ;
#16807 = AXIS2_PLACEMENT_3D ( 'NONE', #80786, #20567, #121332 ) ;
#16808 = ORIENTED_EDGE ( 'NONE', *, *, #91572, .T. ) ;
#16809 = DIRECTION ( 'NONE',  ( 0.000000000000000000, 1.000000000000000000, 0.000000000000000000 ) ) ;
#16810 = ORIENTED_EDGE ( 'NONE', *, *, #4734, .F. ) ;
#16811 = LINE ( 'NONE', #54824, #91748 ) ;
#16812 = DIRECTION ( 'NONE',  ( -0.000000000000000000, 1.000000000000000000, -0.000000000000000000 ) ) ;
#16813 = CARTESIAN_POINT ( 'NONE',  ( 187.5000000000000000, 1.375000000000002442, -7.576237522675751457 ) ) ;
#16814 = ORIENTED_EDGE ( 'NONE', *, *, #95210, .F. ) ;
#16815 = CARTESIAN_POINT ( 'NONE',  ( 19.01901804971413767, -2.576149587736929369, -2.431039412660861210 ) ) ;
#16816 = CARTESIAN_POINT ( 'NONE',  ( 13.54999999999990123, 2.500000000000000000, 1.818653347947321475 ) ) ;
#16818 = ORIENTED_EDGE ( 'NONE', *, *, #13017, .T. ) ;
#16817 = CARTESIAN_POINT ( 'NONE',  ( -2.500000000000032419, 2.500000000000000000, 0.5928203230275495006 ) ) ;
#16819 = DIRECTION ( 'NONE',  ( 0.000000000000000000, 1.000000000000000000, 0.000000000000000000 ) ) ;
#16820 = ORIENTED_EDGE ( 'NONE', *, *, #127155, .F. ) ;
#16821 = EDGE_CURVE ( 'NONE', #8340, #87068, #83716, .T. ) ;
#16822 = ORIENTED_EDGE ( 'NONE', *, *, #96975, .F. ) ;
#16823 = VERTEX_POINT ( 'NONE', #48431 ) ;
#16824 = ORIENTED_EDGE ( 'NONE', *, *, #109684, .F. ) ;
#16825 = CARTESIAN_POINT ( 'NONE',  ( 5.199999999999933564, 2.500000000000000000, 0.3464101615137735735 ) ) ;
#16826 = CARTESIAN_POINT ( 'NONE',  ( -0.2000000000000412836, 2.500000000000000000, 4.676537180435972552 ) ) ;
#16827 = CARTESIAN_POINT ( 'NONE',  ( 129.5000000000000000, 0.6250000000000003331, 6.000000000000000000 ) ) ;
#16828 = DIRECTION ( 'NONE',  ( 0.000000000000000000, 1.000000000000000000, 0.000000000000000000 ) ) ;
#16829 = EDGE_CURVE ( 'NONE', #71159, #79454, #9796, .T. ) ;
#16830 = ORIENTED_EDGE ( 'NONE', *, *, #104618, .T. ) ;
#16831 = CONICAL_SURFACE ( 'NONE', #60870, 0.1000000000000000056, 0.003490658503988666988 ) ;
#16832 = DIRECTION ( 'NONE',  ( 0.000000000000000000, 0.000000000000000000, 1.000000000000000000 ) ) ;
#16833 = VERTEX_POINT ( 'NONE', #10437 ) ;
#16834 = LINE ( 'NONE', #115706, #30844 ) ;
#16835 = DIRECTION ( 'NONE',  ( 0.000000000000000000, 1.000000000000000000, 0.000000000000000000 ) ) ;
#16836 = ADVANCED_FACE ( 'NONE', ( #89009 ), #73244, .T. ) ;
#16837 = CARTESIAN_POINT ( 'NONE',  ( 6.449999999999930012, 2.500000000000000000, -1.918653347947326004 ) ) ;
#16838 = CARTESIAN_POINT ( 'NONE',  ( 19.72570408286438592, -0.6078483229322464432, 4.299616118078763094 ) ) ;
#16839 = ADVANCED_FACE ( 'NONE', ( #58266 ), #60729, .T. ) ;
#16840 = CIRCLE ( 'NONE', #35667, 0.09999999999999999167 ) ;
#16841 = EDGE_LOOP ( 'NONE', ( #8665, #74626 ) ) ;
#16842 = VERTEX_POINT ( 'NONE', #99481 ) ;
#16843 = EDGE_CURVE ( 'NONE', #7520, #47255, #87885, .T. ) ;
#16844 = ORIENTED_EDGE ( 'NONE', *, *, #128399, .F. ) ;
#16845 = CARTESIAN_POINT ( 'NONE',  ( 7.299999999999927880, 2.500000000000000000, 3.983716857408420964 ) ) ;
#16846 = PLANE ( 'NONE',  #72771 ) ;
#16847 = FACE_OUTER_BOUND ( 'NONE', #94627, .T. ) ;
#16848 = ADVANCED_FACE ( 'NONE', ( #40575 ), #10531, .T. ) ;
#16849 = FACE_BOUND ( 'NONE', #12362, .T. ) ;
#16850 = CARTESIAN_POINT ( 'NONE',  ( 0.1999999999999571565, 2.500000000000000000, 3.883716857408420431 ) ) ;
#16851 = DIRECTION ( 'NONE',  ( 0.000000000000000000, 1.000000000000000000, 0.000000000000000000 ) ) ;
#16852 = DIRECTION ( 'NONE',  ( 0.000000000000000000, 1.000000000000000000, 0.000000000000000000 ) ) ;
#16853 = CARTESIAN_POINT ( 'NONE',  ( 7.299999999999927880, 12.50000000000000000, -4.676537180435977881 ) ) ;
#16854 = AXIS2_PLACEMENT_3D ( 'NONE', #10420, #107977, #88316 ) ;
#16855 = CONICAL_SURFACE ( 'NONE', #96297, 0.1000000000000000472, 0.003490658503988666988 ) ;
#16856 = CARTESIAN_POINT ( 'NONE',  ( 185.4218750003414016, 0.000000000000000000, 7.564683531250000925 ) ) ;
#16857 = DIRECTION ( 'NONE',  ( -0.000000000000000000, 1.000000000000000000, -0.000000000000000000 ) ) ;
#16858 = FACE_OUTER_BOUND ( 'NONE', #12386, .T. ) ;
#16859 = AXIS2_PLACEMENT_3D ( 'NONE', #34618, #84337, #36548 ) ;
#16860 = PLANE ( 'NONE',  #22250 ) ;
#16861 = VERTEX_POINT ( 'NONE', #108635 ) ;
#16862 = CONICAL_SURFACE ( 'NONE', #31486, 0.1000000000000002554, 0.003490658503988666988 ) ;
#16863 = EDGE_LOOP ( 'NONE', ( #4234, #85534 ) ) ;
#16864 = ORIENTED_EDGE ( 'NONE', *, *, #17592, .F. ) ;
#16865 = ORIENTED_EDGE ( 'NONE', *, *, #49749, .F. ) ;
#16866 = DIRECTION ( 'NONE',  ( -0.000000000000000000, -1.000000000000000000, -0.000000000000000000 ) ) ;
#16867 = FACE_BOUND ( 'NONE', #76428, .T. ) ;
#16868 = PLANE ( 'NONE',  #87019 ) ;
#16869 = CARTESIAN_POINT ( 'NONE',  ( 6.449999999999930012, 2.500000000000000000, -1.918653347947326004 ) ) ;
#16870 = ORIENTED_EDGE ( 'NONE', *, *, #650, .F. ) ;
#16871 = LINE ( 'NONE', #46362, #46726 ) ;
#16872 = DIRECTION ( 'NONE',  ( 1.000000000000000000, 0.000000000000000000, 0.000000000000000000 ) ) ;
#16873 = ORIENTED_EDGE ( 'NONE', *, *, #26783, .T. ) ;
#16874 = DIRECTION ( 'NONE',  ( 0.000000000000000000, 0.000000000000000000, 1.000000000000000000 ) ) ;
#16875 = CARTESIAN_POINT ( 'NONE',  ( 17.79089025268845603, 2.511997385349134859, -2.795007471442833236 ) ) ;
#16877 = EDGE_CURVE ( 'NONE', #112226, #90933, #89957, .T. ) ;
#16876 = AXIS2_PLACEMENT_3D ( 'NONE', #20361, #129049, #10522 ) ;
#16878 = ORIENTED_EDGE ( 'NONE', *, *, #94997, .T. ) ;
#16879 = EDGE_CURVE ( 'NONE', #117157, #113704, #8472, .T. ) ;
#16880 = FACE_OUTER_BOUND ( 'NONE', #112802, .T. ) ;
#16881 = AXIS2_PLACEMENT_3D ( 'NONE', #113559, #63825, #123376 ) ;
#16882 = CARTESIAN_POINT ( 'NONE',  ( -9.350000000000008527, 12.50000000000000000, -6.148780366869520897 ) ) ;
#16883 = EDGE_CURVE ( 'NONE', #87020, #10181, #119213, .T. ) ;
#16884 = EDGE_CURVE ( 'NONE', #118072, #40034, #69346, .T. ) ;
#16885 = EDGE_LOOP ( 'NONE', ( #47450, #37963, #16308, #28231 ) ) ;
#16886 = CARTESIAN_POINT ( 'NONE',  ( -5.600000000000023626, 2.500000000000000000, -3.983716857408426293 ) ) ;
#16887 = AXIS2_PLACEMENT_3D ( 'NONE', #19769, #109434, #120542 ) ;
#16888 = FACE_OUTER_BOUND ( 'NONE', #32024, .T. ) ;
#16889 = VERTEX_POINT ( 'NONE', #120405 ) ;
#16891 = EDGE_CURVE ( 'NONE', #42074, #123090, #58586, .T. ) ;
#16890 = CARTESIAN_POINT ( 'NONE',  ( 11.89999999999990798, 12.50000000000000000, 4.676537180435972552 ) ) ;
#16892 = ORIENTED_EDGE ( 'NONE', *, *, #92572, .F. ) ;
#16893 = VECTOR ( 'NONE', #7609, 1000.000000000000000 ) ;
#16894 = VERTEX_POINT ( 'NONE', #129599 ) ;
#16895 = LINE ( 'NONE', #26118, #20120 ) ;
#16896 = EDGE_LOOP ( 'NONE', ( #53111, #21230, #37831, #50850 ) ) ;
#16897 = DIRECTION ( 'NONE',  ( -0.000000000000000000, -1.000000000000000000, -0.000000000000000000 ) ) ;
#16898 = DIRECTION ( 'NONE',  ( 0.000000000000000000, 0.000000000000000000, 1.000000000000000000 ) ) ;
#16899 = EDGE_CURVE ( 'NONE', #14536, #85204, #41864, .T. ) ;
#16900 = EDGE_CURVE ( 'NONE', #49639, #106042, #100118, .T. ) ;
#16901 = ORIENTED_EDGE ( 'NONE', *, *, #112977, .T. ) ;
#16902 = DIRECTION ( 'NONE',  ( 0.000000000000000000, -0.000000000000000000, 1.000000000000000000 ) ) ;
#16903 = ORIENTED_EDGE ( 'NONE', *, *, #106865, .F. ) ;
#16904 = LINE ( 'NONE', #86310, #50396 ) ;
#16905 = DIRECTION ( 'NONE',  ( 0.000000000000000000, 0.000000000000000000, 1.000000000000000000 ) ) ;
#16906 = LINE ( 'NONE', #56213, #13128 ) ;
#16907 = DIRECTION ( 'NONE',  ( -0.000000000000000000, -1.000000000000000000, -0.000000000000000000 ) ) ;
#16908 = CARTESIAN_POINT ( 'NONE',  ( -9.600000000000008527, 2.500000000000000000, 4.430127018922196847 ) ) ;
#16909 = ORIENTED_EDGE ( 'NONE', *, *, #8366, .T. ) ;
#16910 = ORIENTED_EDGE ( 'NONE', *, *, #79140, .T. ) ;
#16911 = CIRCLE ( 'NONE', #102623, 0.1000000000000000472 ) ;
#16912 = DIRECTION ( 'NONE',  ( 0.000000000000000000, 0.000000000000000000, 1.000000000000000000 ) ) ;
#16913 = CARTESIAN_POINT ( 'NONE',  ( 21.24754738303277080, -0.7337760880902354232, 4.182111650399362723 ) ) ;
#16914 = CARTESIAN_POINT ( 'NONE',  ( -9.800000000000006040, 2.500000000000000000, 4.776537180435972196 ) ) ;
#16916 = ORIENTED_EDGE ( 'NONE', *, *, #116798, .T. ) ;
#16915 = EDGE_LOOP ( 'NONE', ( #123598, #44146, #108798, #20319 ) ) ;
#16917 = ORIENTED_EDGE ( 'NONE', *, *, #50360, .F. ) ;
#16918 = CARTESIAN_POINT ( 'NONE',  ( -1.850000000000033396, 2.500000000000000000, -2.411473670974877859 ) ) ;
#16919 = VECTOR ( 'NONE', #41181, 1000.000000000000000 ) ;
#16920 = CARTESIAN_POINT ( 'NONE',  ( 15.83209681635555377, 1.499999999999999556, 5.404881881984147540 ) ) ;
#16921 = CONICAL_SURFACE ( 'NONE', #10676, 0.09999999999999982514, 0.003490658503988666988 ) ;
#16922 = DIRECTION ( 'NONE',  ( 0.000000000000000000, -0.000000000000000000, 1.000000000000000000 ) ) ;
#16923 = SHAPE_DEFINITION_REPRESENTATION ( #73316, #5058 ) ;
#16924 = DIRECTION ( 'NONE',  ( -4.274815082592931898E-19, -0.9999939076577903929, -0.003490651415223739937 ) ) ;
#16925 = CARTESIAN_POINT ( 'NONE',  ( 187.2500000000000000, 9.429780353434619030E-16, -7.700000000000000178 ) ) ;
#16926 = DIRECTION ( 'NONE',  ( -0.000000000000000000, -1.000000000000000000, -0.000000000000000000 ) ) ;
#16927 = CARTESIAN_POINT ( 'NONE',  ( 115.5000000000000000, 0.000000000000000000, 0.000000000000000000 ) ) ;
#16928 = DIRECTION ( 'NONE',  ( -4.274815082592931898E-19, -0.9999939076577903929, -0.003490651415223739937 ) ) ;
#16930 = CIRCLE ( 'NONE', #98431, 0.06509327318403745899 ) ;
#16929 = CARTESIAN_POINT ( 'NONE',  ( -6.450000000000019718, 12.50000000000000000, -1.883746621131363597 ) ) ;
#16931 = CIRCLE ( 'NONE', #90108, 0.09999999999999982514 ) ;
#16932 = VERTEX_POINT ( 'NONE', #51031 ) ;
#16933 = LINE ( 'NONE', #118393, #96753 ) ;
#16934 = ORIENTED_EDGE ( 'NONE', *, *, #11310, .T. ) ;
#16935 = VERTEX_POINT ( 'NONE', #113807 ) ;
#16936 = DIRECTION ( 'NONE',  ( 0.000000000000000000, 0.000000000000000000, -1.000000000000000000 ) ) ;
#16937 = CARTESIAN_POINT ( 'NONE',  ( -6.700000000000016165, 2.500000000000000000, 4.430127018922196847 ) ) ;
#16938 = CARTESIAN_POINT ( 'NONE',  ( -3.350000000000031619, 12.50000000000000000, -7.188010851410854052 ) ) ;
#16939 = VECTOR ( 'NONE', #59397, 1000.000000000000000 ) ;
#16940 = DIRECTION ( 'NONE',  ( 0.000000000000000000, -0.9999939076577903929, 0.003490651415223739937 ) ) ;
#16941 = AXIS2_PLACEMENT_3D ( 'NONE', #66464, #99164, #38311 ) ;
#16942 = EDGE_CURVE ( 'NONE', #56443, #126922, #14724, .T. ) ;
#16943 = CARTESIAN_POINT ( 'NONE',  ( 4.149999999999941735, 12.50000000000000000, -7.188010851410854052 ) ) ;
#16944 = FACE_OUTER_BOUND ( 'NONE', #112119, .T. ) ;
#16945 = DIRECTION ( 'NONE',  ( -0.000000000000000000, -1.000000000000000000, -0.000000000000000000 ) ) ;
#16946 = ORIENTED_EDGE ( 'NONE', *, *, #41474, .T. ) ;
#16947 = DIRECTION ( 'NONE',  ( 0.000000000000000000, 1.000000000000000000, 0.000000000000000000 ) ) ;
#16948 = AXIS2_PLACEMENT_3D ( 'NONE', #24624, #126691, #65817 ) ;
#16949 = CARTESIAN_POINT ( 'NONE',  ( 0.7999999999999553024, 2.500000000000000000, -4.430127018922202176 ) ) ;
#16950 = ORIENTED_EDGE ( 'NONE', *, *, #36108, .T. ) ;
#16951 = ORIENTED_EDGE ( 'NONE', *, *, #67563, .T. ) ;
#16952 = CIRCLE ( 'NONE', #21098, 0.1000000000000002554 ) ;
#16953 = CIRCLE ( 'NONE', #85930, 0.1000000000000002554 ) ;
#16954 = VERTEX_POINT ( 'NONE', #52303 ) ;
#16955 = ORIENTED_EDGE ( 'NONE', *, *, #85529, .F. ) ;
#16956 = ORIENTED_EDGE ( 'NONE', *, *, #14401, .T. ) ;
#16957 = DIRECTION ( 'NONE',  ( 0.000000000000000000, 1.000000000000000000, 0.000000000000000000 ) ) ;
#16958 = DIRECTION ( 'NONE',  ( 0.000000000000000000, 0.000000000000000000, 1.000000000000000000 ) ) ;
#16959 = ORIENTED_EDGE ( 'NONE', *, *, #152, .T. ) ;
#16960 = DIRECTION ( 'NONE',  ( 0.000000000000000000, 1.000000000000000000, 0.000000000000000000 ) ) ;
#16961 = DIRECTION ( 'NONE',  ( -4.274815082592931898E-19, -0.9999939076577903929, -0.003490651415223739937 ) ) ;
#16962 = DIRECTION ( 'NONE',  ( 0.000000000000000000, 1.000000000000000000, 0.000000000000000000 ) ) ;
#16963 = ORIENTED_EDGE ( 'NONE', *, *, #9554, .F. ) ;
#16964 = CARTESIAN_POINT ( 'NONE',  ( 3.549999999999944755, 2.500000000000000000, -2.511473670974877948 ) ) ;
#16965 = CARTESIAN_POINT ( 'NONE',  ( -14.19999999999998685, 12.50000000000000000, -0.06509327318403752838 ) ) ;
#16966 = EDGE_LOOP ( 'NONE', ( #102248, #67737, #34286, #98490 ) ) ;
#16967 = ORIENTED_EDGE ( 'NONE', *, *, #44217, .F. ) ;
#16968 = EDGE_LOOP ( 'NONE', ( #98083, #106977, #79927, #96668 ) ) ;
#16969 = AXIS2_PLACEMENT_3D ( 'NONE', #115145, #95547, #56876 ) ;
#16970 = CARTESIAN_POINT ( 'NONE',  ( -0.6500000000000389910, 2.500000000000000000, -6.248780366869526759 ) ) ;
#16971 = AXIS2_PLACEMENT_3D ( 'NONE', #59682, #17109, #29549 ) ;
#16972 = CIRCLE ( 'NONE', #83907, 0.06509327318403745899 ) ;
#16973 = LINE ( 'NONE', #67368, #119206 ) ;
#16974 = EDGE_CURVE ( 'NONE', #84331, #69984, #81643, .T. ) ;
#16975 = AXIS2_PLACEMENT_3D ( 'NONE', #45208, #85115, #106687 ) ;
#16976 = AXIS2_PLACEMENT_3D ( 'NONE', #24039, #95995, #63956 ) ;
#16978 = VERTEX_POINT ( 'NONE', #53602 ) ;
#16977 = CIRCLE ( 'NONE', #23277, 0.06509327318403745899 ) ;
#16979 = DIRECTION ( 'NONE',  ( 0.000000000000000000, 0.000000000000000000, 1.000000000000000000 ) ) ;
#16980 = DIRECTION ( 'NONE',  ( 0.000000000000000000, 1.000000000000000000, 0.000000000000000000 ) ) ;
#16981 = EDGE_CURVE ( 'NONE', #126577, #118519, #33328, .T. ) ;
#16982 = CARTESIAN_POINT ( 'NONE',  ( 154.1524742528378056, 2.500000000000000000, -1.703575533167231537 ) ) ;
#16983 = FACE_OUTER_BOUND ( 'NONE', #53384, .T. ) ;
#16984 = EDGE_CURVE ( 'NONE', #77757, #29713, #41852, .T. ) ;
#16985 = ORIENTED_EDGE ( 'NONE', *, *, #1235, .F. ) ;
#16986 = LINE ( 'NONE', #77243, #98025 ) ;
#16987 = ORIENTED_EDGE ( 'NONE', *, *, #10091, .T. ) ;
#16988 = EDGE_CURVE ( 'NONE', #55865, #21250, #27260, .T. ) ;
#16990 = ORIENTED_EDGE ( 'NONE', *, *, #7587, .F. ) ;
#16989 = EDGE_CURVE ( 'NONE', #82532, #57756, #1267, .T. ) ;
#16991 = ORIENTED_EDGE ( 'NONE', *, *, #121472, .F. ) ;
#16992 = EDGE_CURVE ( 'NONE', #87403, #21143, #75289, .T. ) ;
#16994 = EDGE_CURVE ( 'NONE', #46254, #121408, #103985, .T. ) ;
#16993 = DIRECTION ( 'NONE',  ( 0.000000000000000000, 0.000000000000000000, 1.000000000000000000 ) ) ;
#16995 = EDGE_CURVE ( 'NONE', #117447, #36746, #85748, .T. ) ;
#16996 = FACE_BOUND ( 'NONE', #61400, .T. ) ;
#16997 = CARTESIAN_POINT ( 'NONE',  ( -10.20000000000000284, 12.50000000000000000, 4.048810130592458201 ) ) ;
#16998 = DIRECTION ( 'NONE',  ( -0.000000000000000000, 1.000000000000000000, -0.000000000000000000 ) ) ;
#16999 = DIRECTION ( 'NONE',  ( 0.000000000000000000, 0.000000000000000000, -1.000000000000000000 ) ) ;
#17000 = ORIENTED_EDGE ( 'NONE', *, *, #25401, .F. ) ;
#17001 = DIRECTION ( 'NONE',  ( -0.000000000000000000, 1.000000000000000000, -0.000000000000000000 ) ) ;
#17002 = DIRECTION ( 'NONE',  ( 0.000000000000000000, 0.000000000000000000, -1.000000000000000000 ) ) ;
#17003 = EDGE_CURVE ( 'NONE', #108664, #5075, #81127, .T. ) ;
#17004 = CARTESIAN_POINT ( 'NONE',  ( -7.100000000000013856, 12.50000000000000000, 3.637306695894644726 ) ) ;
#17005 = CARTESIAN_POINT ( 'NONE',  ( -6.450000000000017941, 12.50000000000000000, -2.446380397790840266 ) ) ;
#17006 = ORIENTED_EDGE ( 'NONE', *, *, #59383, .F. ) ;
#17007 = AXIS2_PLACEMENT_3D ( 'NONE', #84938, #14876, #4414 ) ;
#17008 = CARTESIAN_POINT ( 'NONE',  ( -14.14999999999998614, 2.500000000000000000, -2.957883832488651610 ) ) ;
#17009 = CARTESIAN_POINT ( 'NONE',  ( -8.550000000000011369, 2.500000000000000000, -2.511473670974877948 ) ) ;
#17010 = ORIENTED_EDGE ( 'NONE', *, *, #85978, .T. ) ;
#17011 = DIRECTION ( 'NONE',  ( 0.000000000000000000, -0.9999939076577903929, 0.003490651415223739937 ) ) ;
#17012 = DIRECTION ( 'NONE',  ( 0.000000000000000000, 0.000000000000000000, -1.000000000000000000 ) ) ;
#17013 = FACE_BOUND ( 'NONE', #58329, .T. ) ;
#17014 = CIRCLE ( 'NONE', #90202, 0.06509327318403745899 ) ;
#17015 = CARTESIAN_POINT ( 'NONE',  ( 7.173569985920785541, -2.500000000000000000, -8.713264184442472526 ) ) ;
#17016 = AXIS2_PLACEMENT_3D ( 'NONE', #74615, #107292, #104702 ) ;
#17017 = ORIENTED_EDGE ( 'NONE', *, *, #10364, .T. ) ;
#17019 = DIRECTION ( 'NONE',  ( 0.000000000000000000, -0.000000000000000000, 1.000000000000000000 ) ) ;
#17018 = AXIS2_PLACEMENT_3D ( 'NONE', #2333, #20073, #90738 ) ;
#17020 = ORIENTED_EDGE ( 'NONE', *, *, #33062, .F. ) ;
#17021 = VERTEX_POINT ( 'NONE', #92211 ) ;
#17022 = CARTESIAN_POINT ( 'NONE',  ( 16.86635082839110211, 0.4716143926291168631, -5.778906370536269321 ) ) ;
#17023 = CARTESIAN_POINT ( 'NONE',  ( 187.3333333333333144, 6.668395609140177704, -3.849999999999998312 ) ) ;
#17024 = ORIENTED_EDGE ( 'NONE', *, *, #25746, .F. ) ;
#17026 = CARTESIAN_POINT ( 'NONE',  ( 14.14999999999989200, 2.500000000000000000, -2.265063509461101798 ) ) ;
#17025 = AXIS2_PLACEMENT_3D ( 'NONE', #123435, #124084, #25889 ) ;
#17027 = DIRECTION ( 'NONE',  ( 0.000000000000000000, -0.000000000000000000, 1.000000000000000000 ) ) ;
#17028 = CONICAL_SURFACE ( 'NONE', #98617, 0.1000000000000000472, 0.003490658503988666988 ) ;
#17029 = CIRCLE ( 'NONE', #90220, 0.09999999999999999167 ) ;
#17030 = CARTESIAN_POINT ( 'NONE',  ( 13.34999999999989662, 12.50000000000000000, -1.472243186433550122 ) ) ;
#17031 = EDGE_CURVE ( 'NONE', #43734, #8654, #94167, .T. ) ;
#17032 = CARTESIAN_POINT ( 'NONE',  ( 185.7812500006828031, 0.000000000000000000, 7.700000000000000178 ) ) ;
#17033 = CONICAL_SURFACE ( 'NONE', #90222, 0.1000000000000002554, 0.003490658503988666988 ) ;
#17034 = EDGE_CURVE ( 'NONE', #109486, #16978, #62791, .T. ) ;
#17035 = EDGE_LOOP ( 'NONE', ( #5001, #65090, #120774, #126329 ) ) ;
#17036 = ADVANCED_FACE ( 'NONE', ( #73233 ), #23076, .T. ) ;
#17037 = CARTESIAN_POINT ( 'NONE',  ( 7.899999999999921307, 2.500000000000000000, -0.1000000000000023925 ) ) ;
#17038 = CIRCLE ( 'NONE', #10705, 0.1000000000000002554 ) ;
#17039 = CIRCLE ( 'NONE', #60994, 0.1000000000000000056 ) ;
#17040 = DIRECTION ( 'NONE',  ( 0.000000000000000000, -0.9999939076577903929, 0.003490651415223739937 ) ) ;
#17041 = LINE ( 'NONE', #85811, #109813 ) ;
#17042 = CARTESIAN_POINT ( 'NONE',  ( -12.69999999999999396, 12.50000000000000000, 0.4115034346978150848 ) ) ;
#17043 = ORIENTED_EDGE ( 'NONE', *, *, #67229, .T. ) ;
#17044 = PLANE ( 'NONE',  #9856 ) ;
#17045 = ORIENTED_EDGE ( 'NONE', *, *, #21019, .F. ) ;
#17046 = EDGE_CURVE ( 'NONE', #76513, #79082, #79511, .T. ) ;
#17047 = FACE_OUTER_BOUND ( 'NONE', #82379, .T. ) ;
#17048 = DIRECTION ( 'NONE',  ( -0.000000000000000000, -1.000000000000000000, -0.000000000000000000 ) ) ;
#17050 = VERTEX_POINT ( 'NONE', #71956 ) ;
#17049 = ADVANCED_FACE ( 'NONE', ( #23481 ), #151, .T. ) ;
#17051 = CARTESIAN_POINT ( 'NONE',  ( -0.4000000000000396572, 12.50000000000000000, 4.330127018922196314 ) ) ;
#17052 = DIRECTION ( 'NONE',  ( 0.000000000000000000, 1.000000000000000000, 0.000000000000000000 ) ) ;
#17053 = EDGE_CURVE ( 'NONE', #72282, #18843, #54457, .T. ) ;
#17054 = DIRECTION ( 'NONE',  ( 0.000000000000000000, 0.000000000000000000, 1.000000000000000000 ) ) ;
#17055 = ADVANCED_FACE ( 'NONE', ( #64055 ), #113038, .T. ) ;
#17056 = DIRECTION ( 'NONE',  ( -0.000000000000000000, -1.000000000000000000, -0.000000000000000000 ) ) ;
#17057 = EDGE_LOOP ( 'NONE', ( #59874, #38521, #112051, #101176 ) ) ;
#17058 = FACE_OUTER_BOUND ( 'NONE', #60433, .T. ) ;
#17059 = PLANE ( 'NONE',  #123319 ) ;
#17060 = CARTESIAN_POINT ( 'NONE',  ( 184.6927083336747160, 6.551208109652275624, -3.782341765624998686 ) ) ;
#17061 = DIRECTION ( 'NONE',  ( 0.000000000000000000, 0.000000000000000000, 1.000000000000000000 ) ) ;
#17063 = ADVANCED_FACE ( 'NONE', ( #122345 ), #81728, .T. ) ;
#17062 = DIRECTION ( 'NONE',  ( -0.000000000000000000, 1.000000000000000000, -0.000000000000000000 ) ) ;
#17064 = EDGE_LOOP ( 'NONE', ( #3253, #50345 ) ) ;
#17065 = ORIENTED_EDGE ( 'NONE', *, *, #74394, .T. ) ;
#17066 = DIRECTION ( 'NONE',  ( 0.000000000000000000, -0.000000000000000000, 1.000000000000000000 ) ) ;
#17067 = ORIENTED_EDGE ( 'NONE', *, *, #89792, .F. ) ;
#17068 = CONICAL_SURFACE ( 'NONE', #35891, 0.1000000000000002554, 0.003490658503988666988 ) ;
#17069 = DIRECTION ( 'NONE',  ( -0.000000000000000000, -1.000000000000000000, -0.000000000000000000 ) ) ;
#17070 = CONICAL_SURFACE ( 'NONE', #73527, 0.1000000000000002554, 0.003490658503988666988 ) ;
#17071 = CIRCLE ( 'NONE', #117424, 0.06509327318403745899 ) ;
#17073 = EDGE_LOOP ( 'NONE', ( #83131, #65394, #5574, #74536 ) ) ;
#17072 = VERTEX_POINT ( 'NONE', #62778 ) ;
#17074 = ORIENTED_EDGE ( 'NONE', *, *, #102200, .T. ) ;
#17075 = DIRECTION ( 'NONE',  ( -0.000000000000000000, -1.000000000000000000, -0.000000000000000000 ) ) ;
#17076 = CARTESIAN_POINT ( 'NONE',  ( 10.39999999999991154, 12.50000000000000000, -3.637306695894650055 ) ) ;
#17077 = CIRCLE ( 'NONE', #77650, 0.06509327318403745899 ) ;
#17078 = FACE_OUTER_BOUND ( 'NONE', #106351, .T. ) ;
#17079 = CONICAL_SURFACE ( 'NONE', #27561, 0.09999999999999982514, 0.003490658503988666988 ) ;
#17080 = DIRECTION ( 'NONE',  ( 0.000000000000000000, 1.000000000000000000, 0.000000000000000000 ) ) ;
#17081 = DIRECTION ( 'NONE',  ( 0.000000000000000000, 0.000000000000000000, 1.000000000000000000 ) ) ;
#17082 = AXIS2_PLACEMENT_3D ( 'NONE', #128697, #47529, #117515 ) ;
#17083 = CARTESIAN_POINT ( 'NONE',  ( -9.400000000000007461, 12.50000000000000000, -0.3464101615137783474 ) ) ;
#17084 = AXIS2_PLACEMENT_3D ( 'NONE', #27629, #96373, #85910 ) ;
#17085 = EDGE_CURVE ( 'NONE', #72494, #89288, #108821, .T. ) ;
#17086 = ORIENTED_EDGE ( 'NONE', *, *, #86200, .F. ) ;
#17087 = DIRECTION ( 'NONE',  ( 0.000000000000000000, 1.000000000000000000, 0.000000000000000000 ) ) ;
#17089 = ORIENTED_EDGE ( 'NONE', *, *, #115648, .T. ) ;
#17088 = AXIS2_PLACEMENT_3D ( 'NONE', #35751, #56016, #84842 ) ;
#17090 = ORIENTED_EDGE ( 'NONE', *, *, #83650, .T. ) ;
#17091 = EDGE_LOOP ( 'NONE', ( #106900, #11827, #85613, #84293 ) ) ;
#17092 = ORIENTED_EDGE ( 'NONE', *, *, #45553, .T. ) ;
#17093 = DIRECTION ( 'NONE',  ( 0.000000000000000000, 0.000000000000000000, 1.000000000000000000 ) ) ;
#17094 = VERTEX_POINT ( 'NONE', #96088 ) ;
#17095 = VERTEX_POINT ( 'NONE', #54239 ) ;
#17096 = DIRECTION ( 'NONE',  ( 0.000000000000000000, 1.000000000000000000, 0.000000000000000000 ) ) ;
#17097 = CARTESIAN_POINT ( 'NONE',  ( 129.5000000000000000, -0.6250000000000028866, -7.634788798650553154 ) ) ;
#17098 = EDGE_CURVE ( 'NONE', #31405, #71950, #94155, .T. ) ;
#17099 = DIRECTION ( 'NONE',  ( 0.000000000000000000, -0.000000000000000000, 1.000000000000000000 ) ) ;
#17100 = DIRECTION ( 'NONE',  ( 0.000000000000000000, 0.000000000000000000, 1.000000000000000000 ) ) ;
#17101 = CARTESIAN_POINT ( 'NONE',  ( -7.900000000000011013, 12.50000000000000000, 3.637306695894644726 ) ) ;
#17102 = ORIENTED_EDGE ( 'NONE', *, *, #31428, .F. ) ;
#17103 = DIRECTION ( 'NONE',  ( 0.000000000000000000, 0.000000000000000000, 1.000000000000000000 ) ) ;
#17104 = AXIS2_PLACEMENT_3D ( 'NONE', #20076, #101852, #404 ) ;
#17105 = CIRCLE ( 'NONE', #46372, 0.09999999999999982514 ) ;
#17106 = ORIENTED_EDGE ( 'NONE', *, *, #83456, .T. ) ;
#17107 = CARTESIAN_POINT ( 'NONE',  ( 2.049999999999950084, 2.500000000000000000, -2.265063509461101798 ) ) ;
#17108 = ORIENTED_EDGE ( 'NONE', *, *, #101030, .F. ) ;
#17109 = DIRECTION ( 'NONE',  ( -0.000000000000000000, 1.000000000000000000, -0.000000000000000000 ) ) ;
#17110 = VERTEX_POINT ( 'NONE', #115721 ) ;
#17111 = ADVANCED_FACE ( 'NONE', ( #126195 ), #98356, .T. ) ;
#17112 = EDGE_LOOP ( 'NONE', ( #97392, #63245 ) ) ;
#17113 = CARTESIAN_POINT ( 'NONE',  ( 7.299999999999926104, 2.500000000000000000, -4.083716857408426826 ) ) ;
#17114 = DIRECTION ( 'NONE',  ( 0.000000000000000000, 0.000000000000000000, 1.000000000000000000 ) ) ;
#17115 = AXIS2_PLACEMENT_3D ( 'NONE', #95724, #125182, #65608 ) ;
#17116 = CARTESIAN_POINT ( 'NONE',  ( 186.2083333333333428, -4.445597072760145707, -7.699999999999951328 ) ) ;
#17117 = AXIS2_PLACEMENT_3D ( 'NONE', #93963, #102495, #122151 ) ;
#17118 = DIRECTION ( 'NONE',  ( 0.000000000000000000, -0.9999939076577903929, 0.003490651415223739937 ) ) ;
#17119 = DIRECTION ( 'NONE',  ( 0.000000000000000000, 0.000000000000000000, -1.000000000000000000 ) ) ;
#17120 = ORIENTED_EDGE ( 'NONE', *, *, #113606, .T. ) ;
#17121 = CARTESIAN_POINT ( 'NONE',  ( -4.350000000000027178, 2.500000000000000000, -6.048780366869526581 ) ) ;
#17122 = CARTESIAN_POINT ( 'NONE',  ( -5.850000000000018296, 12.50000000000000000, 2.857883832488649301 ) ) ;
#17123 = DIRECTION ( 'NONE',  ( 0.000000000000000000, 1.000000000000000000, 0.000000000000000000 ) ) ;
#17124 = DIRECTION ( 'NONE',  ( 0.000000000000000000, 0.000000000000000000, 1.000000000000000000 ) ) ;
#17125 = AXIS2_PLACEMENT_3D ( 'NONE', #43937, #74031, #73373 ) ;
#17126 = AXIS2_PLACEMENT_3D ( 'NONE', #50531, #31554, #111377 ) ;
#17127 = DIRECTION ( 'NONE',  ( 0.000000000000000000, 0.000000000000000000, 1.000000000000000000 ) ) ;
#17128 = EDGE_LOOP ( 'NONE', ( #46452, #128656 ) ) ;
#17129 = AXIS2_PLACEMENT_3D ( 'NONE', #118637, #8664, #99661 ) ;
#17130 = CONICAL_SURFACE ( 'NONE', #42226, 0.09999999999999982514, 0.003490658503988666988 ) ;
#17131 = EDGE_LOOP ( 'NONE', ( #94606, #76102, #78500, #6059 ) ) ;
#17132 = CARTESIAN_POINT ( 'NONE',  ( -2.300000000000033573, 12.50000000000000000, 0.4115034346978109769 ) ) ;
#17133 = AXIS2_PLACEMENT_3D ( 'NONE', #84015, #96901, #17012 ) ;
#17134 = ORIENTED_EDGE ( 'NONE', *, *, #105152, .F. ) ;
#17135 = DIRECTION ( 'NONE',  ( 0.000000000000000000, 0.000000000000000000, 1.000000000000000000 ) ) ;
#17136 = DIRECTION ( 'NONE',  ( 0.000000000000000000, 0.000000000000000000, -1.000000000000000000 ) ) ;
#17137 = EDGE_CURVE ( 'NONE', #30008, #118142, #21093, .T. ) ;
#17138 = AXIS2_PLACEMENT_3D ( 'NONE', #7891, #30139, #56983 ) ;
#17139 = EDGE_LOOP ( 'NONE', ( #24329, #112993 ) ) ;
#17140 = CARTESIAN_POINT ( 'NONE',  ( 184.2500000000000000, 9.429780353434619030E-16, -7.700000000000000178 ) ) ;
#17141 = DIRECTION ( 'NONE',  ( -0.000000000000000000, 1.000000000000000000, -0.000000000000000000 ) ) ;
#17142 = DIRECTION ( 'NONE',  ( 0.000000000000000000, 0.000000000000000000, -1.000000000000000000 ) ) ;
#17143 = DIRECTION ( 'NONE',  ( 0.000000000000000000, 1.000000000000000000, 0.000000000000000000 ) ) ;
#17144 = VERTEX_POINT ( 'NONE', #75793 ) ;
#17145 = EDGE_CURVE ( 'NONE', #66592, #19145, #73322, .T. ) ;
#17146 = CARTESIAN_POINT ( 'NONE',  ( -7.500000000000001776, -1.500000000000000000, 10.00000000000000178 ) ) ;
#17147 = DIRECTION ( 'NONE',  ( -0.000000000000000000, -1.000000000000000000, -0.000000000000000000 ) ) ;
#17148 = ORIENTED_EDGE ( 'NONE', *, *, #129442, .T. ) ;
#17149 = EDGE_CURVE ( 'NONE', #72904, #65479, #47004, .T. ) ;
#17150 = EDGE_CURVE ( 'NONE', #118811, #91731, #69120, .T. ) ;
#17151 = EDGE_CURVE ( 'NONE', #125468, #93533, #126847, .T. ) ;
#17153 = ADVANCED_FACE ( 'NONE', ( #124910 ), #104612, .T. ) ;
#17152 = PLANE ( 'NONE',  #67341 ) ;
#17154 = CARTESIAN_POINT ( 'NONE',  ( 4.349999999999937472, 2.500000000000000000, 6.841600689897072485 ) ) ;
#17155 = DIRECTION ( 'NONE',  ( -4.274815082592931898E-19, -0.9999939076577903929, -0.003490651415223739937 ) ) ;
#17156 = ORIENTED_EDGE ( 'NONE', *, *, #47209, .T. ) ;
#17157 = DIRECTION ( 'NONE',  ( 0.000000000000000000, 0.000000000000000000, 1.000000000000000000 ) ) ;
#17158 = AXIS2_PLACEMENT_3D ( 'NONE', #21398, #90123, #451 ) ;
#17159 = AXIS2_PLACEMENT_3D ( 'NONE', #48592, #41366, #9303 ) ;
#17160 = CIRCLE ( 'NONE', #29722, 0.1000000000000002554 ) ;
#17161 = EDGE_LOOP ( 'NONE', ( #107186, #36476, #78326, #49216 ) ) ;
#17162 = DIRECTION ( 'NONE',  ( -0.000000000000000000, 1.000000000000000000, -0.000000000000000000 ) ) ;
#17163 = CARTESIAN_POINT ( 'NONE',  ( -11.05000000000000071, 2.500000000000000000, -2.511473670974873951 ) ) ;
#17164 = EDGE_CURVE ( 'NONE', #45421, #112782, #124270, .T. ) ;
#17165 = PLANE ( 'NONE',  #22507 ) ;
#17166 = ORIENTED_EDGE ( 'NONE', *, *, #19671, .T. ) ;
#17167 = EDGE_CURVE ( 'NONE', #102949, #109829, #55531, .T. ) ;
#17170 = EDGE_CURVE ( 'NONE', #39659, #12221, #115064, .T. ) ;
#17169 = FACE_OUTER_BOUND ( 'NONE', #116253, .T. ) ;
#17168 = AXIS2_PLACEMENT_3D ( 'NONE', #68543, #79033, #91901 ) ;
#17171 = VECTOR ( 'NONE', #13765, 1000.000000000000000 ) ;
#17172 = CIRCLE ( 'NONE', #40203, 0.1000000000000002554 ) ;
#17173 = DIRECTION ( 'NONE',  ( 0.000000000000000000, -0.000000000000000000, 1.000000000000000000 ) ) ;
#17174 = CIRCLE ( 'NONE', #36002, 0.06509327318403745899 ) ;
#17175 = ORIENTED_EDGE ( 'NONE', *, *, #14501, .F. ) ;
#17176 = AXIS2_PLACEMENT_3D ( 'NONE', #127562, #48354, #98095 ) ;
#17177 = CARTESIAN_POINT ( 'NONE',  ( 10.84999999999991260, 12.50000000000000000, -2.165063509461101710 ) ) ;
#17178 = ORIENTED_EDGE ( 'NONE', *, *, #36383, .T. ) ;
#17179 = CIRCLE ( 'NONE', #42270, 0.1000000000000002554 ) ;
#17180 = CARTESIAN_POINT ( 'NONE',  ( -13.14999999999999147, 2.500000000000000000, 1.718653347947325383 ) ) ;
#17181 = ORIENTED_EDGE ( 'NONE', *, *, #45984, .F. ) ;
#17182 = CARTESIAN_POINT ( 'NONE',  ( -11.05000000000000071, 12.50000000000000000, -6.841600689897075149 ) ) ;
#17183 = CARTESIAN_POINT ( 'NONE',  ( 14.59999999999989484, 2.500000000000000000, -0.7928203230275542301 ) ) ;
#17184 = EDGE_LOOP ( 'NONE', ( #59926, #94832, #69664, #92386 ) ) ;
#17185 = EDGE_LOOP ( 'NONE', ( #75782, #46271 ) ) ;
#17186 = CARTESIAN_POINT ( 'NONE',  ( -1.250000000000036193, 12.50000000000000000, 5.802370205355744659 ) ) ;
#17187 = DIRECTION ( 'NONE',  ( -4.274815082592931898E-19, -0.9999939076577903929, -0.003490651415223739937 ) ) ;
#17188 = ORIENTED_EDGE ( 'NONE', *, *, #107016, .F. ) ;
#17189 = CARTESIAN_POINT ( 'NONE',  ( -1.900000000000034106, 2.500000000000000000, 0.3464101615137735735 ) ) ;
#17190 = CARTESIAN_POINT ( 'NONE',  ( -7.300000000000018474, 2.500000000000000000, -3.883716857408426648 ) ) ;
#17191 = DIRECTION ( 'NONE',  ( 0.000000000000000000, 1.000000000000000000, 0.000000000000000000 ) ) ;
#17192 = CARTESIAN_POINT ( 'NONE',  ( -11.84999999999999609, 2.500000000000000000, 2.611473670974873151 ) ) ;
#17193 = DIRECTION ( 'NONE',  ( 0.000000000000000000, 0.000000000000000000, 1.000000000000000000 ) ) ;
#17194 = CARTESIAN_POINT ( 'NONE',  ( 2.099999999999950351, 2.500000000000000000, -5.022947341949754119 ) ) ;
#17195 = VECTOR ( 'NONE', #85428, 1000.000000000000000 ) ;
#17196 = AXIS2_PLACEMENT_3D ( 'NONE', #128069, #67172, #97952 ) ;
#17197 = EDGE_LOOP ( 'NONE', ( #62385, #8576 ) ) ;
#17198 = ORIENTED_EDGE ( 'NONE', *, *, #76465, .F. ) ;
#17199 = ORIENTED_EDGE ( 'NONE', *, *, #28497, .F. ) ;
#17200 = EDGE_LOOP ( 'NONE', ( #42786, #115505 ) ) ;
#17201 = FACE_OUTER_BOUND ( 'NONE', #100504, .T. ) ;
#17202 = FACE_OUTER_BOUND ( 'NONE', #119976, .T. ) ;
#17203 = DIRECTION ( 'NONE',  ( 0.000000000000000000, -0.000000000000000000, 1.000000000000000000 ) ) ;
#17204 = EDGE_LOOP ( 'NONE', ( #29989, #109325 ) ) ;
#17205 = FACE_BOUND ( 'NONE', #54979, .T. ) ;
#17206 = ADVANCED_FACE ( 'NONE', ( #95452 ), #2213, .T. ) ;
#17207 = AXIS2_PLACEMENT_3D ( 'NONE', #3043, #111027, #21379 ) ;
#17208 = CARTESIAN_POINT ( 'NONE',  ( 10.19999999999991580, 12.50000000000000000, -0.2813168883297409439 ) ) ;
#17209 = CARTESIAN_POINT ( 'NONE',  ( 14.54999999999989591, 2.500000000000000000, 2.265063509461097357 ) ) ;
#17210 =( GEOMETRIC_REPRESENTATION_CONTEXT ( 3 ) GLOBAL_UNCERTAINTY_ASSIGNED_CONTEXT ( ( #14045 ) ) GLOBAL_UNIT_ASSIGNED_CONTEXT ( ( #22472, #129212, #51921 ) ) REPRESENTATION_CONTEXT ( 'NONE', 'WORKASPACE' ) );
#17211 = EDGE_CURVE ( 'NONE', #37472, #35157, #18936, .T. ) ;
#17213 = CARTESIAN_POINT ( 'NONE',  ( -2.100000000000033840, 12.50000000000000000, 3.702399969078682407 ) ) ;
#17212 = CIRCLE ( 'NONE', #48648, 0.06509327318403745899 ) ;
#17214 = AXIS2_PLACEMENT_3D ( 'NONE', #32973, #12013, #72876 ) ;
#17215 = DIRECTION ( 'NONE',  ( 0.000000000000000000, 0.000000000000000000, 1.000000000000000000 ) ) ;
#17216 = ADVANCED_FACE ( 'NONE', ( #125542 ), #90043, .T. ) ;
#17217 = CARTESIAN_POINT ( 'NONE',  ( 0.3999999999999555023, 12.50000000000000000, 4.330127018922196314 ) ) ;
#17218 = DIRECTION ( 'NONE',  ( 0.000000000000000000, 1.000000000000000000, 0.000000000000000000 ) ) ;
#17219 = CARTESIAN_POINT ( 'NONE',  ( -13.29999999999998828, 12.50000000000000000, 4.265033745738159077 ) ) ;
#17220 = CARTESIAN_POINT ( 'NONE',  ( 2.699999999999944666, 12.50000000000000000, 4.676537180435972552 ) ) ;
#17221 = CARTESIAN_POINT ( 'NONE',  ( -2.300000000000033573, 12.50000000000000000, -3.983716857408426293 ) ) ;
#17222 = CIRCLE ( 'NONE', #50702, 0.06509327318403745899 ) ;
#17224 = ADVANCED_FACE ( 'NONE', ( #77100 ), #35688, .T. ) ;
#17223 = CARTESIAN_POINT ( 'NONE',  ( 12.49999999999990408, 12.50000000000000000, -3.572213422710612374 ) ) ;
#17225 = AXIS2_PLACEMENT_3D ( 'NONE', #9180, #90965, #18984 ) ;
#17226 = VERTEX_POINT ( 'NONE', #76456 ) ;
#17227 = ORIENTED_EDGE ( 'NONE', *, *, #96378, .F. ) ;
#17228 = ORIENTED_EDGE ( 'NONE', *, *, #71233, .F. ) ;
#17230 = VERTEX_POINT ( 'NONE', #26710 ) ;
#17229 = VECTOR ( 'NONE', #10368, 1000.000000000000000 ) ;
#17231 = AXIS2_PLACEMENT_3D ( 'NONE', #80573, #31469, #83778 ) ;
#17232 = CIRCLE ( 'NONE', #115530, 0.09999999999999982514 ) ;
#17233 = CARTESIAN_POINT ( 'NONE',  ( 17.50000000000000355, -2.413244906436780024, -3.595454705092401504 ) ) ;
#17234 = DIRECTION ( 'NONE',  ( 0.000000000000000000, 1.000000000000000000, 0.000000000000000000 ) ) ;
#17236 = ORIENTED_EDGE ( 'NONE', *, *, #9480, .T. ) ;
#17235 = VERTEX_POINT ( 'NONE', #66620 ) ;
#17237 = ORIENTED_EDGE ( 'NONE', *, *, #1867, .F. ) ;
#17238 = AXIS2_PLACEMENT_3D ( 'NONE', #37204, #77119, #67254 ) ;
#17239 = DIRECTION ( 'NONE',  ( -0.000000000000000000, -1.000000000000000000, -0.000000000000000000 ) ) ;
#17240 = AXIS2_PLACEMENT_3D ( 'NONE', #64728, #66021, #75201 ) ;
#17241 = CARTESIAN_POINT ( 'NONE',  ( -9.800000000000004263, 2.500000000000000000, 3.983716857408420076 ) ) ;
#17242 = DIRECTION ( 'NONE',  ( -4.274815082592931898E-19, -0.9999939076577903929, -0.003490651415223739937 ) ) ;
#17243 = LINE ( 'NONE', #125924, #88963 ) ;
#17244 = PLANE ( 'NONE',  #39386 ) ;
#17245 = ADVANCED_FACE ( 'NONE', ( #16847 ), #116997, .T. ) ;
#17246 = ORIENTED_EDGE ( 'NONE', *, *, #94708, .F. ) ;
#17247 = EDGE_LOOP ( 'NONE', ( #42993, #99985, #56194, #59557 ) ) ;
#17248 = ORIENTED_EDGE ( 'NONE', *, *, #75410, .F. ) ;
#17249 = VERTEX_POINT ( 'NONE', #27995 ) ;
#17250 = CARTESIAN_POINT ( 'NONE',  ( -12.89999999999999147, 2.500000000000000000, -0.5928203230275499447 ) ) ;
#17251 = CONICAL_SURFACE ( 'NONE', #59056, 0.1000000000000002554, 0.003490658503988666988 ) ;
#17252 = VERTEX_POINT ( 'NONE', #47642 ) ;
#17253 = EDGE_LOOP ( 'NONE', ( #82987, #127167, #39361, #108474 ) ) ;
#17254 = CARTESIAN_POINT ( 'NONE',  ( -8.550000000000013145, 2.500000000000000000, -1.818653347947326138 ) ) ;
#17255 = CARTESIAN_POINT ( 'NONE',  ( 3.099999999999945466, 12.50000000000000000, 0.3464101615137735735 ) ) ;
#17256 = CARTESIAN_POINT ( 'NONE',  ( -6.450000000000017941, 2.500000000000000000, -2.511473670974877948 ) ) ;
#17257 = ADVANCED_FACE ( 'NONE', ( #67914 ), #87977, .T. ) ;
#17259 = DIRECTION ( 'NONE',  ( -0.000000000000000000, 1.000000000000000000, -0.000000000000000000 ) ) ;
#17258 = CIRCLE ( 'NONE', #46520, 0.1000000000000002554 ) ;
#17260 = AXIS2_PLACEMENT_3D ( 'NONE', #85678, #77157, #84394 ) ;
#17261 = VECTOR ( 'NONE', #5858, 1000.000000000000000 ) ;
#17262 = CARTESIAN_POINT ( 'NONE',  ( -9.600000000000006750, 2.500000000000000000, 3.637306695894644726 ) ) ;
#17263 = ORIENTED_EDGE ( 'NONE', *, *, #501, .F. ) ;
#17264 = DIRECTION ( 'NONE',  ( 0.000000000000000000, 0.000000000000000000, -1.000000000000000000 ) ) ;
#17265 = CIRCLE ( 'NONE', #31879, 0.1000000000000000056 ) ;
#17267 = VERTEX_POINT ( 'NONE', #69190 ) ;
#17266 = AXIS2_PLACEMENT_3D ( 'NONE', #105876, #126809, #75757 ) ;
#17268 = DIRECTION ( 'NONE',  ( 0.000000000000000000, 0.000000000000000000, -1.000000000000000000 ) ) ;
#17269 = VECTOR ( 'NONE', #64486, 1000.000000000000000 ) ;
#17270 = EDGE_LOOP ( 'NONE', ( #123824, #100918 ) ) ;
#17271 = DIRECTION ( 'NONE',  ( -1.000000000000000000, 0.000000000000000000, 7.228014483236698281E-17 ) ) ;
#17272 = DIRECTION ( 'NONE',  ( 0.000000000000000000, -0.9999939076577903929, 0.003490651415223739937 ) ) ;
#17273 = VERTEX_POINT ( 'NONE', #98016 ) ;
#17274 = CIRCLE ( 'NONE', #90440, 0.09999999999999982514 ) ;
#17275 = CARTESIAN_POINT ( 'NONE',  ( -9.800000000000006040, 12.50000000000000000, 4.611443907251934426 ) ) ;
#17276 = AXIS2_PLACEMENT_3D ( 'NONE', #2440, #42395, #122248 ) ;
#17277 = EDGE_CURVE ( 'NONE', #83264, #118052, #62876, .T. ) ;
#17278 = DIRECTION ( 'NONE',  ( -0.4999999999999471534, -0.000000000000000000, -0.8660254037844692387 ) ) ;
#17279 = ORIENTED_EDGE ( 'NONE', *, *, #122695, .F. ) ;
#17280 = CIRCLE ( 'NONE', #71689, 0.06509327318403741736 ) ;
#17281 = DIRECTION ( 'NONE',  ( 0.000000000000000000, 0.000000000000000000, 1.000000000000000000 ) ) ;
#17282 = EDGE_LOOP ( 'NONE', ( #85462, #127230, #105432, #77362 ) ) ;
#17284 = EDGE_LOOP ( 'NONE', ( #115854, #563 ) ) ;
#17283 = ADVANCED_FACE ( 'NONE', ( #48283 ), #8985, .T. ) ;
#17285 = CARTESIAN_POINT ( 'NONE',  ( 4.549999999999939426, 12.50000000000000000, -2.165063509461101710 ) ) ;
#17286 = DIRECTION ( 'NONE',  ( 0.000000000000000000, 0.000000000000000000, -1.000000000000000000 ) ) ;
#17287 = CARTESIAN_POINT ( 'NONE',  ( 187.0052083336747444, -6.551208109652278289, 3.782341765624995134 ) ) ;
#17288 = CARTESIAN_POINT ( 'NONE',  ( 13.34999999999989662, 2.500000000000000000, -2.165063509461101710 ) ) ;
#17289 = DIRECTION ( 'NONE',  ( 0.8660254037844390407, 0.000000000000000000, -0.4999999999999991673 ) ) ;
#17290 = CARTESIAN_POINT ( 'NONE',  ( -1.250000000000035749, 2.500000000000000000, -2.757883832488654097 ) ) ;
#17291 = AXIS2_PLACEMENT_3D ( 'NONE', #53887, #3498, #93816 ) ;
#17292 = VERTEX_POINT ( 'NONE', #90115 ) ;
#17293 = CONICAL_SURFACE ( 'NONE', #46872, 0.1000000000000002554, 0.003490658503988666988 ) ;
#17294 = CARTESIAN_POINT ( 'NONE',  ( -3.150000000000030109, 2.500000000000000000, 1.818653347947321475 ) ) ;
#17295 = FACE_OUTER_BOUND ( 'NONE', #124701, .T. ) ;
#17296 = PRESENTATION_LAYER_ASSIGNMENT (  '', '', ( #10944 ) ) ;
#17297 = EDGE_CURVE ( 'NONE', #83209, #67824, #4346, .T. ) ;
#17298 = EDGE_LOOP ( 'NONE', ( #26971, #12330, #99023, #18050 ) ) ;
#17299 = DIRECTION ( 'NONE',  ( 0.000000000000000000, -0.000000000000000000, 1.000000000000000000 ) ) ;
#17300 = LINE ( 'NONE', #108918, #78219 ) ;
#17301 = FACE_OUTER_BOUND ( 'NONE', #53614, .T. ) ;
#17302 = CARTESIAN_POINT ( 'NONE',  ( 0.7999999999999548583, 12.50000000000000000, 4.330127018922196314 ) ) ;
#17303 = CIRCLE ( 'NONE', #59217, 0.1000000000000002554 ) ;
#17305 = AXIS2_PLACEMENT_3D ( 'NONE', #73468, #113401, #63673 ) ;
#17304 = CARTESIAN_POINT ( 'NONE',  ( 3.549999999999943867, 12.50000000000000000, -1.753560074763288679 ) ) ;
#17306 = ORIENTED_EDGE ( 'NONE', *, *, #117101, .F. ) ;
#17308 = EDGE_CURVE ( 'NONE', #64742, #129259, #80328, .T. ) ;
#17307 = CIRCLE ( 'NONE', #46578, 5.000000000000004441 ) ;
#17309 = AXIS2_PLACEMENT_3D ( 'NONE', #36186, #106206, #57093 ) ;
#17310 = DIRECTION ( 'NONE',  ( 0.000000000000000000, 0.000000000000000000, 1.000000000000000000 ) ) ;
#17311 =( NAMED_UNIT ( * ) SI_UNIT ( $, .STERADIAN. ) SOLID_ANGLE_UNIT ( ) );
#17312 = ADVANCED_FACE ( 'NONE', ( #444 ), #67044, .T. ) ;
#17313 = EDGE_CURVE ( 'NONE', #38667, #108868, #29428, .T. ) ;
#17314 = EDGE_CURVE ( 'NONE', #104775, #51072, #40413, .T. ) ;
#17315 = ADVANCED_FACE ( 'NONE', ( #88173 ), #104710, .T. ) ;
#17316 = AXIS2_PLACEMENT_3D ( 'NONE', #124273, #56155, #27331 ) ;
#17317 = EDGE_LOOP ( 'NONE', ( #10455, #113612, #86877, #9161 ) ) ;
#17319 = CIRCLE ( 'NONE', #50506, 0.06509327318403745899 ) ;
#17318 = DIRECTION ( 'NONE',  ( -0.000000000000000000, -1.000000000000000000, -0.000000000000000000 ) ) ;
#17320 = ORIENTED_EDGE ( 'NONE', *, *, #32738, .F. ) ;
#17321 = CIRCLE ( 'NONE', #123948, 0.1000000000000000056 ) ;
#17323 = VERTEX_POINT ( 'NONE', #109782 ) ;
#17322 = VECTOR ( 'NONE', #73007, 1000.000000000000000 ) ;
#17324 = CARTESIAN_POINT ( 'NONE',  ( -2.100000000000033396, 2.500000000000000000, -4.922947341949753586 ) ) ;
#17325 = ADVANCED_FACE ( 'NONE', ( #39139 ), #37827, .T. ) ;
#17326 = ADVANCED_FACE ( 'NONE', ( #20111 ), #48295, .T. ) ;
#17328 = ORIENTED_EDGE ( 'NONE', *, *, #18385, .F. ) ;
#17327 = AXIS2_PLACEMENT_3D ( 'NONE', #62001, #101915, #12229 ) ;
#17329 = DIRECTION ( 'NONE',  ( 0.000000000000000000, -0.9999939076577903929, 0.003490651415223739937 ) ) ;
#17330 = CARTESIAN_POINT ( 'NONE',  ( -13.94999999999998685, 2.500000000000000000, 1.718653347947325383 ) ) ;
#17331 = DIRECTION ( 'NONE',  ( 0.000000000000000000, 0.000000000000000000, -1.000000000000000000 ) ) ;
#17332 = ORIENTED_EDGE ( 'NONE', *, *, #16176, .T. ) ;
#17333 = ADVANCED_FACE ( 'NONE', ( #79670 ), #7696, .T. ) ;
#17335 = ADVANCED_FACE ( 'NONE', ( #79047 ), #117297, .T. ) ;
#17334 = FACE_BOUND ( 'NONE', #79686, .T. ) ;
#17336 = AXIS2_PLACEMENT_3D ( 'NONE', #17554, #66652, #79084 ) ;
#17338 = ORIENTED_EDGE ( 'NONE', *, *, #95880, .F. ) ;
#17337 = CARTESIAN_POINT ( 'NONE',  ( 3.349999999999944578, 2.500000000000000000, -5.802370205355749988 ) ) ;
#17339 = FACE_OUTER_BOUND ( 'NONE', #77583, .T. ) ;
#17340 = EDGE_CURVE ( 'NONE', #94540, #46019, #67131, .T. ) ;
#17341 = CARTESIAN_POINT ( 'NONE',  ( -15.59999999999998010, 2.500000000000000000, 0.4464101615137759382 ) ) ;
#17342 = ADVANCED_FACE ( 'NONE', ( #49587 ), #12765, .T. ) ;
#17343 = ORIENTED_EDGE ( 'NONE', *, *, #23538, .T. ) ;
#17344 = ORIENTED_EDGE ( 'NONE', *, *, #99561, .T. ) ;
#17345 = ORIENTED_EDGE ( 'NONE', *, *, #62717, .F. ) ;
#17346 = LINE ( 'NONE', #116847, #46309 ) ;
#17347 = CARTESIAN_POINT ( 'NONE',  ( 3.349999999999941913, 2.500000000000000000, 5.802370205355744659 ) ) ;
#17349 = CARTESIAN_POINT ( 'NONE',  ( 13.09999999999990195, 2.500000000000000000, 4.576537180435972019 ) ) ;
#17348 = CIRCLE ( 'NONE', #123975, 0.09999999999999982514 ) ;
#17350 = CIRCLE ( 'NONE', #94632, 0.09999999999999982514 ) ;
#17351 = FACE_BOUND ( 'NONE', #93381, .T. ) ;
#17352 = VERTEX_POINT ( 'NONE', #20752 ) ;
#17353 = PLANE ( 'NONE',  #117973 ) ;
#17354 = FACE_OUTER_BOUND ( 'NONE', #75541, .T. ) ;
#17355 = ORIENTED_EDGE ( 'NONE', *, *, #57587, .F. ) ;
#17357 = FACE_OUTER_BOUND ( 'NONE', #32864, .T. ) ;
#17356 = AXIS2_PLACEMENT_3D ( 'NONE', #27170, #7521, #68378 ) ;
#17358 = AXIS2_PLACEMENT_3D ( 'NONE', #88363, #127663, #124611 ) ;
#17359 = AXIS2_PLACEMENT_3D ( 'NONE', #8399, #129509, #49003 ) ;
#17361 = AXIS2_PLACEMENT_3D ( 'NONE', #31175, #52724, #63194 ) ;
#17360 = DIRECTION ( 'NONE',  ( 0.000000000000000000, 0.000000000000000000, 1.000000000000000000 ) ) ;
#17362 = DIRECTION ( 'NONE',  ( -0.000000000000000000, -1.000000000000000000, -0.000000000000000000 ) ) ;
#17363 = CARTESIAN_POINT ( 'NONE',  ( -9.400000000000007461, 12.50000000000000000, 0.3464101615137735735 ) ) ;
#17364 = DIRECTION ( 'NONE',  ( 0.000000000000000000, 0.000000000000000000, 1.000000000000000000 ) ) ;
#17365 = AXIS2_PLACEMENT_3D ( 'NONE', #58405, #98297, #8616 ) ;
#17366 = AXIS2_PLACEMENT_3D ( 'NONE', #44371, #104581, #35221 ) ;
#17367 = AXIS2_PLACEMENT_3D ( 'NONE', #32970, #12010, #32332 ) ;
#17368 = ORIENTED_EDGE ( 'NONE', *, *, #45686, .F. ) ;
#17369 = ORIENTED_EDGE ( 'NONE', *, *, #118129, .F. ) ;
#17370 = ORIENTED_EDGE ( 'NONE', *, *, #53680, .T. ) ;
#17371 = ORIENTED_EDGE ( 'NONE', *, *, #125056, .F. ) ;
#17373 = ORIENTED_EDGE ( 'NONE', *, *, #102734, .T. ) ;
#17372 = AXIS2_PLACEMENT_3D ( 'NONE', #7760, #512, #40477 ) ;
#17374 = LINE ( 'NONE', #19315, #58898 ) ;
#17375 = CARTESIAN_POINT ( 'NONE',  ( -4.600000000000028066, 12.50000000000000000, -3.637306695894650055 ) ) ;
#17376 = ORIENTED_EDGE ( 'NONE', *, *, #99772, .T. ) ;
#17377 = FACE_BOUND ( 'NONE', #6657, .T. ) ;
#17378 = DIRECTION ( 'NONE',  ( 0.000000000000000000, 0.000000000000000000, -1.000000000000000000 ) ) ;
#17379 = ADVANCED_FACE ( 'NONE', ( #60693 ), #2301, .T. ) ;
#17380 = FACE_OUTER_BOUND ( 'NONE', #16140, .T. ) ;
#17381 = ADVANCED_FACE ( 'NONE', ( #71133 ), #80968, .T. ) ;
#17382 = CARTESIAN_POINT ( 'NONE',  ( -1.250000000000001110, 2.500000000000000000, -2.165063509461101710 ) ) ;
#17383 = CARTESIAN_POINT ( 'NONE',  ( -1.850000000000033396, 12.50000000000000000, -1.818653347947325916 ) ) ;
#17384 = FACE_OUTER_BOUND ( 'NONE', #80984, .T. ) ;
#17385 = VERTEX_POINT ( 'NONE', #122185 ) ;
#17386 = CARTESIAN_POINT ( 'NONE',  ( 18.00406198521865164, -1.510509990005264314, 4.944015973543655740 ) ) ;
#17387 = CIRCLE ( 'NONE', #13183, 0.06509327318403745899 ) ;
#17388 = ADVANCED_FACE ( 'NONE', ( #83550 ), #115160, .T. ) ;
#17389 = VERTEX_POINT ( 'NONE', #22704 ) ;
#17390 = ORIENTED_EDGE ( 'NONE', *, *, #70778, .F. ) ;
#17391 = ORIENTED_EDGE ( 'NONE', *, *, #62884, .F. ) ;
#17392 = DIRECTION ( 'NONE',  ( 0.000000000000000000, 0.000000000000000000, 1.000000000000000000 ) ) ;
#17393 = LINE ( 'NONE', #118836, #123704 ) ;
#17394 = CARTESIAN_POINT ( 'NONE',  ( -7.500000000000001776, -1.500000000000000000, 9.000000000000001776 ) ) ;
#17395 = ORIENTED_EDGE ( 'NONE', *, *, #32195, .F. ) ;
#17396 = CARTESIAN_POINT ( 'NONE',  ( 4.912722231850285226, 2.500000000000252687, -9.942384338124218957 ) ) ;
#17397 = AXIS2_PLACEMENT_3D ( 'NONE', #97993, #27308, #56132 ) ;
#17398 = VECTOR ( 'NONE', #82107, 1000.000000000000000 ) ;
#17400 = CARTESIAN_POINT ( 'NONE',  ( 3.149999999999942624, 2.500000000000000000, 6.148780366869520897 ) ) ;
#17399 = CONICAL_SURFACE ( 'NONE', #52933, 0.1000000000000002554, 0.003490658503988666988 ) ;
#17401 = CARTESIAN_POINT ( 'NONE',  ( -12.29999999999999361, 12.50000000000000000, 3.983716857408420076 ) ) ;
#17402 = CARTESIAN_POINT ( 'NONE',  ( 187.2343750003414016, 8.734944146203032389, 5.348610694689227483E-16 ) ) ;
#17403 = DIRECTION ( 'NONE',  ( 0.000000000000000000, 0.000000000000000000, -1.000000000000000000 ) ) ;
#17404 = FACE_OUTER_BOUND ( 'NONE', #7710, .T. ) ;
#17405 = DIRECTION ( 'NONE',  ( 0.000000000000000000, -0.9999939076577903929, 0.003490651415223739937 ) ) ;
#17406 = VECTOR ( 'NONE', #128965, 1000.000000000000000 ) ;
#17407 = ORIENTED_EDGE ( 'NONE', *, *, #10221, .T. ) ;
#17408 = DIRECTION ( 'NONE',  ( -0.000000000000000000, -1.000000000000000000, -0.000000000000000000 ) ) ;
#17409 = CIRCLE ( 'NONE', #98902, 0.06509327318403745899 ) ;
#17410 = CIRCLE ( 'NONE', #63406, 0.06509327318403745899 ) ;
#17411 = ORIENTED_EDGE ( 'NONE', *, *, #56473, .F. ) ;
#17412 = VECTOR ( 'NONE', #51804, 1000.000000000000000 ) ;
#17413 = ORIENTED_EDGE ( 'NONE', *, *, #84151, .T. ) ;
#17414 = CARTESIAN_POINT ( 'NONE',  ( -3.950000000000024603, 12.50000000000000000, -2.511473670974877948 ) ) ;
#17415 = FACE_OUTER_BOUND ( 'NONE', #101762, .T. ) ;
#17416 = DIRECTION ( 'NONE',  ( 0.000000000000000000, 0.000000000000000000, 1.000000000000000000 ) ) ;
#17417 = AXIS2_PLACEMENT_3D ( 'NONE', #67440, #87743, #59618 ) ;
#17418 = ORIENTED_EDGE ( 'NONE', *, *, #53674, .T. ) ;
#17419 = VERTEX_POINT ( 'NONE', #61973 ) ;
#17420 = EDGE_CURVE ( 'NONE', #3252, #30644, #90126, .T. ) ;
#17421 = CARTESIAN_POINT ( 'NONE',  ( 10.44999999999991402, 2.500000000000000000, -2.165063509461101710 ) ) ;
#17423 = AXIS2_PLACEMENT_3D ( 'NONE', #29158, #108334, #69055 ) ;
#17422 = CARTESIAN_POINT ( 'NONE',  ( -12.04999999999999716, 2.500000000000000000, -6.395190528383298378 ) ) ;
#17424 = VECTOR ( 'NONE', #104523, 1000.000000000000000 ) ;
#17425 = CARTESIAN_POINT ( 'NONE',  ( -13.54999999999998828, 12.50000000000000000, -2.511473670974875727 ) ) ;
#17426 = ORIENTED_EDGE ( 'NONE', *, *, #108506, .T. ) ;
#17427 = VERTEX_POINT ( 'NONE', #102528 ) ;
#17428 = CARTESIAN_POINT ( 'NONE',  ( 1.249999999999986899, 2.500000000000000000, 6.495190528383297135 ) ) ;
#17429 = CIRCLE ( 'NONE', #27916, 0.09999999999999982514 ) ;
#17430 = VERTEX_POINT ( 'NONE', #63251 ) ;
#17431 = DIRECTION ( 'NONE',  ( -0.000000000000000000, -1.000000000000000000, -0.000000000000000000 ) ) ;
#17432 = DIRECTION ( 'NONE',  ( 0.000000000000000000, 1.000000000000000000, 0.000000000000000000 ) ) ;
#17433 = ORIENTED_EDGE ( 'NONE', *, *, #5934, .F. ) ;
#17434 = CARTESIAN_POINT ( 'NONE',  ( 14.34999999999989662, 2.500000000000000000, 1.818653347947321475 ) ) ;
#17435 = DIRECTION ( 'NONE',  ( 0.000000000000000000, 1.000000000000000000, 0.000000000000000000 ) ) ;
#17436 = CARTESIAN_POINT ( 'NONE',  ( -2.700000000000031264, 2.500000000000000000, 4.576537180435972019 ) ) ;
#17437 = B_SPLINE_CURVE_WITH_KNOTS ( 'NONE', 3,
 ( #128445, #129095, #21039, #100257, #100879, #59708, #70153, #11211, #29569, #99615, #104, #49879, #9933, #41350, #88481, #60959 ),
 .UNSPECIFIED., .F., .F.,
 ( 4, 2, 2, 2, 2, 2, 2, 4 ),
 ( 0.0007527720032625739898, 0.001260609959358783812, 0.001768447915454993743, 0.002022366893503097299, 0.002276285871551201288, 0.002784123827647406665, 0.003799799739839814817, 0.004815475652032223837 ),
 .UNSPECIFIED. ) ;
#17438 = EDGE_CURVE ( 'NONE', #116494, #39604, #77616, .T. ) ;
#17439 = ADVANCED_FACE ( 'NONE', ( #100588 ), #101894, .T. ) ;
#17440 = CARTESIAN_POINT ( 'NONE',  ( -0.6500000000000403233, 2.500000000000000000, 6.148780366869520009 ) ) ;
#17441 = EDGE_LOOP ( 'NONE', ( #58935, #110328, #67057, #4975 ) ) ;
#17442 = CARTESIAN_POINT ( 'NONE',  ( -0.6500000000000398792, 2.500000000000000000, -2.611473670974877592 ) ) ;
#17443 = FACE_OUTER_BOUND ( 'NONE', #96854, .T. ) ;
#17444 = VERTEX_POINT ( 'NONE', #43633 ) ;
#17445 = VERTEX_POINT ( 'NONE', #3055 ) ;
#17446 = AXIS2_PLACEMENT_3D ( 'NONE', #47730, #85702, #116446 ) ;
#17447 = AXIS2_PLACEMENT_3D ( 'NONE', #109238, #30720, #119078 ) ;
#17448 = EDGE_CURVE ( 'NONE', #36869, #113352, #29519, .T. ) ;
#17449 = DIRECTION ( 'NONE',  ( -0.000000000000000000, 1.000000000000000000, -0.000000000000000000 ) ) ;
#17450 = DIRECTION ( 'NONE',  ( 0.000000000000000000, 0.000000000000000000, 1.000000000000000000 ) ) ;
#17451 = CARTESIAN_POINT ( 'NONE',  ( 1.249999999999988898, 2.500000000000000000, -6.395190528383301931 ) ) ;
#17452 = DIRECTION ( 'NONE',  ( 0.000000000000000000, 0.000000000000000000, 1.000000000000000000 ) ) ;
#17453 = CARTESIAN_POINT ( 'NONE',  ( -3.350000000000031619, 12.50000000000000000, -5.737276932171712751 ) ) ;
#17454 = DIRECTION ( 'NONE',  ( 0.000000000000000000, 0.000000000000000000, 1.000000000000000000 ) ) ;
#17455 = CONICAL_SURFACE ( 'NONE', #4842, 0.1000000000000000472, 0.003490658503988666988 ) ;
#17456 = AXIS2_PLACEMENT_3D ( 'NONE', #24084, #14865, #92831 ) ;
#17457 = DIRECTION ( 'NONE',  ( 0.000000000000000000, -0.9999939076577903929, 0.003490651415223739937 ) ) ;
#17458 = VECTOR ( 'NONE', #54264, 1000.000000000000000 ) ;
#17459 = CARTESIAN_POINT ( 'NONE',  ( 13.14999999999989733, 12.50000000000000000, -1.883746621131363375 ) ) ;
#17461 = CONICAL_SURFACE ( 'NONE', #94839, 0.09999999999999982514, 0.003490658503988666988 ) ;
#17460 = DIRECTION ( 'NONE',  ( 0.000000000000000000, 0.000000000000000000, 1.000000000000000000 ) ) ;
#17462 = AXIS2_PLACEMENT_3D ( 'NONE', #125806, #33591, #76085 ) ;
#17463 = DIRECTION ( 'NONE',  ( -0.000000000000000000, -1.000000000000000000, -0.000000000000000000 ) ) ;
#17464 = VECTOR ( 'NONE', #73450, 1000.000000000000000 ) ;
#17465 = CIRCLE ( 'NONE', #113630, 0.06509327318403745899 ) ;
#17466 = ORIENTED_EDGE ( 'NONE', *, *, #79554, .F. ) ;
#17467 = CARTESIAN_POINT ( 'NONE',  ( 8.349999999999923261, 2.500000000000000000, 2.857883832488649301 ) ) ;
#17468 = CIRCLE ( 'NONE', #92816, 0.06509327318403745899 ) ;
#17469 = DIRECTION ( 'NONE',  ( 0.000000000000000000, 1.000000000000000000, 0.000000000000000000 ) ) ;
#17470 = DIRECTION ( 'NONE',  ( 0.000000000000000000, 0.000000000000000000, 1.000000000000000000 ) ) ;
#17471 = DIRECTION ( 'NONE',  ( 0.000000000000000000, 0.000000000000000000, -1.000000000000000000 ) ) ;
#17472 = ORIENTED_EDGE ( 'NONE', *, *, #123464, .T. ) ;
#17473 = DIRECTION ( 'NONE',  ( 0.000000000000000000, -0.000000000000000000, 1.000000000000000000 ) ) ;
#17474 = EDGE_CURVE ( 'NONE', #65281, #19309, #98535, .T. ) ;
#17475 = CARTESIAN_POINT ( 'NONE',  ( 185.2916666666666572, 4.445597072760072876, -7.700000000000080114 ) ) ;
#17477 = ORIENTED_EDGE ( 'NONE', *, *, #161, .F. ) ;
#17476 = CARTESIAN_POINT ( 'NONE',  ( 13.54999999999989768, 2.500000000000000000, -2.511473670974877948 ) ) ;
#17478 = EDGE_CURVE ( 'NONE', #114104, #25583, #52483, .T. ) ;
#17479 = EDGE_CURVE ( 'NONE', #85979, #38146, #50862, .T. ) ;
#17480 = CIRCLE ( 'NONE', #109443, 0.06509327318403745899 ) ;
#17481 = ORIENTED_EDGE ( 'NONE', *, *, #9103, .F. ) ;
#17482 = EDGE_LOOP ( 'NONE', ( #110612, #51771 ) ) ;
#17483 = VERTEX_POINT ( 'NONE', #31866 ) ;
#17484 = ORIENTED_EDGE ( 'NONE', *, *, #47074, .T. ) ;
#17485 = DIRECTION ( 'NONE',  ( -4.274815082592931898E-19, -0.9999939076577903929, -0.003490651415223739937 ) ) ;
#17486 = EDGE_CURVE ( 'NONE', #112609, #24484, #121526, .T. ) ;
#17487 = ADVANCED_FACE ( 'NONE', ( #52149 ), #1105, .T. ) ;
#17488 = ADVANCED_FACE ( 'NONE', ( #82904 ), #37919, .T. ) ;
#17490 = FACE_OUTER_BOUND ( 'NONE', #2674, .T. ) ;
#17489 = AXIS2_PLACEMENT_3D ( 'NONE', #129429, #70474, #120861 ) ;
#17491 = PLANE ( 'NONE',  #31656 ) ;
#17492 = CIRCLE ( 'NONE', #111603, 0.06509327318403745899 ) ;
#17493 = CARTESIAN_POINT ( 'NONE',  ( -12.09999999999999609, 2.500000000000000000, -4.330127018922198978 ) ) ;
#17494 = CIRCLE ( 'NONE', #30049, 0.1000000000000002554 ) ;
#17495 = ORIENTED_EDGE ( 'NONE', *, *, #91527, .T. ) ;
#17496 = EDGE_CURVE ( 'NONE', #13248, #9486, #91425, .T. ) ;
#17497 = CARTESIAN_POINT ( 'NONE',  ( 9.549999999999918998, 2.500000000000000000, 2.265063509461097357 ) ) ;
#17498 = ORIENTED_EDGE ( 'NONE', *, *, #37404, .F. ) ;
#17499 = CARTESIAN_POINT ( 'NONE',  ( 81.97643238337541050, -3.858501996648050714, -6.173828409589621202 ) ) ;
#17500 = CARTESIAN_POINT ( 'NONE',  ( 12.64862127267602254, -2.500000000000000000, -8.430718249867293679 ) ) ;
#17501 = DIRECTION ( 'NONE',  ( -0.000000000000000000, -1.000000000000000000, -0.000000000000000000 ) ) ;
#17502 = DIRECTION ( 'NONE',  ( 0.000000000000000000, 0.000000000000000000, 1.000000000000000000 ) ) ;
#17503 = DIRECTION ( 'NONE',  ( 0.000000000000000000, 0.000000000000000000, -1.000000000000000000 ) ) ;
#17504 = CIRCLE ( 'NONE', #90678, 0.1000000000000002554 ) ;
#17505 = AXIS2_PLACEMENT_3D ( 'NONE', #88106, #79609, #28577 ) ;
#17506 = ADVANCED_FACE ( 'NONE', ( #23313 ), #71793, .T. ) ;
#17507 = CONICAL_SURFACE ( 'NONE', #119930, 0.1000000000000002554, 0.003490658503988666988 ) ;
#17508 = ORIENTED_EDGE ( 'NONE', *, *, #38366, .F. ) ;
#17509 = AXIS2_PLACEMENT_3D ( 'NONE', #3027, #25215, #24591 ) ;
#17510 = ORIENTED_EDGE ( 'NONE', *, *, #52986, .F. ) ;
#17511 = VERTEX_POINT ( 'NONE', #46848 ) ;
#17512 = VERTEX_POINT ( 'NONE', #75012 ) ;
#17513 = DIRECTION ( 'NONE',  ( -4.274815082592931898E-19, -0.9999939076577903929, -0.003490651415223739937 ) ) ;
#17514 = DIRECTION ( 'NONE',  ( -0.000000000000000000, 1.000000000000000000, -0.000000000000000000 ) ) ;
#17515 = CARTESIAN_POINT ( 'NONE',  ( 0.6499999999999566125, 2.500000000000000000, -6.148780366869526226 ) ) ;
#17516 = FACE_BOUND ( 'NONE', #107881, .T. ) ;
#17517 = CIRCLE ( 'NONE', #42598, 0.06509327318403745899 ) ;
#17518 = DIRECTION ( 'NONE',  ( 0.000000000000000000, 1.000000000000000000, 0.000000000000000000 ) ) ;
#17519 = CARTESIAN_POINT ( 'NONE',  ( 5.399999999999932854, 12.50000000000000000, 5.088040615133786027 ) ) ;
#17520 = DIRECTION ( 'NONE',  ( 0.000000000000000000, 0.000000000000000000, -1.000000000000000000 ) ) ;
#17521 = FACE_OUTER_BOUND ( 'NONE', #25525, .T. ) ;
#17522 = CIRCLE ( 'NONE', #15463, 0.1000000000000002554 ) ;
#17523 = VECTOR ( 'NONE', #68751, 1000.000000000000000 ) ;
#17524 = AXIS2_PLACEMENT_3D ( 'NONE', #18725, #97927, #28555 ) ;
#17525 = CARTESIAN_POINT ( 'NONE',  ( 184.0468750003414300, -8.734944146203032389, -1.604583208406767949E-15 ) ) ;
#17526 = CARTESIAN_POINT ( 'NONE',  ( 184.5000000000000000, 0.000000000000000000, -7.699999999999999289 ) ) ;
#17527 = CIRCLE ( 'NONE', #38497, 0.09999999999999982514 ) ;
#17528 = CARTESIAN_POINT ( 'NONE',  ( -4.600000000000025402, 2.500000000000000000, -2.385244779468109755E-15 ) ) ;
#17529 = AXIS2_PLACEMENT_3D ( 'NONE', #103683, #25749, #4159 ) ;
#17530 = CARTESIAN_POINT ( 'NONE',  ( 11.44999999999990692, 2.500000000000000000, -6.841600689897078702 ) ) ;
#17531 = ORIENTED_EDGE ( 'NONE', *, *, #38142, .F. ) ;
#17532 = ORIENTED_EDGE ( 'NONE', *, *, #49299, .T. ) ;
#17533 = VERTEX_POINT ( 'NONE', #113644 ) ;
#17534 = ORIENTED_EDGE ( 'NONE', *, *, #110600, .F. ) ;
#17535 = FACE_OUTER_BOUND ( 'NONE', #5797, .T. ) ;
#17536 = FACE_BOUND ( 'NONE', #73248, .T. ) ;
#17537 = DIRECTION ( 'NONE',  ( 0.000000000000000000, -0.000000000000000000, 1.000000000000000000 ) ) ;
#17538 = DIRECTION ( 'NONE',  ( -0.000000000000000000, 1.000000000000000000, -0.000000000000000000 ) ) ;
#17539 = EDGE_CURVE ( 'NONE', #94776, #61381, #73411, .T. ) ;
#17541 = ORIENTED_EDGE ( 'NONE', *, *, #22244, .T. ) ;
#17540 = AXIS2_PLACEMENT_3D ( 'NONE', #50958, #12925, #63984 ) ;
#17543 = VECTOR ( 'NONE', #123639, 1000.000000000000000 ) ;
#17542 = CARTESIAN_POINT ( 'NONE',  ( -6.650000000000014566, 2.500000000000000000, 6.595190528383296780 ) ) ;
#17544 = CARTESIAN_POINT ( 'NONE',  ( 1.649999999999951950, 2.500000000000000000, -5.802370205355749988 ) ) ;
#17545 = PLANE ( 'NONE',  #26483 ) ;
#17546 = VERTEX_POINT ( 'NONE', #94001 ) ;
#17547 = FACE_OUTER_BOUND ( 'NONE', #72631, .T. ) ;
#17548 = DIRECTION ( 'NONE',  ( 0.000000000000000000, 0.000000000000000000, 1.000000000000000000 ) ) ;
#17549 = EDGE_CURVE ( 'NONE', #63883, #21550, #33712, .T. ) ;
#17550 = AXIS2_PLACEMENT_3D ( 'NONE', #63075, #42828, #52605 ) ;
#17551 = CONICAL_SURFACE ( 'NONE', #74005, 0.09999999999999999167, 0.003490658503988666988 ) ;
#17552 = VECTOR ( 'NONE', #21969, 1000.000000000000000 ) ;
#17553 = VERTEX_POINT ( 'NONE', #44245 ) ;
#17554 = CARTESIAN_POINT ( 'NONE',  ( 8.099999999999921485, 12.50000000000000000, -0.3464101615137783474 ) ) ;
#17555 = CARTESIAN_POINT ( 'NONE',  ( 2.099999999999947686, 12.50000000000000000, 5.022947341949748790 ) ) ;
#17556 = CIRCLE ( 'NONE', #109524, 0.06509327318403745899 ) ;
#17558 = VERTEX_POINT ( 'NONE', #34454 ) ;
#17557 = CIRCLE ( 'NONE', #122045, 0.06509327318403743123 ) ;
#17559 = VECTOR ( 'NONE', #7887, 1000.000000000000000 ) ;
#17560 = DIRECTION ( 'NONE',  ( 0.000000000000000000, -0.9999939076577903929, 0.003490651415223739937 ) ) ;
#17561 = DIRECTION ( 'NONE',  ( -0.000000000000000000, 1.000000000000000000, -0.000000000000000000 ) ) ;
#17562 = DIRECTION ( 'NONE',  ( -0.000000000000000000, -1.000000000000000000, -0.000000000000000000 ) ) ;
#17564 = EDGE_LOOP ( 'NONE', ( #62073, #73258, #97491, #54644 ) ) ;
#17563 = CONICAL_SURFACE ( 'NONE', #40601, 0.09999999999999982514, 0.003490658503988666988 ) ;
#17565 = VERTEX_POINT ( 'NONE', #4300 ) ;
#17566 = CARTESIAN_POINT ( 'NONE',  ( -9.600000000000006750, 12.50000000000000000, -0.6928203230275542523 ) ) ;
#17567 = EDGE_LOOP ( 'NONE', ( #4599, #52117 ) ) ;
#17568 = CARTESIAN_POINT ( 'NONE',  ( 8.099999999999923261, 2.500000000000000000, 4.676537180435972552 ) ) ;
#17569 = FACE_BOUND ( 'NONE', #41180, .T. ) ;
#17570 = ORIENTED_EDGE ( 'NONE', *, *, #64896, .F. ) ;
#17571 = CARTESIAN_POINT ( 'NONE',  ( 4.149999999999938183, 12.50000000000000000, 5.802370205355744659 ) ) ;
#17572 = ORIENTED_EDGE ( 'NONE', *, *, #68946, .F. ) ;
#17573 = LINE ( 'NONE', #48338, #29478 ) ;
#17574 = AXIS2_PLACEMENT_3D ( 'NONE', #59816, #68300, #88599 ) ;
#17575 = DIRECTION ( 'NONE',  ( -0.000000000000000000, -1.000000000000000000, -0.000000000000000000 ) ) ;
#17576 = CARTESIAN_POINT ( 'NONE',  ( 8.749999999999923617, 2.500000000000000000, -7.288010851410854585 ) ) ;
#17577 = FACE_OUTER_BOUND ( 'NONE', #118449, .T. ) ;
#17578 = DIRECTION ( 'NONE',  ( 0.000000000000000000, 0.000000000000000000, 1.000000000000000000 ) ) ;
#17579 = AXIS2_PLACEMENT_3D ( 'NONE', #107124, #8283, #105854 ) ;
#17580 = EDGE_LOOP ( 'NONE', ( #118211, #92492 ) ) ;
#17582 = ORIENTED_EDGE ( 'NONE', *, *, #25073, .T. ) ;
#17581 = EDGE_CURVE ( 'NONE', #41455, #77736, #96391, .T. ) ;
#17583 = DIRECTION ( 'NONE',  ( 0.000000000000000000, -0.9999939076577903929, 0.003490651415223739937 ) ) ;
#17584 = DIRECTION ( 'NONE',  ( 0.000000000000000000, 0.000000000000000000, -1.000000000000000000 ) ) ;
#17585 = CARTESIAN_POINT ( 'NONE',  ( -1.250000000000001554, 12.50000000000000000, 2.099970236277060032 ) ) ;
#17587 = VERTEX_POINT ( 'NONE', #55997 ) ;
#17586 = ORIENTED_EDGE ( 'NONE', *, *, #96807, .F. ) ;
#17588 = ORIENTED_EDGE ( 'NONE', *, *, #74964, .T. ) ;
#17589 = FACE_OUTER_BOUND ( 'NONE', #55034, .T. ) ;
#17590 = AXIS2_PLACEMENT_3D ( 'NONE', #76645, #109145, #19485 ) ;
#17592 = EDGE_CURVE ( 'NONE', #27692, #66554, #58761, .T. ) ;
#17591 = FACE_OUTER_BOUND ( 'NONE', #31639, .T. ) ;
#17593 = CONICAL_SURFACE ( 'NONE', #19663, 0.1000000000000002554, 0.003490658503988666988 ) ;
#17594 = CARTESIAN_POINT ( 'NONE',  ( -4.400000000000025224, 12.50000000000000000, 0.3464101615137735735 ) ) ;
#17595 = APPLICATION_PROTOCOL_DEFINITION ( 'draft international standard', 'automotive_design', 1998, #83124 ) ;
#17596 = LINE ( 'NONE', #67318, #41139 ) ;
#17597 = DIRECTION ( 'NONE',  ( -0.000000000000000000, -1.000000000000000000, -0.000000000000000000 ) ) ;
#17598 = CARTESIAN_POINT ( 'NONE',  ( -2.900000000000029221, 12.50000000000000000, -4.265033745738164406 ) ) ;
#17599 = DIRECTION ( 'NONE',  ( -0.000000000000000000, -1.000000000000000000, -0.000000000000000000 ) ) ;
#17600 = DIRECTION ( 'NONE',  ( 0.000000000000000000, 0.000000000000000000, 1.000000000000000000 ) ) ;
#17601 = ADVANCED_FACE ( 'NONE', ( #25240 ), #65086, .T. ) ;
#17602 = EDGE_CURVE ( 'NONE', #120216, #87169, #114915, .T. ) ;
#17603 = CARTESIAN_POINT ( 'NONE',  ( 12.49999999999990052, 12.50000000000000000, 0.6928203230275494784 ) ) ;
#17604 = EDGE_LOOP ( 'NONE', ( #25085, #28564 ) ) ;
#17605 = EDGE_LOOP ( 'NONE', ( #35249, #107748 ) ) ;
#17606 = AXIS2_PLACEMENT_3D ( 'NONE', #78869, #66440, #56604 ) ;
#17607 = EDGE_CURVE ( 'NONE', #89288, #72494, #85923, .T. ) ;
#17608 = FACE_OUTER_BOUND ( 'NONE', #75984, .T. ) ;
#17609 = ORIENTED_EDGE ( 'NONE', *, *, #114046, .F. ) ;
#17610 = ORIENTED_EDGE ( 'NONE', *, *, #60221, .T. ) ;
#17611 = ADVANCED_FACE ( 'NONE', ( #103828 ), #14138, .T. ) ;
#17612 = DIRECTION ( 'NONE',  ( -4.274815082592931898E-19, -0.9999939076577903929, -0.003490651415223739937 ) ) ;
#17613 = DIRECTION ( 'NONE',  ( 0.000000000000000000, 0.000000000000000000, 1.000000000000000000 ) ) ;
#17614 = DIRECTION ( 'NONE',  ( 0.000000000000000000, 0.000000000000000000, 1.000000000000000000 ) ) ;
#17615 = FACE_OUTER_BOUND ( 'NONE', #114064, .T. ) ;
#17616 = DIRECTION ( 'NONE',  ( -4.274815082592931898E-19, -0.9999939076577903929, -0.003490651415223739937 ) ) ;
#17617 = AXIS2_PLACEMENT_3D ( 'NONE', #115892, #116533, #63584 ) ;
#17618 = LINE ( 'NONE', #35983, #126320 ) ;
#17619 = CONICAL_SURFACE ( 'NONE', #42699, 0.09999999999999982514, 0.003490658503988666988 ) ;
#17620 = DIRECTION ( 'NONE',  ( 0.000000000000000000, -0.9999939076577903929, 0.003490651415223739937 ) ) ;
#17621 = EDGE_LOOP ( 'NONE', ( #15190, #72563 ) ) ;
#17622 = DIRECTION ( 'NONE',  ( 0.000000000000000000, 0.000000000000000000, 1.000000000000000000 ) ) ;
#17623 = AXIS2_PLACEMENT_3D ( 'NONE', #44616, #65536, #123185 ) ;
#17624 = AXIS2_PLACEMENT_3D ( 'NONE', #94636, #14142, #54085 ) ;
#17625 = DIRECTION ( 'NONE',  ( 0.000000000000000000, 0.000000000000000000, 1.000000000000000000 ) ) ;
#17626 = EDGE_LOOP ( 'NONE', ( #57369, #41175 ) ) ;
#17627 = ADVANCED_FACE ( 'NONE', ( #4959 ), #42128, .T. ) ;
#17628 = ORIENTED_EDGE ( 'NONE', *, *, #15718, .F. ) ;
#17629 = VERTEX_POINT ( 'NONE', #15419 ) ;
#17630 = ORIENTED_EDGE ( 'NONE', *, *, #52449, .T. ) ;
#17631 = DIRECTION ( 'NONE',  ( 0.000000000000000000, 1.000000000000000000, 0.000000000000000000 ) ) ;
#17632 = CARTESIAN_POINT ( 'NONE',  ( 7.899999999999924860, 2.500000000000000000, -5.022947341949754119 ) ) ;
#17633 = ORIENTED_EDGE ( 'NONE', *, *, #96435, .T. ) ;
#17634 = CARTESIAN_POINT ( 'NONE',  ( -9.550000000000006040, 2.500000000000000000, 2.165063509461097713 ) ) ;
#17635 = EDGE_CURVE ( 'NONE', #5027, #27825, #79680, .T. ) ;
#17636 = CARTESIAN_POINT ( 'NONE',  ( -9.350000000000006750, 12.50000000000000000, 1.883746621131358934 ) ) ;
#17637 = AXIS2_PLACEMENT_3D ( 'NONE', #70753, #61597, #1999 ) ;
#17638 = AXIS2_PLACEMENT_3D ( 'NONE', #106499, #67181, #96033 ) ;
#17639 = CARTESIAN_POINT ( 'NONE',  ( -2.300000000000032685, 2.500000000000000000, -4.676537180435978769 ) ) ;
#17640 = ORIENTED_EDGE ( 'NONE', *, *, #120342, .T. ) ;
#17641 = CONICAL_SURFACE ( 'NONE', #19717, 0.09999999999999982514, 0.003490658503988666988 ) ;
#17642 = DIRECTION ( 'NONE',  ( 0.000000000000000000, 0.000000000000000000, -1.000000000000000000 ) ) ;
#17643 = EDGE_CURVE ( 'NONE', #89461, #74255, #75631, .T. ) ;
#17644 = DIRECTION ( 'NONE',  ( 0.000000000000000000, -0.000000000000000000, 1.000000000000000000 ) ) ;
#17645 = EDGE_LOOP ( 'NONE', ( #97776, #81373 ) ) ;
#17646 = AXIS2_PLACEMENT_3D ( 'NONE', #126359, #117804, #56948 ) ;
#17647 = CIRCLE ( 'NONE', #51127, 0.09999999999999982514 ) ;
#17648 = ORIENTED_EDGE ( 'NONE', *, *, #39741, .T. ) ;
#17649 = ORIENTED_EDGE ( 'NONE', *, *, #7406, .F. ) ;
#17650 = PLANE ( 'NONE',  #124188 ) ;
#17651 = EDGE_CURVE ( 'NONE', #38892, #97893, #42035, .T. ) ;
#17652 = EDGE_CURVE ( 'NONE', #41301, #82923, #35101, .T. ) ;
#17653 = EDGE_CURVE ( 'NONE', #58662, #38209, #46232, .T. ) ;
#17654 = DIRECTION ( 'NONE',  ( 0.000000000000000000, 0.000000000000000000, 1.000000000000000000 ) ) ;
#17655 = CIRCLE ( 'NONE', #82442, 0.06509327318403745899 ) ;
#17656 = AXIS2_PLACEMENT_3D ( 'NONE', #75195, #115089, #25427 ) ;
#17657 = ADVANCED_FACE ( 'NONE', ( #126023 ), #56676, .T. ) ;
#17658 = CIRCLE ( 'NONE', #113825, 0.1000000000000002554 ) ;
#17659 = EDGE_LOOP ( 'NONE', ( #120921, #66177, #109760, #64649 ) ) ;
#17660 = DIRECTION ( 'NONE',  ( 0.000000000000000000, 0.000000000000000000, 1.000000000000000000 ) ) ;
#17661 = PLANE ( 'NONE',  #43410 ) ;
#17662 = PLANE ( 'NONE',  #19056 ) ;
#17663 = FACE_OUTER_BOUND ( 'NONE', #95038, .T. ) ;
#17664 = EDGE_CURVE ( 'NONE', #101480, #85870, #23238, .T. ) ;
#17665 = VERTEX_POINT ( 'NONE', #6877 ) ;
#17666 = EDGE_CURVE ( 'NONE', #122449, #34079, #59254, .T. ) ;
#17667 = DIRECTION ( 'NONE',  ( 0.000000000000000000, 1.000000000000000000, 0.000000000000000000 ) ) ;
#17668 = ORIENTED_EDGE ( 'NONE', *, *, #13919, .T. ) ;
#17669 = ORIENTED_EDGE ( 'NONE', *, *, #31691, .T. ) ;
#17670 = CARTESIAN_POINT ( 'NONE',  ( 11.44999999999991047, 2.500000000000000000, -2.411473670974877859 ) ) ;
#17671 = DIRECTION ( 'NONE',  ( 0.000000000000000000, 0.000000000000000000, -1.000000000000000000 ) ) ;
#17672 = FACE_BOUND ( 'NONE', #28304, .T. ) ;
#17673 = CARTESIAN_POINT ( 'NONE',  ( 17.50000000000000000, 2.500000000000000000, 4.000000000000000888 ) ) ;
#17674 = CONICAL_SURFACE ( 'NONE', #34428, 0.1000000000000002554, 0.003490658503988666988 ) ;
#17675 = CARTESIAN_POINT ( 'NONE',  ( -9.150000000000005684, 2.500000000000000000, 7.188010851410848723 ) ) ;
#17676 = DIRECTION ( 'NONE',  ( -0.000000000000000000, -1.000000000000000000, -0.000000000000000000 ) ) ;
#17677 = ORIENTED_EDGE ( 'NONE', *, *, #4776, .T. ) ;
#17678 = LINE ( 'NONE', #39302, #106974 ) ;
#17679 = CARTESIAN_POINT ( 'NONE',  ( 7.899999999999924860, 2.500000000000000000, -3.737306695894649700 ) ) ;
#17680 = ADVANCED_FACE ( 'NONE', ( #78893 ), #18008, .T. ) ;
#17681 = CARTESIAN_POINT ( 'NONE',  ( 4.599999999999938360, 2.500000000000000000, -0.6928203230275541413 ) ) ;
#17682 = CARTESIAN_POINT ( 'NONE',  ( -5.400000000000019895, 12.50000000000000000, -2.276824562219559311E-15 ) ) ;
#17683 = ORIENTED_EDGE ( 'NONE', *, *, #64746, .F. ) ;
#17684 = VECTOR ( 'NONE', #114946, 1000.000000000000000 ) ;
#17685 = CIRCLE ( 'NONE', #28166, 0.1000000000000002554 ) ;
#17686 = CARTESIAN_POINT ( 'NONE',  ( -8.950000000000009948, 12.50000000000000000, -6.841600689897072485 ) ) ;
#17687 = CARTESIAN_POINT ( 'NONE',  ( 11.84999999999990727, 12.50000000000000000, -2.446380397790840266 ) ) ;
#17688 = ORIENTED_EDGE ( 'NONE', *, *, #117204, .T. ) ;
#17689 = DIRECTION ( 'NONE',  ( 0.000000000000000000, 0.000000000000000000, -1.000000000000000000 ) ) ;
#17690 = FACE_OUTER_BOUND ( 'NONE', #127939, .T. ) ;
#17691 = FACE_BOUND ( 'NONE', #41565, .T. ) ;
#17692 = DIRECTION ( 'NONE',  ( -0.000000000000000000, 1.000000000000000000, -0.000000000000000000 ) ) ;
#17693 = ORIENTED_EDGE ( 'NONE', *, *, #32175, .F. ) ;
#17694 = DIRECTION ( 'NONE',  ( 0.000000000000000000, 1.000000000000000000, 0.000000000000000000 ) ) ;
#17695 = VECTOR ( 'NONE', #98845, 1000.000000000000000 ) ;
#17696 = ORIENTED_EDGE ( 'NONE', *, *, #101543, .F. ) ;
#17697 = ORIENTED_EDGE ( 'NONE', *, *, #30231, .F. ) ;
#17698 = CARTESIAN_POINT ( 'NONE',  ( 20.80940928220359609, 0.7000174339601031859, -4.161255421338316829 ) ) ;
#17699 = CARTESIAN_POINT ( 'NONE',  ( 187.0000000000000000, 0.000000000000000000, 7.700000000000000178 ) ) ;
#17700 = VERTEX_POINT ( 'NONE', #9491 ) ;
#17701 = DIRECTION ( 'NONE',  ( 0.000000000000000000, -0.000000000000000000, 1.000000000000000000 ) ) ;
#17702 = CARTESIAN_POINT ( 'NONE',  ( -2.100000000000033840, 2.500000000000000000, 5.122947341949749323 ) ) ;
#17703 = ADVANCED_FACE ( 'NONE', ( #48779 ), #21283, .T. ) ;
#17704 = AXIS2_PLACEMENT_3D ( 'NONE', #7865, #77264, #29459 ) ;
#17705 = AXIS2_PLACEMENT_3D ( 'NONE', #21728, #101576, #52461 ) ;
#17706 = CIRCLE ( 'NONE', #17417, 0.1000000000000002554 ) ;
#17707 = CARTESIAN_POINT ( 'NONE',  ( -4.119968255444916849E-14, 12.50000000000000000, 3.637306695894644726 ) ) ;
#17708 = ORIENTED_EDGE ( 'NONE', *, *, #92729, .T. ) ;
#17709 = SURFACE_STYLE_FILL_AREA ( #118495 ) ;
#17710 = CARTESIAN_POINT ( 'NONE',  ( -3.100000000000028511, 2.500000000000000000, -4.676537180435977881 ) ) ;
#17711 = CARTESIAN_POINT ( 'NONE',  ( -10.00000000000000711, 2.500000000000000000, -3.537306695894645969 ) ) ;
#17712 = CARTESIAN_POINT ( 'NONE',  ( 18.45986578164202996, -0.7763536479255006562, -4.045836815165628764 ) ) ;
#17713 = ORIENTED_EDGE ( 'NONE', *, *, #3450, .F. ) ;
#17714 = CARTESIAN_POINT ( 'NONE',  ( 11.64999999999990621, 12.50000000000000000, 6.495190528383297135 ) ) ;
#17715 = VERTEX_POINT ( 'NONE', #7540 ) ;
#17716 = DIRECTION ( 'NONE',  ( -0.000000000000000000, -1.000000000000000000, -0.000000000000000000 ) ) ;
#17717 = VERTEX_POINT ( 'NONE', #108953 ) ;
#17718 = CARTESIAN_POINT ( 'NONE',  ( 14.99999999999989342, 2.500000000000000000, -0.7928203230275542301 ) ) ;
#17719 = CARTESIAN_POINT ( 'NONE',  ( 87.49999999999998579, -5.708722954879575262, 4.899943752027914989 ) ) ;
#17720 = DIRECTION ( 'NONE',  ( -0.000000000000000000, 1.000000000000000000, -0.000000000000000000 ) ) ;
#17722 = DIRECTION ( 'NONE',  ( 0.000000000000000000, -0.000000000000000000, 1.000000000000000000 ) ) ;
#17721 = AXIS2_PLACEMENT_3D ( 'NONE', #77199, #37912, #105369 ) ;
#17723 = ORIENTED_EDGE ( 'NONE', *, *, #9371, .T. ) ;
#17724 = VECTOR ( 'NONE', #41655, 1000.000000000000000 ) ;
#17725 = CARTESIAN_POINT ( 'NONE',  ( 3.099999999999945466, 2.500000000000000000, -3.983716857408426293 ) ) ;
#17726 = CARTESIAN_POINT ( 'NONE',  ( -11.25000000000000178, 2.500000000000000000, -1.372243186433546036 ) ) ;
#17727 = AXIS2_PLACEMENT_3D ( 'NONE', #9423, #8752, #99746 ) ;
#17728 = VECTOR ( 'NONE', #78938, 1000.000000000000000 ) ;
#17729 = CARTESIAN_POINT ( 'NONE',  ( -0.8000000000000376810, 2.500000000000000000, -4.330127018922201643 ) ) ;
#17730 = DIRECTION ( 'NONE',  ( 0.000000000000000000, 1.000000000000000000, 0.000000000000000000 ) ) ;
#17731 = CARTESIAN_POINT ( 'NONE',  ( 4.149999999999938183, 2.500000000000000000, 7.188010851410848723 ) ) ;
#17732 = VECTOR ( 'NONE', #81391, 1000.000000000000000 ) ;
#17733 = ORIENTED_EDGE ( 'NONE', *, *, #33326, .F. ) ;
#17735 = VERTEX_POINT ( 'NONE', #19958 ) ;
#17734 = VECTOR ( 'NONE', #124317, 1000.000000000000000 ) ;
#17737 = DIRECTION ( 'NONE',  ( -0.000000000000000000, 1.000000000000000000, -0.000000000000000000 ) ) ;
#17736 = VECTOR ( 'NONE', #20531, 1000.000000000000000 ) ;
#17738 = ORIENTED_EDGE ( 'NONE', *, *, #63174, .F. ) ;
#17740 = LINE ( 'NONE', #57689, #17979 ) ;
#17739 = B_SPLINE_CURVE_WITH_KNOTS ( 'NONE', 3,
 ( #126101, #35797, #84238, #55437, #5032, #86822, #86158, #46251, #37098, #35173 ),
 .UNSPECIFIED., .F., .F.,
 ( 4, 2, 2, 2, 4 ),
 ( -0.0001133383185230014501, 0.01648989986483693007, 0.03309313804819685734, 0.04969637623155678807, 0.06629961441491671881 ),
 .UNSPECIFIED. ) ;
#17743 = ORIENTED_EDGE ( 'NONE', *, *, #2256, .F. ) ;
#17742 = ORIENTED_EDGE ( 'NONE', *, *, #25479, .F. ) ;
#17741 = VECTOR ( 'NONE', #6354, 1000.000000000000000 ) ;
#17744 = ORIENTED_EDGE ( 'NONE', *, *, #97126, .T. ) ;
#17745 = CARTESIAN_POINT ( 'NONE',  ( -9.600000000000006750, 12.50000000000000000, 0.6277270498435120194 ) ) ;
#17746 = AXIS2_PLACEMENT_3D ( 'NONE', #56719, #18752, #58052 ) ;
#17748 = ADVANCED_FACE ( 'NONE', ( #78243 ), #31766, .T. ) ;
#17747 = CARTESIAN_POINT ( 'NONE',  ( 8.749999999999920064, 12.50000000000000000, -2.922977105672691422 ) ) ;
#17749 = DIRECTION ( 'NONE',  ( 0.000000000000000000, 1.000000000000000000, 0.000000000000000000 ) ) ;
#17750 = CARTESIAN_POINT ( 'NONE',  ( -6.450000000000014388, 2.500000000000000000, 1.718653347947321386 ) ) ;
#17751 = PLANE ( 'NONE',  #60630 ) ;
#17752 = AXIS2_PLACEMENT_3D ( 'NONE', #1056, #109731, #69804 ) ;
#17753 = CARTESIAN_POINT ( 'NONE',  ( -5.650000000000019895, 12.50000000000000000, 2.576566944158910744 ) ) ;
#17754 = CARTESIAN_POINT ( 'NONE',  ( -10.20000000000000462, 2.500000000000000000, 4.776537180435972196 ) ) ;
#17755 = EDGE_CURVE ( 'NONE', #38783, #5075, #50519, .T. ) ;
#17756 = ORIENTED_EDGE ( 'NONE', *, *, #62244, .T. ) ;
#17757 = EDGE_CURVE ( 'NONE', #64023, #98238, #29147, .T. ) ;
#17758 = DIRECTION ( 'NONE',  ( 0.000000000000000000, 1.000000000000000000, 0.000000000000000000 ) ) ;
#17759 = ORIENTED_EDGE ( 'NONE', *, *, #27403, .T. ) ;
#17760 = ORIENTED_EDGE ( 'NONE', *, *, #49770, .F. ) ;
#17761 = VERTEX_POINT ( 'NONE', #59903 ) ;
#17762 = EDGE_LOOP ( 'NONE', ( #32980, #101069 ) ) ;
#17763 = EDGE_CURVE ( 'NONE', #64667, #104068, #69042, .T. ) ;
#17765 = ADVANCED_FACE ( 'NONE', ( #107022 ), #33803, .T. ) ;
#17764 = CARTESIAN_POINT ( 'NONE',  ( -10.84999999999999964, 12.50000000000000000, 5.802370205355744659 ) ) ;
#17767 = ORIENTED_EDGE ( 'NONE', *, *, #96524, .F. ) ;
#17766 = EDGE_CURVE ( 'NONE', #114247, #10596, #18658, .T. ) ;
#17768 = ORIENTED_EDGE ( 'NONE', *, *, #62106, .T. ) ;
#17769 = EDGE_CURVE ( 'NONE', #1435, #103138, #115347, .T. ) ;
#17770 = CIRCLE ( 'NONE', #32483, 0.1000000000000002554 ) ;
#17771 = DIRECTION ( 'NONE',  ( 0.000000000000000000, 0.000000000000000000, 1.000000000000000000 ) ) ;
#17772 = DIRECTION ( 'NONE',  ( -0.000000000000000000, 1.000000000000000000, -0.000000000000000000 ) ) ;
#17773 = DIRECTION ( 'NONE',  ( 0.000000000000000000, 1.000000000000000000, 0.000000000000000000 ) ) ;
#17774 = FACE_OUTER_BOUND ( 'NONE', #119639, .T. ) ;
#17775 = DIRECTION ( 'NONE',  ( 0.000000000000000000, 0.000000000000000000, 1.000000000000000000 ) ) ;
#17776 = VERTEX_POINT ( 'NONE', #10137 ) ;
#17777 = CARTESIAN_POINT ( 'NONE',  ( -4.294451507785425339E-14, 12.50000000000000000, 4.957854068765711553 ) ) ;
#17778 = VECTOR ( 'NONE', #120126, 1000.000000000000000 ) ;
#17779 = CIRCLE ( 'NONE', #38654, 0.06509327318403745899 ) ;
#17780 = ORIENTED_EDGE ( 'NONE', *, *, #124543, .F. ) ;
#17781 = CARTESIAN_POINT ( 'NONE',  ( -12.29999999999999538, 2.500000000000000000, 4.776537180435972196 ) ) ;
#17782 = EDGE_LOOP ( 'NONE', ( #128177, #26734, #108737, #88245 ) ) ;
#17783 = CARTESIAN_POINT ( 'NONE',  ( 11.04999999999991189, 2.500000000000000000, -2.411473670974877859 ) ) ;
#17784 = ORIENTED_EDGE ( 'NONE', *, *, #118962, .T. ) ;
#17785 = EDGE_LOOP ( 'NONE', ( #28389, #21369, #64760, #68131 ) ) ;
#17786 = DIRECTION ( 'NONE',  ( 0.000000000000000000, 0.000000000000000000, 1.000000000000000000 ) ) ;
#17787 = DIRECTION ( 'NONE',  ( 0.000000000000000000, 0.000000000000000000, -1.000000000000000000 ) ) ;
#17788 = CIRCLE ( 'NONE', #32498, 0.1000000000000002554 ) ;
#17789 = DIRECTION ( 'NONE',  ( -0.000000000000000000, 1.000000000000000000, -0.000000000000000000 ) ) ;
#17790 = CARTESIAN_POINT ( 'NONE',  ( -13.34999999999999076, 12.50000000000000000, -2.857883832488651521 ) ) ;
#17791 = CIRCLE ( 'NONE', #45005, 0.1000000000000000472 ) ;
#17792 = CARTESIAN_POINT ( 'NONE',  ( 13.34999999999990017, 12.50000000000000000, 2.857883832488649301 ) ) ;
#17793 = EDGE_LOOP ( 'NONE', ( #122567, #125241 ) ) ;
#17794 = DIRECTION ( 'NONE',  ( -4.274815082592931898E-19, -0.9999939076577903929, -0.003490651415223739937 ) ) ;
#17795 = DIRECTION ( 'NONE',  ( -0.000000000000000000, 1.000000000000000000, -0.000000000000000000 ) ) ;
#17796 = EDGE_CURVE ( 'NONE', #20424, #11168, #88017, .T. ) ;
#17797 = CARTESIAN_POINT ( 'NONE',  ( 1.249999999999988454, 2.500000000000000000, 2.265063509461097357 ) ) ;
#17798 = CARTESIAN_POINT ( 'NONE',  ( 149.5981739382431783, 0.5000000000000000000, -1.703575533167231537 ) ) ;
#17799 = DIRECTION ( 'NONE',  ( 0.000000000000000000, 0.000000000000000000, 1.000000000000000000 ) ) ;
#17800 = ORIENTED_EDGE ( 'NONE', *, *, #29308, .T. ) ;
#17801 = AXIS2_PLACEMENT_3D ( 'NONE', #19991, #19320, #97889 ) ;
#17802 = ORIENTED_EDGE ( 'NONE', *, *, #121783, .T. ) ;
#17803 = EDGE_CURVE ( 'NONE', #5314, #125017, #76946, .T. ) ;
#17804 = CARTESIAN_POINT ( 'NONE',  ( -2.700000000000030820, 12.50000000000000000, -3.918623584224389056 ) ) ;
#17805 = EDGE_CURVE ( 'NONE', #69443, #112225, #104893, .T. ) ;
#17806 = EDGE_CURVE ( 'NONE', #120000, #102762, #2386, .T. ) ;
#17807 = VERTEX_POINT ( 'NONE', #37671 ) ;
#17808 = CARTESIAN_POINT ( 'NONE',  ( -5.650000000000023448, 12.50000000000000000, -1.818653347947326138 ) ) ;
#17809 = PLANE ( 'NONE',  #12496 ) ;
#17810 = ADVANCED_FACE ( 'NONE', ( #57953 ), #19110, .T. ) ;
#17811 = ORIENTED_EDGE ( 'NONE', *, *, #39272, .F. ) ;
#17812 = CARTESIAN_POINT ( 'NONE',  ( 185.2083333333333144, -4.445597072760115509, -7.700000000000001954 ) ) ;
#17813 = DIRECTION ( 'NONE',  ( 0.000000000000000000, 1.000000000000000000, 0.000000000000000000 ) ) ;
#17814 = ADVANCED_FACE ( 'NONE', ( #28491 ), #127969, .T. ) ;
#17815 = DIRECTION ( 'NONE',  ( 0.000000000000000000, -0.000000000000000000, 1.000000000000000000 ) ) ;
#17816 = CONICAL_SURFACE ( 'NONE', #34576, 0.1000000000000002554, 0.003490658503988666988 ) ;
#17817 = FACE_OUTER_BOUND ( 'NONE', #101641, .T. ) ;
#17818 = VERTEX_POINT ( 'NONE', #128648 ) ;
#17819 = ADVANCED_FACE ( 'NONE', ( #40241 ), #80162, .T. ) ;
#17820 = ADVANCED_FACE ( 'NONE', ( #122661 ), #92289, .T. ) ;
#17821 = ADVANCED_FACE ( 'NONE', ( #91270 ), #72289, .T. ) ;
#17823 = CARTESIAN_POINT ( 'NONE',  ( -6.900000000000015454, 2.500000000000000000, 4.676537180435972552 ) ) ;
#17822 = AXIS2_PLACEMENT_3D ( 'NONE', #81699, #73809, #72548 ) ;
#17824 = CARTESIAN_POINT ( 'NONE',  ( -3.350000000000028511, 2.500000000000000000, -1.472243186433550122 ) ) ;
#17825 = CIRCLE ( 'NONE', #99316, 0.06509327318403745899 ) ;
#17826 = EDGE_LOOP ( 'NONE', ( #123734, #69264, #42843, #37200 ) ) ;
#17827 = AXIS2_PLACEMENT_3D ( 'NONE', #76678, #57016, #56378 ) ;
#17828 = DIRECTION ( 'NONE',  ( 0.000000000000000000, 0.000000000000000000, 1.000000000000000000 ) ) ;
#17829 = CARTESIAN_POINT ( 'NONE',  ( 0.5999999999999551248, 2.500000000000000000, -4.676537180435978769 ) ) ;
#17830 = EDGE_CURVE ( 'NONE', #78336, #22216, #46317, .T. ) ;
#17831 = DIRECTION ( 'NONE',  ( -0.000000000000000000, 1.000000000000000000, -0.000000000000000000 ) ) ;
#17832 = AXIS2_PLACEMENT_3D ( 'NONE', #38073, #126461, #78657 ) ;
#17833 = AXIS2_PLACEMENT_3D ( 'NONE', #87600, #127541, #59473 ) ;
#17834 = EDGE_LOOP ( 'NONE', ( #82588, #117974, #101761, #49621 ) ) ;
#17835 = AXIS2_PLACEMENT_3D ( 'NONE', #122596, #102944, #32946 ) ;
#17836 = DIRECTION ( 'NONE',  ( 0.000000000000000000, 0.000000000000000000, 1.000000000000000000 ) ) ;
#17837 = AXIS2_PLACEMENT_3D ( 'NONE', #57271, #55338, #85434 ) ;
#17838 = ORIENTED_EDGE ( 'NONE', *, *, #26404, .T. ) ;
#17839 = PLANE ( 'NONE',  #64726 ) ;
#17840 = CARTESIAN_POINT ( 'NONE',  ( -12.69999999999999396, 12.50000000000000000, 0.3464101615137776813 ) ) ;
#17841 = CARTESIAN_POINT ( 'NONE',  ( -14.34999999999998543, 12.50000000000000000, -2.446380397790838046 ) ) ;
#17842 = ORIENTED_EDGE ( 'NONE', *, *, #30634, .T. ) ;
#17843 = AXIS2_PLACEMENT_3D ( 'NONE', #43579, #86033, #125970 ) ;
#17844 = VECTOR ( 'NONE', #62972, 1000.000000000000000 ) ;
#17845 = CARTESIAN_POINT ( 'NONE',  ( 15.39999999999989200, 2.500000000000000000, 0.5928203230275495006 ) ) ;
#17846 = AXIS2_PLACEMENT_3D ( 'NONE', #70892, #51271, #50593 ) ;
#17847 = DIRECTION ( 'NONE',  ( -0.000000000000000000, 1.000000000000000000, -0.000000000000000000 ) ) ;
#17848 = ORIENTED_EDGE ( 'NONE', *, *, #40430, .F. ) ;
#17849 = DIRECTION ( 'NONE',  ( 0.000000000000000000, 1.000000000000000000, 0.000000000000000000 ) ) ;
#17850 = ORIENTED_EDGE ( 'NONE', *, *, #42664, .T. ) ;
#17851 = PLANE ( 'NONE',  #114225 ) ;
#17852 = EDGE_LOOP ( 'NONE', ( #98182, #31989 ) ) ;
#17853 = CARTESIAN_POINT ( 'NONE',  ( 0.000000000000000000, 1.500000000000000000, 9.000000000000001776 ) ) ;
#17854 = DIRECTION ( 'NONE',  ( 0.000000000000000000, 0.000000000000000000, 1.000000000000000000 ) ) ;
#17855 = ORIENTED_EDGE ( 'NONE', *, *, #98166, .F. ) ;
#17856 = ORIENTED_EDGE ( 'NONE', *, *, #27853, .F. ) ;
#17857 = DIRECTION ( 'NONE',  ( 0.000000000000000000, 0.000000000000000000, 1.000000000000000000 ) ) ;
#17858 = CARTESIAN_POINT ( 'NONE',  ( -4.350000000000027178, 12.50000000000000000, -6.776507416713039689 ) ) ;
#17859 = AXIS2_PLACEMENT_3D ( 'NONE', #79872, #39957, #30793 ) ;
#17860 = VERTEX_POINT ( 'NONE', #22549 ) ;
#17861 = CARTESIAN_POINT ( 'NONE',  ( 4.349999999999939249, 2.500000000000000000, 2.511473670974873507 ) ) ;
#17862 = FACE_OUTER_BOUND ( 'NONE', #48028, .T. ) ;
#17863 = EDGE_CURVE ( 'NONE', #126669, #115818, #71442, .T. ) ;
#17864 = DIRECTION ( 'NONE',  ( 0.000000000000000000, 1.000000000000000000, 0.000000000000000000 ) ) ;
#17865 = DIRECTION ( 'NONE',  ( 0.000000000000000000, 1.000000000000000000, 0.000000000000000000 ) ) ;
#17866 = CARTESIAN_POINT ( 'NONE',  ( -9.550000000000006040, 2.500000000000000000, 2.065063509461097624 ) ) ;
#17867 = CIRCLE ( 'NONE', #53394, 0.06509327318403745899 ) ;
#17868 = CARTESIAN_POINT ( 'NONE',  ( 8.949999999999915801, 12.50000000000000000, 6.906693963081109722 ) ) ;
#17869 = CIRCLE ( 'NONE', #22109, 0.1000000000000002554 ) ;
#17870 = AXIS2_PLACEMENT_3D ( 'NONE', #104472, #36400, #56007 ) ;
#17871 = ORIENTED_EDGE ( 'NONE', *, *, #29173, .F. ) ;
#17872 = ORIENTED_EDGE ( 'NONE', *, *, #14243, .T. ) ;
#17873 = VERTEX_POINT ( 'NONE', #20601 ) ;
#17874 = EDGE_LOOP ( 'NONE', ( #101890, #101951, #78743, #126517 ) ) ;
#17875 = CARTESIAN_POINT ( 'NONE',  ( -2.900000000000029221, 12.50000000000000000, -4.395220292106239768 ) ) ;
#17876 = DIRECTION ( 'NONE',  ( 0.000000000000000000, 0.000000000000000000, 1.000000000000000000 ) ) ;
#17877 = DIRECTION ( 'NONE',  ( -0.000000000000000000, -1.000000000000000000, -0.000000000000000000 ) ) ;
#17878 = ORIENTED_EDGE ( 'NONE', *, *, #13674, .T. ) ;
#17879 = ADVANCED_FACE ( 'NONE', ( #51367 ), #113214, .T. ) ;
#17880 = FACE_BOUND ( 'NONE', #54738, .T. ) ;
#17881 = EDGE_LOOP ( 'NONE', ( #27967, #1167, #64929, #58686 ) ) ;
#17882 = DIRECTION ( 'NONE',  ( 0.000000000000000000, 1.000000000000000000, 0.000000000000000000 ) ) ;
#17883 = CARTESIAN_POINT ( 'NONE',  ( -8.150000000000012790, 12.50000000000000000, 1.753560074763284016 ) ) ;
#17884 = VECTOR ( 'NONE', #49099, 1000.000000000000000 ) ;
#17885 = DIRECTION ( 'NONE',  ( 0.000000000000000000, 0.000000000000000000, -1.000000000000000000 ) ) ;
#17886 = CARTESIAN_POINT ( 'NONE',  ( -7.500000000000016875, 2.500000000000000000, -3.537306695894649966 ) ) ;
#17887 = AXIS2_PLACEMENT_3D ( 'NONE', #112396, #43036, #50256 ) ;
#17888 = FACE_OUTER_BOUND ( 'NONE', #18005, .T. ) ;
#17889 = FACE_OUTER_BOUND ( 'NONE', #87233, .T. ) ;
#17890 = FACE_OUTER_BOUND ( 'NONE', #59828, .T. ) ;
#17891 = DIRECTION ( 'NONE',  ( -0.000000000000000000, 1.000000000000000000, -0.000000000000000000 ) ) ;
#17892 = DIRECTION ( 'NONE',  ( -0.000000000000000000, -1.000000000000000000, -0.000000000000000000 ) ) ;
#17893 = DIRECTION ( 'NONE',  ( 0.000000000000000000, -0.000000000000000000, 1.000000000000000000 ) ) ;
#17894 = AXIS2_PLACEMENT_3D ( 'NONE', #801, #99664, #87879 ) ;
#17895 = EDGE_LOOP ( 'NONE', ( #34435, #91252 ) ) ;
#17896 = ORIENTED_EDGE ( 'NONE', *, *, #37823, .F. ) ;
#17897 = AXIS2_PLACEMENT_3D ( 'NONE', #98372, #8693, #48651 ) ;
#17898 = ORIENTED_EDGE ( 'NONE', *, *, #36439, .F. ) ;
#17899 = VERTEX_POINT ( 'NONE', #63095 ) ;
#17900 = CARTESIAN_POINT ( 'NONE',  ( 17.50000000000000000, -2.500000000000000000, -2.922290670087884124 ) ) ;
#17901 = CARTESIAN_POINT ( 'NONE',  ( 0.6499999999999561684, 2.500000000000000000, 2.511473670974873507 ) ) ;
#17903 = ORIENTED_EDGE ( 'NONE', *, *, #107218, .T. ) ;
#17902 = ORIENTED_EDGE ( 'NONE', *, *, #27216, .F. ) ;
#17904 = EDGE_LOOP ( 'NONE', ( #109604, #64135 ) ) ;
#17905 = CARTESIAN_POINT ( 'NONE',  ( 1.249999999999953815, 12.50000000000000000, -2.857883832488653741 ) ) ;
#17906 = ADVANCED_FACE ( 'NONE', ( #33015 ), #69295, .T. ) ;
#17907 = FACE_OUTER_BOUND ( 'NONE', #47444, .T. ) ;
#17908 = CARTESIAN_POINT ( 'NONE',  ( -10.00000000000000355, 12.50000000000000000, -0.6928203230275541413 ) ) ;
#17909 = DIRECTION ( 'NONE',  ( 0.000000000000000000, 0.000000000000000000, 1.000000000000000000 ) ) ;
#17910 = FACE_OUTER_BOUND ( 'NONE', #62186, .T. ) ;
#17911 = DIRECTION ( 'NONE',  ( 1.000000000000000000, 0.000000000000000000, 8.881784197001235560E-16 ) ) ;
#17912 = AXIS2_PLACEMENT_3D ( 'NONE', #128887, #39219, #27413 ) ;
#17913 = EDGE_LOOP ( 'NONE', ( #49271, #123797 ) ) ;
#17914 = EDGE_CURVE ( 'NONE', #54140, #96322, #56759, .T. ) ;
#17915 = CARTESIAN_POINT ( 'NONE',  ( 7.899999999999921307, 12.50000000000000000, -0.06509327318403980434 ) ) ;
#17916 = ORIENTED_EDGE ( 'NONE', *, *, #63030, .T. ) ;
#17918 = EDGE_LOOP ( 'NONE', ( #119085, #128669 ) ) ;
#17917 = CIRCLE ( 'NONE', #91079, 0.1000000000000002554 ) ;
#17919 = VERTEX_POINT ( 'NONE', #1586 ) ;
#17920 = AXIS2_PLACEMENT_3D ( 'NONE', #82704, #122618, #73496 ) ;
#17921 = EDGE_CURVE ( 'NONE', #11906, #45961, #123668, .T. ) ;
#17923 = EDGE_CURVE ( 'NONE', #56262, #98108, #14996, .T. ) ;
#17922 = DIRECTION ( 'NONE',  ( 0.000000000000000000, -0.9999939076577903929, 0.003490651415223739937 ) ) ;
#17926 = VERTEX_POINT ( 'NONE', #50697 ) ;
#17925 = EDGE_CURVE ( 'NONE', #80384, #114882, #88153, .T. ) ;
#17924 = APPLICATION_CONTEXT ( 'automotive_design' ) ;
#17927 = ADVANCED_FACE ( 'NONE', ( #952 ), #17033, .T. ) ;
#17929 = ORIENTED_EDGE ( 'NONE', *, *, #46398, .T. ) ;
#17928 = EDGE_CURVE ( 'NONE', #15359, #6313, #53295, .T. ) ;
#17930 = CARTESIAN_POINT ( 'NONE',  ( -2.100000000000033396, 2.500000000000000000, -0.6928203230275542523 ) ) ;
#17931 = DIRECTION ( 'NONE',  ( 0.000000000000000000, 0.000000000000000000, -1.000000000000000000 ) ) ;
#17932 = DIRECTION ( 'NONE',  ( 0.000000000000000000, 0.000000000000000000, -1.000000000000000000 ) ) ;
#17933 = CARTESIAN_POINT ( 'NONE',  ( 8.549999999999924327, 2.500000000000000000, -6.741600689897077281 ) ) ;
#17934 = FACE_OUTER_BOUND ( 'NONE', #125302, .T. ) ;
#17935 = EDGE_CURVE ( 'NONE', #48604, #10563, #52001, .T. ) ;
#17936 = ORIENTED_EDGE ( 'NONE', *, *, #58141, .T. ) ;
#17937 = DIRECTION ( 'NONE',  ( 0.000000000000000000, 1.000000000000000000, 0.000000000000000000 ) ) ;
#17938 = EDGE_CURVE ( 'NONE', #26160, #64274, #110895, .T. ) ;
#17939 = AXIS2_PLACEMENT_3D ( 'NONE', #77521, #48080, #117418 ) ;
#17940 = VECTOR ( 'NONE', #68762, 1000.000000000000000 ) ;
#17941 = EDGE_CURVE ( 'NONE', #22615, #116464, #81911, .T. ) ;
#17942 = ORIENTED_EDGE ( 'NONE', *, *, #66101, .T. ) ;
#17943 = FACE_OUTER_BOUND ( 'NONE', #53416, .T. ) ;
#17944 = CIRCLE ( 'NONE', #109897, 0.06509327318403745899 ) ;
#17945 = ORIENTED_EDGE ( 'NONE', *, *, #107795, .F. ) ;
#17946 = CARTESIAN_POINT ( 'NONE',  ( 110.5217483863200414, 7.548960721389698314, -4.329587527523654167 ) ) ;
#17947 = CARTESIAN_POINT ( 'NONE',  ( -4.150000000000025224, 2.500000000000000000, 6.495190528383297135 ) ) ;
#17948 = CONICAL_SURFACE ( 'NONE', #89053, 0.1000000000000002554, 0.003490658503988666988 ) ;
#17949 = ORIENTED_EDGE ( 'NONE', *, *, #121327, .T. ) ;
#17950 = DIRECTION ( 'NONE',  ( -0.000000000000000000, -1.000000000000000000, -0.000000000000000000 ) ) ;
#17951 = CARTESIAN_POINT ( 'NONE',  ( -6.850000000000017408, 12.50000000000000000, -1.818653347947325916 ) ) ;
#17952 = ORIENTED_EDGE ( 'NONE', *, *, #2514, .T. ) ;
#17953 = DIRECTION ( 'NONE',  ( -0.000000000000000000, -1.000000000000000000, -0.000000000000000000 ) ) ;
#17954 = ORIENTED_EDGE ( 'NONE', *, *, #24758, .T. ) ;
#17955 = EDGE_LOOP ( 'NONE', ( #47487, #76341 ) ) ;
#17956 = CARTESIAN_POINT ( 'NONE',  ( 5.849999999999933031, 12.50000000000000000, -1.407149913249512663 ) ) ;
#17957 = CARTESIAN_POINT ( 'NONE',  ( 10.19999999999991402, 2.500000000000000000, 0.4464101615137735513 ) ) ;
#17958 = CARTESIAN_POINT ( 'NONE',  ( 186.6302083336747160, -4.367472073101514418, -7.564683531250002702 ) ) ;
#17959 = CONICAL_SURFACE ( 'NONE', #120376, 0.09999999999999982514, 0.003490658503988666988 ) ;
#17960 = CARTESIAN_POINT ( 'NONE',  ( -11.24999999999999822, 12.50000000000000000, 1.472243186433545459 ) ) ;
#17961 = CARTESIAN_POINT ( 'NONE',  ( 9.349999999999919709, 2.500000000000000000, 2.411473670974873862 ) ) ;
#17962 = DIRECTION ( 'NONE',  ( -0.000000000000000000, 1.000000000000000000, -0.000000000000000000 ) ) ;
#17963 = AXIS2_PLACEMENT_3D ( 'NONE', #100786, #122390, #51080 ) ;
#17964 = VECTOR ( 'NONE', #2083, 1000.000000000000000 ) ;
#17965 = VERTEX_POINT ( 'NONE', #91915 ) ;
#17966 = DIRECTION ( 'NONE',  ( 0.000000000000000000, 0.000000000000000000, -1.000000000000000000 ) ) ;
#17967 = DIRECTION ( 'NONE',  ( 0.000000000000000000, -0.000000000000000000, 1.000000000000000000 ) ) ;
#17968 = AXIS2_PLACEMENT_3D ( 'NONE', #117820, #47826, #28175 ) ;
#17969 = ORIENTED_EDGE ( 'NONE', *, *, #93580, .T. ) ;
#17970 = DIRECTION ( 'NONE',  ( -0.000000000000000000, -1.000000000000000000, -0.000000000000000000 ) ) ;
#17971 = FACE_OUTER_BOUND ( 'NONE', #28141, .T. ) ;
#17972 = DIRECTION ( 'NONE',  ( 0.000000000000000000, 0.000000000000000000, 1.000000000000000000 ) ) ;
#17973 = EDGE_CURVE ( 'NONE', #64554, #81253, #117398, .T. ) ;
#17974 = DIRECTION ( 'NONE',  ( 0.000000000000000000, 1.000000000000000000, 0.000000000000000000 ) ) ;
#17975 = DIRECTION ( 'NONE',  ( 0.000000000000000000, 0.000000000000000000, 1.000000000000000000 ) ) ;
#17976 = ORIENTED_EDGE ( 'NONE', *, *, #113289, .F. ) ;
#17977 = CONICAL_SURFACE ( 'NONE', #107863, 0.1000000000000002554, 0.003490658503988666988 ) ;
#17978 = EDGE_CURVE ( 'NONE', #104697, #97467, #58947, .T. ) ;
#17981 = ADVANCED_FACE ( 'NONE', ( #103681 ), #123939, .T. ) ;
#17980 = VECTOR ( 'NONE', #74084, 1000.000000000000000 ) ;
#17979 = VECTOR ( 'NONE', #68130, 1000.000000000000000 ) ;
#17982 = DIRECTION ( 'NONE',  ( 0.000000000000000000, 0.000000000000000000, 1.000000000000000000 ) ) ;
#17983 = DIRECTION ( 'NONE',  ( 0.000000000000000000, -0.000000000000000000, 1.000000000000000000 ) ) ;
#17984 = EDGE_LOOP ( 'NONE', ( #98974, #120625, #78155, #58723 ) ) ;
#17985 = EDGE_CURVE ( 'NONE', #16266, #22601, #54816, .T. ) ;
#17986 = DIRECTION ( 'NONE',  ( 0.000000000000000000, 0.000000000000000000, 1.000000000000000000 ) ) ;
#17987 = ORIENTED_EDGE ( 'NONE', *, *, #125059, .F. ) ;
#17988 = ORIENTED_EDGE ( 'NONE', *, *, #82659, .T. ) ;
#17989 = LINE ( 'NONE', #17324, #105205 ) ;
#17990 = VERTEX_POINT ( 'NONE', #23825 ) ;
#17991 = PLANE ( 'NONE',  #67464 ) ;
#17992 = CARTESIAN_POINT ( 'NONE',  ( -11.89999999999999503, 2.500000000000000000, 3.883716857408420431 ) ) ;
#17993 = CARTESIAN_POINT ( 'NONE',  ( 0.5999999999999547917, 12.50000000000000000, 4.048810130592458201 ) ) ;
#17994 = EDGE_LOOP ( 'NONE', ( #30889, #24018, #13911, #69106 ) ) ;
#17995 = FACE_OUTER_BOUND ( 'NONE', #20492, .T. ) ;
#17997 = VERTEX_POINT ( 'NONE', #96246 ) ;
#17996 = DIRECTION ( 'NONE',  ( -0.000000000000000000, 1.000000000000000000, -0.000000000000000000 ) ) ;
#17998 = CARTESIAN_POINT ( 'NONE',  ( -8.150000000000012790, 12.50000000000000000, 1.883746621131358934 ) ) ;
#17999 = CARTESIAN_POINT ( 'NONE',  ( -10.65000000000000213, 2.500000000000000000, 6.048780366869520364 ) ) ;
#18000 = ADVANCED_FACE ( 'NONE', ( #47171 ), #75647, .T. ) ;
#18001 = ORIENTED_EDGE ( 'NONE', *, *, #120243, .T. ) ;
#18002 = AXIS2_PLACEMENT_3D ( 'NONE', #61044, #51255, #1473 ) ;
#18003 = ORIENTED_EDGE ( 'NONE', *, *, #5688, .F. ) ;
#18004 = CIRCLE ( 'NONE', #51479, 0.06509327318403745899 ) ;
#18005 = EDGE_LOOP ( 'NONE', ( #22441, #25831 ) ) ;
#18006 = DIRECTION ( 'NONE',  ( -0.000000000000000000, 1.000000000000000000, -0.000000000000000000 ) ) ;
#18007 = CARTESIAN_POINT ( 'NONE',  ( 3.549999999999943867, 2.500000000000000000, -1.718653347947326049 ) ) ;
#18008 = PLANE ( 'NONE',  #12848 ) ;
#18009 = FACE_BOUND ( 'NONE', #122218, .T. ) ;
#18010 = ORIENTED_EDGE ( 'NONE', *, *, #127728, .T. ) ;
#18011 = CARTESIAN_POINT ( 'NONE',  ( 14.99999999999989164, 12.50000000000000000, 0.6928203230275494784 ) ) ;
#18012 = DIRECTION ( 'NONE',  ( 0.000000000000000000, 0.000000000000000000, 1.000000000000000000 ) ) ;
#18013 = VERTEX_POINT ( 'NONE', #7872 ) ;
#18014 = AXIS2_PLACEMENT_3D ( 'NONE', #13457, #93323, #123412 ) ;
#18015 = CARTESIAN_POINT ( 'NONE',  ( 184.9583333333332860, 4.445597072760175905, 7.699999999999896261 ) ) ;
#18016 = EDGE_CURVE ( 'NONE', #58128, #119493, #27617, .T. ) ;
#18017 = CARTESIAN_POINT ( 'NONE',  ( 105.5000000000000142, 0.000000000000000000, 0.000000000000000000 ) ) ;
#18018 = DIRECTION ( 'NONE',  ( -4.274815082592931898E-19, -0.9999939076577903929, -0.003490651415223739937 ) ) ;
#18019 = DIRECTION ( 'NONE',  ( 0.000000000000000000, 0.000000000000000000, -1.000000000000000000 ) ) ;
#18020 = FACE_OUTER_BOUND ( 'NONE', #56053, .T. ) ;
#18022 = AXIS2_PLACEMENT_3D ( 'NONE', #100908, #42675, #81289 ) ;
#18021 = AXIS2_PLACEMENT_3D ( 'NONE', #5403, #83343, #52574 ) ;
#18023 = AXIS2_PLACEMENT_3D ( 'NONE', #81206, #58985, #91658 ) ;
#18024 = EDGE_LOOP ( 'NONE', ( #112406, #20226, #60341, #20009 ) ) ;
#18025 = ORIENTED_EDGE ( 'NONE', *, *, #73769, .F. ) ;
#18026 = ORIENTED_EDGE ( 'NONE', *, *, #28281, .F. ) ;
#18027 = ORIENTED_EDGE ( 'NONE', *, *, #39689, .F. ) ;
#18028 = ORIENTED_EDGE ( 'NONE', *, *, #49861, .F. ) ;
#18029 = FACE_OUTER_BOUND ( 'NONE', #31856, .T. ) ;
#18030 = DIRECTION ( 'NONE',  ( 0.000000000000000000, 0.000000000000000000, 1.000000000000000000 ) ) ;
#18031 = ORIENTED_EDGE ( 'NONE', *, *, #64476, .F. ) ;
#18032 = ADVANCED_FACE ( 'NONE', ( #104313 ), #56861, .T. ) ;
#18033 = FACE_BOUND ( 'NONE', #707, .T. ) ;
#18034 = CARTESIAN_POINT ( 'NONE',  ( 129.5000000000000000, 1.375000000000000000, 7.576237522675751457 ) ) ;
#18035 = CARTESIAN_POINT ( 'NONE',  ( 12.09999999999990550, 12.50000000000000000, 4.330127018922196314 ) ) ;
#18036 = DIRECTION ( 'NONE',  ( 0.000000000000000000, 1.000000000000000000, 0.000000000000000000 ) ) ;
#18037 = LINE ( 'NONE', #39016, #88799 ) ;
#18038 = DIRECTION ( 'NONE',  ( 0.000000000000000000, 1.000000000000000000, 0.000000000000000000 ) ) ;
#18040 = ORIENTED_EDGE ( 'NONE', *, *, #62154, .F. ) ;
#18039 = CIRCLE ( 'NONE', #107936, 0.06509327318403745899 ) ;
#18041 = CARTESIAN_POINT ( 'NONE',  ( 11.89999999999990443, 12.50000000000000000, -0.3464101615137782364 ) ) ;
#18042 = ORIENTED_EDGE ( 'NONE', *, *, #29335, .T. ) ;
#18043 = VECTOR ( 'NONE', #64462, 1000.000000000000000 ) ;
#18044 = ORIENTED_EDGE ( 'NONE', *, *, #74204, .F. ) ;
#18045 = ORIENTED_EDGE ( 'NONE', *, *, #1695, .T. ) ;
#18046 = DIRECTION ( 'NONE',  ( 0.000000000000000000, 0.000000000000000000, 1.000000000000000000 ) ) ;
#18047 = LINE ( 'NONE', #77612, #8684 ) ;
#18048 = CONICAL_SURFACE ( 'NONE', #7584, 0.09999999999999982514, 0.003490658503988666988 ) ;
#18049 = DIRECTION ( 'NONE',  ( 0.000000000000000000, 0.000000000000000000, -1.000000000000000000 ) ) ;
#18050 = ORIENTED_EDGE ( 'NONE', *, *, #39063, .T. ) ;
#18051 = DIRECTION ( 'NONE',  ( 0.000000000000000000, 1.000000000000000000, 0.000000000000000000 ) ) ;
#18052 = CIRCLE ( 'NONE', #64034, 0.06509327318403745899 ) ;
#18053 = CIRCLE ( 'NONE', #126739, 0.06509327318403745899 ) ;
#18054 = DIRECTION ( 'NONE',  ( 0.000000000000000000, 0.000000000000000000, 1.000000000000000000 ) ) ;
#18055 = CIRCLE ( 'NONE', #103754, 0.1000000000000002554 ) ;
#18056 = EDGE_CURVE ( 'NONE', #26032, #103454, #96572, .T. ) ;
#18057 = FACE_OUTER_BOUND ( 'NONE', #68249, .T. ) ;
#18058 = CARTESIAN_POINT ( 'NONE',  ( 183.9010416670080588, -4.367472073101519747, 7.564683531249999149 ) ) ;
#18059 = CARTESIAN_POINT ( 'NONE',  ( 8.149999999999920419, 2.500000000000000000, 6.841600689897072485 ) ) ;
#18060 = FACE_OUTER_BOUND ( 'NONE', #13795, .T. ) ;
#18061 = DIRECTION ( 'NONE',  ( 0.000000000000000000, 1.000000000000000000, 0.000000000000000000 ) ) ;
#18062 = ORIENTED_EDGE ( 'NONE', *, *, #77491, .T. ) ;
#18063 = CARTESIAN_POINT ( 'NONE',  ( -12.29999999999999716, 12.50000000000000000, 0.3464101615137776813 ) ) ;
#18064 = AXIS2_PLACEMENT_3D ( 'NONE', #84009, #54540, #94471 ) ;
#18065 = ADVANCED_FACE ( 'NONE', ( #74211 ), #125824, .T. ) ;
#18066 = ORIENTED_EDGE ( 'NONE', *, *, #23690, .F. ) ;
#18067 = CIRCLE ( 'NONE', #47329, 0.1000000000000002554 ) ;
#18068 = ORIENTED_EDGE ( 'NONE', *, *, #52846, .T. ) ;
#18069 = DIRECTION ( 'NONE',  ( 0.000000000000000000, -0.000000000000000000, 1.000000000000000000 ) ) ;
#18070 = ADVANCED_FACE ( 'NONE', ( #14616 ), #68083, .T. ) ;
#18071 = DIRECTION ( 'NONE',  ( -0.000000000000000000, -1.000000000000000000, -0.000000000000000000 ) ) ;
#18073 = EDGE_CURVE ( 'NONE', #94129, #104091, #87075, .T. ) ;
#18072 = FACE_OUTER_BOUND ( 'NONE', #77690, .T. ) ;
#18074 = EDGE_CURVE ( 'NONE', #56898, #68530, #46409, .T. ) ;
#18075 = EDGE_CURVE ( 'NONE', #106661, #105096, #29699, .T. ) ;
#18076 = ORIENTED_EDGE ( 'NONE', *, *, #29086, .F. ) ;
#18077 = EDGE_LOOP ( 'NONE', ( #30878, #19277, #47662, #3904 ) ) ;
#18078 = CARTESIAN_POINT ( 'NONE',  ( 0.3999999999999628852, 12.50000000000000000, -0.7579135962115894909 ) ) ;
#18079 = DIRECTION ( 'NONE',  ( 0.000000000000000000, 1.000000000000000000, 0.000000000000000000 ) ) ;
#18080 = EDGE_CURVE ( 'NONE', #116825, #5168, #48577, .T. ) ;
#18081 = DIRECTION ( 'NONE',  ( 0.000000000000000000, 1.000000000000000000, 0.000000000000000000 ) ) ;
#18082 = ORIENTED_EDGE ( 'NONE', *, *, #42088, .F. ) ;
#18083 = VERTEX_POINT ( 'NONE', #86434 ) ;
#18084 = ADVANCED_FACE ( 'NONE', ( #108011 ), #92376, .T. ) ;
#18085 = DIRECTION ( 'NONE',  ( 0.000000000000000000, 1.000000000000000000, 0.000000000000000000 ) ) ;
#18086 = EDGE_CURVE ( 'NONE', #102089, #54506, #94534, .T. ) ;
#18087 = ORIENTED_EDGE ( 'NONE', *, *, #125847, .F. ) ;
#18088 = CARTESIAN_POINT ( 'NONE',  ( 9.549999999999918998, 2.500000000000000000, 2.165063509461097713 ) ) ;
#18089 = EDGE_CURVE ( 'NONE', #17389, #19145, #27496, .T. ) ;
#18090 = ADVANCED_FACE ( 'NONE', ( #17690 ), #19211, .T. ) ;
#18091 = CARTESIAN_POINT ( 'NONE',  ( -0.8500000000000382805, 2.500000000000000000, -2.757883832488654097 ) ) ;
#18092 = VERTEX_POINT ( 'NONE', #128979 ) ;
#18093 = CARTESIAN_POINT ( 'NONE',  ( -2.100000000000034284, 2.500000000000000000, -4.430127018922202176 ) ) ;
#18094 = DIRECTION ( 'NONE',  ( 0.000000000000000000, 0.000000000000000000, 1.000000000000000000 ) ) ;
#18095 = DIRECTION ( 'NONE',  ( 0.000000000000000000, 0.000000000000000000, 1.000000000000000000 ) ) ;
#18097 = EDGE_CURVE ( 'NONE', #41716, #91777, #102834, .T. ) ;
#18096 = DIRECTION ( 'NONE',  ( -4.274815082592931898E-19, -0.9999939076577903929, -0.003490651415223739937 ) ) ;
#18098 = VERTEX_POINT ( 'NONE', #38660 ) ;
#18099 = CARTESIAN_POINT ( 'NONE',  ( 17.50000000000000000, -2.500000000000000000, 4.000000000000001776 ) ) ;
#18100 = CONICAL_SURFACE ( 'NONE', #13892, 0.1000000000000002554, 0.003490658503988666988 ) ;
#18101 = CONICAL_SURFACE ( 'NONE', #26436, 0.1000000000000000472, 0.003490658503988666988 ) ;
#18102 = EDGE_LOOP ( 'NONE', ( #49197, #81196 ) ) ;
#18103 = VERTEX_POINT ( 'NONE', #58921 ) ;
#18104 = CARTESIAN_POINT ( 'NONE',  ( 4.799999999999935874, 2.500000000000000000, 3.983716857408420964 ) ) ;
#18105 = CARTESIAN_POINT ( 'NONE',  ( 0.6499999999999566125, 2.500000000000000000, -6.248780366869526759 ) ) ;
#18106 = CARTESIAN_POINT ( 'NONE',  ( -8.550000000000013145, 2.500000000000000000, 2.511473670974873507 ) ) ;
#18107 = CARTESIAN_POINT ( 'NONE',  ( -6.050000000000018474, 2.500000000000000000, 2.611473670974873151 ) ) ;
#18108 = CARTESIAN_POINT ( 'NONE',  ( 14.34999999999989306, 12.50000000000000000, -2.511473670974877948 ) ) ;
#18111 = CIRCLE ( 'NONE', #53626, 0.1000000000000002554 ) ;
#18110 = DIRECTION ( 'NONE',  ( 0.000000000000000000, 0.000000000000000000, 1.000000000000000000 ) ) ;
#18109 = CONICAL_SURFACE ( 'NONE', #28591, 0.1000000000000002554, 0.003490658503988666988 ) ;
#18112 = CARTESIAN_POINT ( 'NONE',  ( -7.100000000000017408, 12.50000000000000000, -3.702399969078687292 ) ) ;
#18113 = DIRECTION ( 'NONE',  ( 0.000000000000000000, 0.000000000000000000, -1.000000000000000000 ) ) ;
#18114 = DIRECTION ( 'NONE',  ( 0.000000000000000000, 0.000000000000000000, -1.000000000000000000 ) ) ;
#18115 = CARTESIAN_POINT ( 'NONE',  ( -11.04999999999999893, 2.500000000000000000, 6.148780366869520009 ) ) ;
#18117 = AXIS2_PLACEMENT_3D ( 'NONE', #35415, #115893, #96243 ) ;
#18116 = AXIS2_PLACEMENT_3D ( 'NONE', #81247, #10546, #30871 ) ;
#18118 = CONICAL_SURFACE ( 'NONE', #36925, 0.09999999999999999167, 0.003490658503988666988 ) ;
#18119 = ORIENTED_EDGE ( 'NONE', *, *, #34591, .F. ) ;
#18120 = DIRECTION ( 'NONE',  ( 0.000000000000000000, 0.000000000000000000, 1.000000000000000000 ) ) ;
#18121 = CARTESIAN_POINT ( 'NONE',  ( -1.250000000000036193, 12.50000000000000000, 5.867463478539781896 ) ) ;
#18122 = DIRECTION ( 'NONE',  ( 0.000000000000000000, 0.000000000000000000, -1.000000000000000000 ) ) ;
#18123 = CARTESIAN_POINT ( 'NONE',  ( 4.149999999999938183, 2.500000000000000000, 5.802370205355744659 ) ) ;
#18124 = LINE ( 'NONE', #118911, #1979 ) ;
#18125 = ORIENTED_EDGE ( 'NONE', *, *, #48102, .T. ) ;
#18126 = CARTESIAN_POINT ( 'NONE',  ( -10.20000000000000462, 2.500000000000000000, 0.3464101615137735735 ) ) ;
#18127 = EDGE_CURVE ( 'NONE', #17235, #101758, #40172, .T. ) ;
#18128 = EDGE_CURVE ( 'NONE', #14173, #63919, #109090, .T. ) ;
#18129 = CARTESIAN_POINT ( 'NONE',  ( 13.29999999999989946, 2.500000000000000000, -2.385244779468109755E-15 ) ) ;
#18131 = ORIENTED_EDGE ( 'NONE', *, *, #129246, .T. ) ;
#18130 = CARTESIAN_POINT ( 'NONE',  ( -3.749999999999991118, 12.50000000000000000, 2.165063509461097713 ) ) ;
#18132 = AXIS2_PLACEMENT_3D ( 'NONE', #105148, #84872, #115609 ) ;
#18133 = AXIS2_PLACEMENT_3D ( 'NONE', #77307, #107411, #45931 ) ;
#18134 = ORIENTED_EDGE ( 'NONE', *, *, #110149, .F. ) ;
#18135 = CIRCLE ( 'NONE', #87090, 0.06509327318403745899 ) ;
#18136 = ADVANCED_FACE ( 'NONE', ( #110592 ), #40604, .T. ) ;
#18137 = DIRECTION ( 'NONE',  ( 0.000000000000000000, 1.000000000000000000, 0.000000000000000000 ) ) ;
#18138 = CIRCLE ( 'NONE', #95424, 0.09999999999999982514 ) ;
#18139 = ORIENTED_EDGE ( 'NONE', *, *, #123478, .T. ) ;
#18140 = ORIENTED_EDGE ( 'NONE', *, *, #78684, .T. ) ;
#18141 = VERTEX_POINT ( 'NONE', #60234 ) ;
#18142 = PLANE ( 'NONE',  #76161 ) ;
#18143 = CIRCLE ( 'NONE', #93374, 0.09999999999999982514 ) ;
#18144 = DIRECTION ( 'NONE',  ( -4.274815082592931898E-19, -0.9999939076577903929, -0.003490651415223739937 ) ) ;
#18145 = CARTESIAN_POINT ( 'NONE',  ( -6.517459502904499961E-15, 2.500000000000000000, 4.230127018922196669 ) ) ;
#18146 = AXIS2_PLACEMENT_3D ( 'NONE', #58780, #60718, #39802 ) ;
#18147 = DIRECTION ( 'NONE',  ( -0.000000000000000000, -1.000000000000000000, -0.000000000000000000 ) ) ;
#18148 = VERTEX_POINT ( 'NONE', #78580 ) ;
#18149 = FACE_OUTER_BOUND ( 'NONE', #5077, .T. ) ;
#18150 = ORIENTED_EDGE ( 'NONE', *, *, #35367, .F. ) ;
#18151 = CARTESIAN_POINT ( 'NONE',  ( -4.999999999999986677, 2.500000000000000000, 4.330127018922196314 ) ) ;
#18152 = DIRECTION ( 'NONE',  ( -0.000000000000000000, -1.000000000000000000, -0.000000000000000000 ) ) ;
#18153 = CARTESIAN_POINT ( 'NONE',  ( 20.80581321129286820, 0.6997403544445329748, 4.161084241360442526 ) ) ;
#18154 = CYLINDRICAL_SURFACE ( 'NONE', #58923, 7.699999999999999289 ) ;
#18155 = AXIS2_PLACEMENT_3D ( 'NONE', #75861, #73942, #105337 ) ;
#18156 = LINE ( 'NONE', #88835, #78898 ) ;
#18157 = AXIS2_PLACEMENT_3D ( 'NONE', #2069, #99647, #9972 ) ;
#18158 = EDGE_LOOP ( 'NONE', ( #43913, #31774 ) ) ;
#18160 = CONICAL_SURFACE ( 'NONE', #34920, 0.09999999999999982514, 0.003490658503988666988 ) ;
#18159 = AXIS2_PLACEMENT_3D ( 'NONE', #29218, #118221, #39052 ) ;
#18161 = ORIENTED_EDGE ( 'NONE', *, *, #14099, .T. ) ;
#18162 = VERTEX_POINT ( 'NONE', #70035 ) ;
#18163 = ORIENTED_EDGE ( 'NONE', *, *, #1237, .F. ) ;
#18164 = VERTEX_POINT ( 'NONE', #79217 ) ;
#18165 = CARTESIAN_POINT ( 'NONE',  ( 1.449999999999951328, 12.50000000000000000, -1.753560074763288679 ) ) ;
#18166 = DIRECTION ( 'NONE',  ( -4.274815082592931898E-19, -0.9999939076577903929, -0.003490651415223739937 ) ) ;
#18167 = DIRECTION ( 'NONE',  ( -0.000000000000000000, -1.000000000000000000, -0.000000000000000000 ) ) ;
#18168 = FACE_BOUND ( 'NONE', #26367, .T. ) ;
#18169 = CARTESIAN_POINT ( 'NONE',  ( -7.900000000000011013, 12.50000000000000000, 4.330127018922196314 ) ) ;
#18170 = CARTESIAN_POINT ( 'NONE',  ( 187.0312500006828031, 9.429780353434619030E-16, -7.700000000000000178 ) ) ;
#18171 = CARTESIAN_POINT ( 'NONE',  ( 12.49999999999990230, 2.500000000000000000, -0.5928203230275541635 ) ) ;
#18172 = DIRECTION ( 'NONE',  ( -0.000000000000000000, -1.000000000000000000, -0.000000000000000000 ) ) ;
#18173 = EDGE_CURVE ( 'NONE', #73698, #2826, #89029, .T. ) ;
#18174 = LINE ( 'NONE', #88181, #8669 ) ;
#18175 = CARTESIAN_POINT ( 'NONE',  ( -11.69999999999999574, 2.500000000000000000, 4.330127018922196314 ) ) ;
#18176 = AXIS2_PLACEMENT_3D ( 'NONE', #103236, #44968, #52842 ) ;
#18177 = CARTESIAN_POINT ( 'NONE',  ( -12.29999999999999361, 12.50000000000000000, 3.918623584224382839 ) ) ;
#18178 = DIRECTION ( 'NONE',  ( 0.000000000000000000, 0.000000000000000000, 1.000000000000000000 ) ) ;
#18179 = VERTEX_POINT ( 'NONE', #31407 ) ;
#18180 = ORIENTED_EDGE ( 'NONE', *, *, #13810, .F. ) ;
#18181 = VERTEX_POINT ( 'NONE', #71306 ) ;
#18182 = ORIENTED_EDGE ( 'NONE', *, *, #83808, .T. ) ;
#18183 = ADVANCED_FACE ( 'NONE', ( #90960 ), #73600, .T. ) ;
#18184 = CARTESIAN_POINT ( 'NONE',  ( -12.29999999999999538, 2.500000000000000000, -0.3464101615137741841 ) ) ;
#18185 = ADVANCED_FACE ( 'NONE', ( #30772 ), #50621, .T. ) ;
#18186 = FACE_BOUND ( 'NONE', #54726, .T. ) ;
#18187 = DIRECTION ( 'NONE',  ( 0.000000000000000000, 0.000000000000000000, 1.000000000000000000 ) ) ;
#18188 = AXIS2_PLACEMENT_3D ( 'NONE', #81034, #90843, #9709 ) ;
#18189 = VECTOR ( 'NONE', #103953, 1000.000000000000000 ) ;
#18190 = ORIENTED_EDGE ( 'NONE', *, *, #31431, .F. ) ;
#18191 = CARTESIAN_POINT ( 'NONE',  ( 12.49999999999990408, 2.500000000000000000, -3.637306695894650055 ) ) ;
#18192 = EDGE_CURVE ( 'NONE', #49438, #39786, #123762, .T. ) ;
#18193 = DIRECTION ( 'NONE',  ( 0.000000000000000000, 0.000000000000000000, 1.000000000000000000 ) ) ;
#18194 = DIRECTION ( 'NONE',  ( -0.000000000000000000, 1.000000000000000000, -0.000000000000000000 ) ) ;
#18195 = ORIENTED_EDGE ( 'NONE', *, *, #28914, .T. ) ;
#18196 = DIRECTION ( 'NONE',  ( 0.000000000000000000, 0.000000000000000000, 1.000000000000000000 ) ) ;
#18197 = CARTESIAN_POINT ( 'NONE',  ( -8.749999999999975131, 2.500000000000000000, -2.165063509461101710 ) ) ;
#18198 = CONICAL_SURFACE ( 'NONE', #47457, 0.09999999999999982514, 0.003490658503988666988 ) ;
#18199 = VERTEX_POINT ( 'NONE', #119770 ) ;
#18200 = VERTEX_POINT ( 'NONE', #99500 ) ;
#18201 = FACE_OUTER_BOUND ( 'NONE', #37724, .T. ) ;
#18202 = LINE ( 'NONE', #99364, #87312 ) ;
#18204 = AXIS2_PLACEMENT_3D ( 'NONE', #37828, #77112, #56165 ) ;
#18203 = CONICAL_SURFACE ( 'NONE', #108095, 0.09999999999999982514, 0.003490658503988666988 ) ;
#18205 = CIRCLE ( 'NONE', #70454, 0.06509327318403745899 ) ;
#18206 = FACE_OUTER_BOUND ( 'NONE', #55944, .T. ) ;
#18207 = CARTESIAN_POINT ( 'NONE',  ( -3.950000000000025491, 2.500000000000000000, 6.148780366869520897 ) ) ;
#18208 = ORIENTED_EDGE ( 'NONE', *, *, #100951, .T. ) ;
#18209 = CARTESIAN_POINT ( 'NONE',  ( -5.850000000000021849, 12.50000000000000000, -7.188010851410854052 ) ) ;
#18210 = ORIENTED_EDGE ( 'NONE', *, *, #77205, .T. ) ;
#18211 = ORIENTED_EDGE ( 'NONE', *, *, #106865, .T. ) ;
#18212 = PLANE ( 'NONE',  #82831 ) ;
#18213 = ORIENTED_EDGE ( 'NONE', *, *, #16417, .T. ) ;
#18214 = FACE_OUTER_BOUND ( 'NONE', #65451, .T. ) ;
#18215 = FACE_BOUND ( 'NONE', #1387, .T. ) ;
#18216 = EDGE_CURVE ( 'NONE', #107817, #73591, #67314, .T. ) ;
#18217 = VERTEX_POINT ( 'NONE', #90287 ) ;
#18218 = DIRECTION ( 'NONE',  ( 0.000000000000000000, 0.000000000000000000, 1.000000000000000000 ) ) ;
#18219 = EDGE_LOOP ( 'NONE', ( #82439, #99029, #12563, #69681 ) ) ;
#18220 = CYLINDRICAL_SURFACE ( 'NONE', #10666, 4.000000000000000000 ) ;
#18221 = DIRECTION ( 'NONE',  ( 0.000000000000000000, 0.000000000000000000, -1.000000000000000000 ) ) ;
#18222 = CARTESIAN_POINT ( 'NONE',  ( -4.600000000000028955, 12.50000000000000000, -4.330127018922201643 ) ) ;
#18224 = EDGE_CURVE ( 'NONE', #55568, #29710, #10882, .T. ) ;
#18223 = DIRECTION ( 'NONE',  ( 0.000000000000000000, 0.000000000000000000, -1.000000000000000000 ) ) ;
#18225 = EDGE_CURVE ( 'NONE', #63575, #17352, #71549, .T. ) ;
#18227 = VECTOR ( 'NONE', #672, 1000.000000000000000 ) ;
#18226 = CARTESIAN_POINT ( 'NONE',  ( -3.750000000000027978, 2.500000000000000000, 7.188010851410848723 ) ) ;
#18228 = EDGE_CURVE ( 'NONE', #100677, #17818, #119561, .T. ) ;
#18229 = ORIENTED_EDGE ( 'NONE', *, *, #68139, .T. ) ;
#18230 = CONICAL_SURFACE ( 'NONE', #95515, 0.09999999999999982514, 0.003490658503988666988 ) ;
#18231 = VERTEX_POINT ( 'NONE', #1282 ) ;
#18232 = ORIENTED_EDGE ( 'NONE', *, *, #97775, .T. ) ;
#18233 = CARTESIAN_POINT ( 'NONE',  ( -3.350000000000028955, 12.50000000000000000, 5.802370205355744659 ) ) ;
#18234 = CIRCLE ( 'NONE', #105979, 1.000000000000000888 ) ;
#18235 = LINE ( 'NONE', #70561, #41090 ) ;
#18236 = EDGE_CURVE ( 'NONE', #99110, #16061, #109302, .T. ) ;
#18237 = CARTESIAN_POINT ( 'NONE',  ( -5.800000000000018474, 2.500000000000000000, -2.276824562219559311E-15 ) ) ;
#18239 = VERTEX_POINT ( 'NONE', #79840 ) ;
#18238 = VERTEX_POINT ( 'NONE', #41234 ) ;
#18240 = ADVANCED_FACE ( 'NONE', ( #50385 ), #15081, .T. ) ;
#18241 = ORIENTED_EDGE ( 'NONE', *, *, #99401, .F. ) ;
#18242 = EDGE_CURVE ( 'NONE', #118223, #2269, #88255, .T. ) ;
#18243 = CARTESIAN_POINT ( 'NONE',  ( -12.04999999999999716, 2.500000000000000000, -6.395190528383298378 ) ) ;
#18244 = CIRCLE ( 'NONE', #49565, 0.1000000000000002554 ) ;
#18245 = DIRECTION ( 'NONE',  ( 0.000000000000000000, 0.000000000000000000, 1.000000000000000000 ) ) ;
#18246 = CIRCLE ( 'NONE', #129097, 0.06509327318403745899 ) ;
#18247 = ADVANCED_FACE ( 'NONE', ( #22878 ), #124292, .T. ) ;
#18248 = DIRECTION ( 'NONE',  ( -0.000000000000000000, -1.000000000000000000, -0.000000000000000000 ) ) ;
#18249 = FACE_OUTER_BOUND ( 'NONE', #25815, .T. ) ;
#18250 = FACE_OUTER_BOUND ( 'NONE', #71532, .T. ) ;
#18251 = DIRECTION ( 'NONE',  ( 0.000000000000000000, -0.9999939076577903929, 0.003490651415223739937 ) ) ;
#18252 = DIRECTION ( 'NONE',  ( 0.000000000000000000, 0.000000000000000000, 1.000000000000000000 ) ) ;
#18253 = AXIS2_PLACEMENT_3D ( 'NONE', #72512, #519, #73146 ) ;
#18254 = EDGE_CURVE ( 'NONE', #113689, #117544, #63431, .T. ) ;
#18256 = EDGE_CURVE ( 'NONE', #10201, #90888, #41873, .T. ) ;
#18255 = CARTESIAN_POINT ( 'NONE',  ( -11.05000000000000071, 2.500000000000000000, 2.411473670974873862 ) ) ;
#18257 = VERTEX_POINT ( 'NONE', #102071 ) ;
#18258 = ORIENTED_EDGE ( 'NONE', *, *, #63108, .T. ) ;
#18259 = CARTESIAN_POINT ( 'NONE',  ( 11.44999999999990870, 12.50000000000000000, 6.841600689897072485 ) ) ;
#18261 = AXIS2_PLACEMENT_3D ( 'NONE', #26910, #107398, #127680 ) ;
#18260 = AXIS2_PLACEMENT_3D ( 'NONE', #48052, #79448, #87941 ) ;
#18262 = DIRECTION ( 'NONE',  ( -0.000000000000000000, 1.000000000000000000, -0.000000000000000000 ) ) ;
#18263 = ORIENTED_EDGE ( 'NONE', *, *, #66578, .T. ) ;
#18264 = ORIENTED_EDGE ( 'NONE', *, *, #44062, .F. ) ;
#18265 = DIRECTION ( 'NONE',  ( 0.000000000000000000, 0.000000000000000000, 1.000000000000000000 ) ) ;
#18266 = LINE ( 'NONE', #8433, #3006 ) ;
#18267 = CARTESIAN_POINT ( 'NONE',  ( 2.500000000000002220, 2.500000000000000000, -8.999999999999998224 ) ) ;
#18268 = CARTESIAN_POINT ( 'NONE',  ( 2.949999999999946887, 2.500000000000000000, -2.165063509461101710 ) ) ;
#18269 = CARTESIAN_POINT ( 'NONE',  ( 9.999999999999948486, 2.500000000000000000, 4.230127018922196669 ) ) ;
#18270 = CARTESIAN_POINT ( 'NONE',  ( 1.849999999999950573, 2.500000000000000000, -1.918653347947326004 ) ) ;
#18271 = LINE ( 'NONE', #88277, #94952 ) ;
#18272 = ORIENTED_EDGE ( 'NONE', *, *, #8320, .F. ) ;
#18273 = DIRECTION ( 'NONE',  ( -4.274815082592931898E-19, -0.9999939076577903929, -0.003490651415223739937 ) ) ;
#18274 = CARTESIAN_POINT ( 'NONE',  ( -8.350000000000013856, 12.50000000000000000, 2.165063509461097713 ) ) ;
#18275 = UNCERTAINTY_MEASURE_WITH_UNIT (LENGTH_MEASURE( 1.000000000000000082E-05 ), #98248, 'distance_accuracy_value', 'NONE');
#18276 = EDGE_LOOP ( 'NONE', ( #17802, #46649 ) ) ;
#18277 = ORIENTED_EDGE ( 'NONE', *, *, #127724, .F. ) ;
#18278 = ORIENTED_EDGE ( 'NONE', *, *, #62154, .T. ) ;
#18279 = ORIENTED_EDGE ( 'NONE', *, *, #27682, .T. ) ;
#18280 = DIRECTION ( 'NONE',  ( 0.000000000000000000, 0.000000000000000000, 1.000000000000000000 ) ) ;
#18281 = CARTESIAN_POINT ( 'NONE',  ( -4.999999999999986677, 12.50000000000000000, 4.395220292106234439 ) ) ;
#18282 = ORIENTED_EDGE ( 'NONE', *, *, #71655, .T. ) ;
#18283 = AXIS2_PLACEMENT_3D ( 'NONE', #110808, #101650, #12600 ) ;
#18284 = CARTESIAN_POINT ( 'NONE',  ( 4.999999999999973355, 2.500000000000000000, -4.330127018922201643 ) ) ;
#18285 = ADVANCED_FACE ( 'NONE', ( #71978 ), #101426, .T. ) ;
#18287 = CARTESIAN_POINT ( 'NONE',  ( -0.8000000000000315747, 2.500000000000000000, -0.1000000000000000056 ) ) ;
#18286 = CONICAL_SURFACE ( 'NONE', #26611, 0.1000000000000002554, 0.003490658503988666988 ) ;
#18288 = EDGE_CURVE ( 'NONE', #70042, #49008, #44429, .T. ) ;
#18289 = CARTESIAN_POINT ( 'NONE',  ( -11.44999999999999929, 12.50000000000000000, -6.213873640053560798 ) ) ;
#18291 = ORIENTED_EDGE ( 'NONE', *, *, #23658, .T. ) ;
#18290 = CYLINDRICAL_SURFACE ( 'NONE', #5667, 2.000000000000000000 ) ;
#18292 = CARTESIAN_POINT ( 'NONE',  ( 4.399999999999937295, 2.500000000000000000, 3.883716857408421319 ) ) ;
#18294 = CIRCLE ( 'NONE', #47558, 0.06509327318403745899 ) ;
#18293 = AXIS2_PLACEMENT_3D ( 'NONE', #74507, #94143, #81736 ) ;
#18295 = LINE ( 'NONE', #48405, #127325 ) ;
#18296 = VERTEX_POINT ( 'NONE', #33974 ) ;
#18297 = AXIS2_PLACEMENT_3D ( 'NONE', #35486, #5994, #114668 ) ;
#18298 = ORIENTED_EDGE ( 'NONE', *, *, #92546, .T. ) ;
#18299 = ORIENTED_EDGE ( 'NONE', *, *, #111934, .F. ) ;
#18300 = DIRECTION ( 'NONE',  ( -0.000000000000000000, -1.000000000000000000, -0.000000000000000000 ) ) ;
#18301 = VECTOR ( 'NONE', #63861, 1000.000000000000000 ) ;
#18302 = DIRECTION ( 'NONE',  ( -0.000000000000000000, -1.000000000000000000, -0.000000000000000000 ) ) ;
#18303 = VECTOR ( 'NONE', #30306, 1000.000000000000000 ) ;
#18304 = ORIENTED_EDGE ( 'NONE', *, *, #3179, .T. ) ;
#18305 = FACE_OUTER_BOUND ( 'NONE', #116311, .T. ) ;
#18306 = DIRECTION ( 'NONE',  ( 0.000000000000000000, 1.000000000000000000, 0.000000000000000000 ) ) ;
#18307 = LINE ( 'NONE', #49732, #73449 ) ;
#18308 = FACE_OUTER_BOUND ( 'NONE', #94748, .T. ) ;
#18309 = ORIENTED_EDGE ( 'NONE', *, *, #39436, .T. ) ;
#18310 = CONICAL_SURFACE ( 'NONE', #58046, 0.1000000000000002554, 0.003490658503988666988 ) ;
#18311 = CARTESIAN_POINT ( 'NONE',  ( -5.850000000000018296, 2.500000000000000000, 7.088010851410848190 ) ) ;
#18312 = VECTOR ( 'NONE', #39523, 1000.000000000000000 ) ;
#18313 = ORIENTED_EDGE ( 'NONE', *, *, #81965, .T. ) ;
#18314 = ORIENTED_EDGE ( 'NONE', *, *, #48811, .F. ) ;
#18315 = DIRECTION ( 'NONE',  ( 0.000000000000000000, 0.000000000000000000, -1.000000000000000000 ) ) ;
#18316 = CARTESIAN_POINT ( 'NONE',  ( 12.69999999999990337, 12.50000000000000000, 3.918623584224382839 ) ) ;
#18317 = FACE_BOUND ( 'NONE', #109209, .T. ) ;
#18318 = AXIS2_PLACEMENT_3D ( 'NONE', #114192, #44155, #121574 ) ;
#18319 = CARTESIAN_POINT ( 'NONE',  ( 127.5000000000000000, -1.500000000000000000, 6.000000000000000000 ) ) ;
#18320 = CARTESIAN_POINT ( 'NONE',  ( -9.150000000000005684, 2.500000000000000000, 7.288010851410849256 ) ) ;
#18321 = CONICAL_SURFACE ( 'NONE', #72628, 0.1000000000000002554, 0.003490658503988666988 ) ;
#18322 = DIRECTION ( 'NONE',  ( -0.000000000000000000, -1.000000000000000000, -0.000000000000000000 ) ) ;
#18323 = ADVANCED_FACE ( 'NONE', ( #53615 ), #109194, .T. ) ;
#18324 = CONICAL_SURFACE ( 'NONE', #64302, 0.1000000000000002554, 0.003490658503988666988 ) ;
#18325 = EDGE_LOOP ( 'NONE', ( #97508, #90310, #95408, #74436 ) ) ;
#18326 = CARTESIAN_POINT ( 'NONE',  ( 13.34999999999989662, 12.50000000000000000, -2.165063509461101710 ) ) ;
#18327 = DIRECTION ( 'NONE',  ( -0.000000000000000000, -1.000000000000000000, -0.000000000000000000 ) ) ;
#18329 = CARTESIAN_POINT ( 'NONE',  ( 3.549999999999942091, 2.500000000000000000, 2.611473670974873151 ) ) ;
#18328 = AXIS2_PLACEMENT_3D ( 'NONE', #107571, #17218, #86631 ) ;
#18331 = CARTESIAN_POINT ( 'NONE',  ( 12.49999999999990585, 2.500000000000000000, 3.637306695894644726 ) ) ;
#18330 = VECTOR ( 'NONE', #41589, 1000.000000000000000 ) ;
#18332 = ORIENTED_EDGE ( 'NONE', *, *, #75975, .F. ) ;
#18333 = EDGE_CURVE ( 'NONE', #113637, #4728, #44453, .T. ) ;
#18334 = PLANE ( 'NONE',  #46882 ) ;
#18335 = CIRCLE ( 'NONE', #62272, 0.1000000000000002554 ) ;
#18336 = CARTESIAN_POINT ( 'NONE',  ( 5.849999999999933031, 2.500000000000000000, -1.472243186433550122 ) ) ;
#18337 = VERTEX_POINT ( 'NONE', #12388 ) ;
#18338 = ORIENTED_EDGE ( 'NONE', *, *, #36366, .T. ) ;
#18339 = EDGE_CURVE ( 'NONE', #109623, #97511, #71644, .T. ) ;
#18340 = DIRECTION ( 'NONE',  ( 0.000000000000000000, 1.000000000000000000, 0.000000000000000000 ) ) ;
#18341 = AXIS2_PLACEMENT_3D ( 'NONE', #77636, #46916, #86821 ) ;
#18343 = EDGE_CURVE ( 'NONE', #91438, #1733, #121811, .T. ) ;
#18342 = DIRECTION ( 'NONE',  ( -0.000000000000000000, -1.000000000000000000, -0.000000000000000000 ) ) ;
#18344 = FACE_BOUND ( 'NONE', #116469, .T. ) ;
#18345 = DIRECTION ( 'NONE',  ( -0.000000000000000000, 1.000000000000000000, -0.000000000000000000 ) ) ;
#18347 = CIRCLE ( 'NONE', #30896, 0.06509327318403743123 ) ;
#18346 = VECTOR ( 'NONE', #112773, 1000.000000000000000 ) ;
#18348 = ORIENTED_EDGE ( 'NONE', *, *, #106890, .F. ) ;
#18349 = DIRECTION ( 'NONE',  ( 0.000000000000000000, -0.9999939076577903929, 0.003490651415223739937 ) ) ;
#18350 = ADVANCED_FACE ( 'NONE', ( #22234 ), #84147, .T. ) ;
#18351 = VERTEX_POINT ( 'NONE', #122364 ) ;
#18352 = EDGE_LOOP ( 'NONE', ( #2743, #71828, #43374, #21440 ) ) ;
#18353 = DIRECTION ( 'NONE',  ( -0.000000000000000000, -1.000000000000000000, -0.000000000000000000 ) ) ;
#18354 = ADVANCED_FACE ( 'NONE', ( #72614 ), #83724, .T. ) ;
#18355 = CARTESIAN_POINT ( 'NONE',  ( 186.4583333333333144, 4.445597072760117285, 7.699999999999999289 ) ) ;
#18356 = EDGE_LOOP ( 'NONE', ( #43369, #15357 ) ) ;
#18357 = DIRECTION ( 'NONE',  ( 0.000000000000000000, 1.000000000000000000, 0.000000000000000000 ) ) ;
#18358 = DIRECTION ( 'NONE',  ( -0.000000000000000000, 1.000000000000000000, -0.000000000000000000 ) ) ;
#18359 = DIRECTION ( 'NONE',  ( 0.000000000000000000, 1.000000000000000000, 0.000000000000000000 ) ) ;
#18360 = DIRECTION ( 'NONE',  ( 0.000000000000000000, 0.000000000000000000, -1.000000000000000000 ) ) ;
#18361 = EDGE_LOOP ( 'NONE', ( #30333, #105550, #57019, #45940 ) ) ;
#18362 =( LENGTH_UNIT ( ) NAMED_UNIT ( * ) SI_UNIT ( .MILLI., .METRE. ) );
#18363 = CARTESIAN_POINT ( 'NONE',  ( 0.3999999999999555023, 12.50000000000000000, 4.265033745738159077 ) ) ;
#18364 = CARTESIAN_POINT ( 'NONE',  ( -2.950000000000033484, 2.500000000000000000, -6.395190528383301931 ) ) ;
#18365 = FACE_OUTER_BOUND ( 'NONE', #2741, .T. ) ;
#18366 = EDGE_LOOP ( 'NONE', ( #28978, #91898 ) ) ;
#18367 = CONICAL_SURFACE ( 'NONE', #7991, 0.1000000000000002554, 0.003490658503988666988 ) ;
#18368 = FACE_OUTER_BOUND ( 'NONE', #109675, .T. ) ;
#18369 = ORIENTED_EDGE ( 'NONE', *, *, #65350, .T. ) ;
#18370 = CARTESIAN_POINT ( 'NONE',  ( -13.29999999999999005, 12.50000000000000000, 1.843143693225357538E-15 ) ) ;
#18371 = EDGE_LOOP ( 'NONE', ( #24524, #56209, #102658, #96120 ) ) ;
#18372 = CARTESIAN_POINT ( 'NONE',  ( 7.499999999999961808, 2.500000000000000000, 4.330127018922196314 ) ) ;
#18373 = CARTESIAN_POINT ( 'NONE',  ( 87.50000000000002842, -4.424430252271037922, 6.079088403633667426 ) ) ;
#18374 = VECTOR ( 'NONE', #95052, 1000.000000000000000 ) ;
#18375 = EDGE_CURVE ( 'NONE', #31757, #37517, #50714, .T. ) ;
#18376 = FACE_OUTER_BOUND ( 'NONE', #11796, .T. ) ;
#18377 = AXIS2_PLACEMENT_3D ( 'NONE', #111339, #2044, #82564 ) ;
#18378 = CARTESIAN_POINT ( 'NONE',  ( -4.150000000000025224, 12.50000000000000000, -1.472243186433550122 ) ) ;
#18379 = ORIENTED_EDGE ( 'NONE', *, *, #35690, .F. ) ;
#18380 = CARTESIAN_POINT ( 'NONE',  ( -14.14999999999998792, 12.50000000000000000, -1.472243186433547901 ) ) ;
#18381 = DIRECTION ( 'NONE',  ( 0.000000000000000000, 0.000000000000000000, 1.000000000000000000 ) ) ;
#18382 = CARTESIAN_POINT ( 'NONE',  ( 107.5000000000000142, 0.000000000000000000, 0.000000000000000000 ) ) ;
#18383 = CARTESIAN_POINT ( 'NONE',  ( 185.6510416670080303, 4.367472073101518859, -7.564683531249999149 ) ) ;
#18384 = DIRECTION ( 'NONE',  ( -4.274815082592931898E-19, -0.9999939076577903929, -0.003490651415223739937 ) ) ;
#18385 = EDGE_CURVE ( 'NONE', #95311, #103899, #2668, .T. ) ;
#18386 = LINE ( 'NONE', #66195, #3439 ) ;
#18388 = EDGE_CURVE ( 'NONE', #82453, #118813, #73249, .T. ) ;
#18387 = AXIS2_PLACEMENT_3D ( 'NONE', #6168, #5525, #46112 ) ;
#18389 = ORIENTED_EDGE ( 'NONE', *, *, #34101, .T. ) ;
#18390 = AXIS2_PLACEMENT_3D ( 'NONE', #111121, #71884, #119671 ) ;
#18392 = ORIENTED_EDGE ( 'NONE', *, *, #128930, .F. ) ;
#18391 = AXIS2_PLACEMENT_3D ( 'NONE', #120404, #32038, #90934 ) ;
#18393 = DIRECTION ( 'NONE',  ( -0.000000000000000000, 1.000000000000000000, -0.000000000000000000 ) ) ;
#18394 = ORIENTED_EDGE ( 'NONE', *, *, #122754, .T. ) ;
#18395 = CARTESIAN_POINT ( 'NONE',  ( 0.8499999999999553468, 2.500000000000000000, 2.265063509461097357 ) ) ;
#18396 = EDGE_CURVE ( 'NONE', #33188, #51687, #67405, .T. ) ;
#18398 = ORIENTED_EDGE ( 'NONE', *, *, #59197, .F. ) ;
#18397 = ORIENTED_EDGE ( 'NONE', *, *, #20447, .F. ) ;
#18399 = ADVANCED_FACE ( 'NONE', ( #92910 ), #113167, .T. ) ;
#18400 = ORIENTED_EDGE ( 'NONE', *, *, #61378, .F. ) ;
#18401 = EDGE_CURVE ( 'NONE', #26037, #37993, #73683, .T. ) ;
#18402 = DIRECTION ( 'NONE',  ( -4.274815082592931898E-19, -0.9999939076577903929, -0.003490651415223739937 ) ) ;
#18403 = EDGE_CURVE ( 'NONE', #28723, #103868, #86269, .T. ) ;
#18405 = LINE ( 'NONE', #100194, #90353 ) ;
#18404 = CIRCLE ( 'NONE', #45518, 0.06509327318403741736 ) ;
#18406 = FACE_OUTER_BOUND ( 'NONE', #4447, .T. ) ;
#18407 = ADVANCED_FACE ( 'NONE', ( #24798 ), #111328, .T. ) ;
#18408 = CARTESIAN_POINT ( 'NONE',  ( 2.499999999999948930, 2.500000000000000000, -0.5928203230275541635 ) ) ;
#18409 = FACE_OUTER_BOUND ( 'NONE', #55341, .T. ) ;
#18410 = DIRECTION ( 'NONE',  ( 0.000000000000000000, 0.000000000000000000, 1.000000000000000000 ) ) ;
#18411 = AXIS2_PLACEMENT_3D ( 'NONE', #97167, #37616, #120036 ) ;
#18412 = DIRECTION ( 'NONE',  ( 0.000000000000000000, 0.000000000000000000, 1.000000000000000000 ) ) ;
#18414 = EDGE_CURVE ( 'NONE', #101138, #123793, #119664, .T. ) ;
#18413 = CARTESIAN_POINT ( 'NONE',  ( 0.8499999999999553468, 2.500000000000000000, -2.065063509461102065 ) ) ;
#18415 = ORIENTED_EDGE ( 'NONE', *, *, #43569, .F. ) ;
#18416 = AXIS2_PLACEMENT_3D ( 'NONE', #88177, #28002, #8989 ) ;
#18417 = EDGE_CURVE ( 'NONE', #64400, #55444, #124929, .T. ) ;
#18418 = VERTEX_POINT ( 'NONE', #7064 ) ;
#18419 = ORIENTED_EDGE ( 'NONE', *, *, #32499, .F. ) ;
#18420 = DIRECTION ( 'NONE',  ( -0.000000000000000000, -1.000000000000000000, -0.000000000000000000 ) ) ;
#18421 = VERTEX_POINT ( 'NONE', #35904 ) ;
#18422 = EDGE_LOOP ( 'NONE', ( #105222, #21950 ) ) ;
#18423 = CARTESIAN_POINT ( 'NONE',  ( 11.69999999999990514, 2.500000000000000000, 0.09999999999999772959 ) ) ;
#18424 = VECTOR ( 'NONE', #41452, 1000.000000000000000 ) ;
#18425 = VECTOR ( 'NONE', #9878, 1000.000000000000000 ) ;
#18426 = FACE_OUTER_BOUND ( 'NONE', #65842, .T. ) ;
#18428 = AXIS2_PLACEMENT_3D ( 'NONE', #53899, #124574, #64354 ) ;
#18427 = DIRECTION ( 'NONE',  ( -0.000000000000000000, 1.000000000000000000, -0.000000000000000000 ) ) ;
#18429 = DIRECTION ( 'NONE',  ( -4.274815082592931898E-19, -0.9999939076577903929, -0.003490651415223739937 ) ) ;
#18430 = FACE_OUTER_BOUND ( 'NONE', #100945, .T. ) ;
#18431 = DIRECTION ( 'NONE',  ( -0.000000000000000000, 1.000000000000000000, -0.000000000000000000 ) ) ;
#18432 = EDGE_LOOP ( 'NONE', ( #101870, #113375 ) ) ;
#18433 = AXIS2_PLACEMENT_3D ( 'NONE', #101628, #12574, #121898 ) ;
#18434 = CARTESIAN_POINT ( 'NONE',  ( 6.049999999999934097, 12.50000000000000000, -6.213873640053564351 ) ) ;
#18435 = EDGE_LOOP ( 'NONE', ( #7434, #100166, #57505, #13627 ) ) ;
#18436 = DIRECTION ( 'NONE',  ( 0.000000000000000000, 0.000000000000000000, -1.000000000000000000 ) ) ;
#18437 = ORIENTED_EDGE ( 'NONE', *, *, #97032, .T. ) ;
#18438 = DIRECTION ( 'NONE',  ( 0.000000000000000000, 0.000000000000000000, 1.000000000000000000 ) ) ;
#18439 = ORIENTED_EDGE ( 'NONE', *, *, #123322, .T. ) ;
#18440 = CONICAL_SURFACE ( 'NONE', #39400, 0.1000000000000002554, 0.003490658503988666988 ) ;
#18441 = VERTEX_POINT ( 'NONE', #14935 ) ;
#18442 = CARTESIAN_POINT ( 'NONE',  ( 9.799999999999913669, 12.50000000000000000, -3.983716857408426293 ) ) ;
#18443 = DIRECTION ( 'NONE',  ( 0.000000000000000000, 1.000000000000000000, 0.000000000000000000 ) ) ;
#18444 = CIRCLE ( 'NONE', #22667, 0.06509327318403745899 ) ;
#18445 = DIRECTION ( 'NONE',  ( 0.000000000000000000, 0.000000000000000000, -1.000000000000000000 ) ) ;
#18446 = ADVANCED_FACE ( 'NONE', ( #26728 ), #40262, .T. ) ;
#18447 = CARTESIAN_POINT ( 'NONE',  ( 7.899999999999921307, 2.500000000000000000, -2.385244779468109755E-15 ) ) ;
#18448 = CARTESIAN_POINT ( 'NONE',  ( -8.150000000000012790, 2.500000000000000000, -1.918653347947326004 ) ) ;
#18449 = ORIENTED_EDGE ( 'NONE', *, *, #13194, .T. ) ;
#18450 = SHAPE_REPRESENTATION ( 'Inductive Wireless Charging Base', ( #108296 ), #37304 ) ;
#18451 = FACE_OUTER_BOUND ( 'NONE', #120222, .T. ) ;
#18452 = CARTESIAN_POINT ( 'NONE',  ( 5.399999999999934630, 2.500000000000000000, -0.5928203230275542746 ) ) ;
#18453 = DIRECTION ( 'NONE',  ( -4.274815082592931898E-19, -0.9999939076577903929, -0.003490651415223739937 ) ) ;
#18454 = CARTESIAN_POINT ( 'NONE',  ( 3.349999999999941025, 2.500000000000000000, 7.188010851410848723 ) ) ;
#18456 = EDGE_CURVE ( 'NONE', #100810, #19127, #96105, .T. ) ;
#18455 = DIRECTION ( 'NONE',  ( 0.000000000000000000, 0.000000000000000000, 1.000000000000000000 ) ) ;
#18457 = ORIENTED_EDGE ( 'NONE', *, *, #93178, .T. ) ;
#18458 = ORIENTED_EDGE ( 'NONE', *, *, #48377, .T. ) ;
#18459 = CIRCLE ( 'NONE', #60339, 0.09999999999999982514 ) ;
#18460 = FACE_OUTER_BOUND ( 'NONE', #33792, .T. ) ;
#18461 = ORIENTED_EDGE ( 'NONE', *, *, #26133, .F. ) ;
#18462 = DIRECTION ( 'NONE',  ( 0.000000000000000000, 0.000000000000000000, 1.000000000000000000 ) ) ;
#18463 = DIRECTION ( 'NONE',  ( -0.000000000000000000, 1.000000000000000000, -0.000000000000000000 ) ) ;
#18464 = CIRCLE ( 'NONE', #102378, 0.06509327318403745899 ) ;
#18465 = AXIS2_PLACEMENT_3D ( 'NONE', #39850, #28726, #50294 ) ;
#18466 = EDGE_LOOP ( 'NONE', ( #73540, #39509, #62442, #18721 ) ) ;
#18467 = CARTESIAN_POINT ( 'NONE',  ( 185.7916666666666572, 4.445597072760120838, -7.699999999999998401 ) ) ;
#18468 = DIRECTION ( 'NONE',  ( 0.000000000000000000, 0.000000000000000000, 1.000000000000000000 ) ) ;
#18469 = DIRECTION ( 'NONE',  ( -0.000000000000000000, -1.000000000000000000, -0.000000000000000000 ) ) ;
#18470 = CARTESIAN_POINT ( 'NONE',  ( -9.600000000000006750, 12.50000000000000000, 4.957854068765711553 ) ) ;
#18471 = ORIENTED_EDGE ( 'NONE', *, *, #121181, .F. ) ;
#18472 = CIRCLE ( 'NONE', #91628, 0.09999999999999999167 ) ;
#18473 = CONICAL_SURFACE ( 'NONE', #14261, 0.1000000000000002554, 0.003490658503988666988 ) ;
#18474 = CARTESIAN_POINT ( 'NONE',  ( 187.5000000000000000, 0.000000000000000000, 0.000000000000000000 ) ) ;
#18475 = VERTEX_POINT ( 'NONE', #25417 ) ;
#18476 = PLANE ( 'NONE',  #109117 ) ;
#18477 = DIRECTION ( 'NONE',  ( 0.000000000000000000, 0.000000000000000000, 1.000000000000000000 ) ) ;
#18478 = AXIS2_PLACEMENT_3D ( 'NONE', #43791, #104611, #103984 ) ;
#18479 = DIRECTION ( 'NONE',  ( 0.000000000000000000, 0.000000000000000000, 1.000000000000000000 ) ) ;
#18480 = CIRCLE ( 'NONE', #108366, 0.06509327318403745899 ) ;
#18481 = VERTEX_POINT ( 'NONE', #5144 ) ;
#18482 = CARTESIAN_POINT ( 'NONE',  ( -1.650000000000034328, 2.500000000000000000, -2.857883832488653741 ) ) ;
#18483 = VERTEX_POINT ( 'NONE', #66639 ) ;
#18484 = CARTESIAN_POINT ( 'NONE',  ( -12.69999999999999218, 12.50000000000000000, -4.741630453620012453 ) ) ;
#18485 = CARTESIAN_POINT ( 'NONE',  ( -5.650000000000023448, 2.500000000000000000, -6.941600689897078347 ) ) ;
#18486 = DIRECTION ( 'NONE',  ( 0.000000000000000000, 0.000000000000000000, -1.000000000000000000 ) ) ;
#18487 = ORIENTED_EDGE ( 'NONE', *, *, #95960, .T. ) ;
#18489 = ADVANCED_FACE ( 'NONE', ( #17535 ), #75813, .F. ) ;
#18488 = AXIS2_PLACEMENT_3D ( 'NONE', #61535, #91620, #41898 ) ;
#18490 = CARTESIAN_POINT ( 'NONE',  ( 4.999999999999935163, 12.50000000000000000, 0.6928203230275494784 ) ) ;
#18491 = CARTESIAN_POINT ( 'NONE',  ( 8.749999999999920064, 12.50000000000000000, -2.857883832488653741 ) ) ;
#18492 = AXIS2_PLACEMENT_3D ( 'NONE', #4739, #84620, #35529 ) ;
#18493 = ORIENTED_EDGE ( 'NONE', *, *, #86362, .F. ) ;
#18494 = EDGE_CURVE ( 'NONE', #125159, #14617, #117585, .T. ) ;
#18495 = CARTESIAN_POINT ( 'NONE',  ( -8.350000000000013856, 12.50000000000000000, -6.560283801567334372 ) ) ;
#18496 = EDGE_CURVE ( 'NONE', #64737, #89101, #6772, .T. ) ;
#18497 = ORIENTED_EDGE ( 'NONE', *, *, #36520, .F. ) ;
#18498 = DIRECTION ( 'NONE',  ( 0.000000000000000000, 0.000000000000000000, 1.000000000000000000 ) ) ;
#18499 = AXIS2_PLACEMENT_3D ( 'NONE', #88957, #19567, #38589 ) ;
#18500 = VERTEX_POINT ( 'NONE', #7712 ) ;
#18501 = DIRECTION ( 'NONE',  ( 0.000000000000000000, 1.000000000000000000, 0.000000000000000000 ) ) ;
#18502 = DIRECTION ( 'NONE',  ( -0.000000000000000000, 1.000000000000000000, -0.000000000000000000 ) ) ;
#18503 = EDGE_CURVE ( 'NONE', #2195, #72665, #27724, .T. ) ;
#18504 = EDGE_LOOP ( 'NONE', ( #118652, #11125, #92586, #39286 ) ) ;
#18505 = ORIENTED_EDGE ( 'NONE', *, *, #22569, .T. ) ;
#18506 = EDGE_CURVE ( 'NONE', #32289, #64667, #79958, .T. ) ;
#18507 = CARTESIAN_POINT ( 'NONE',  ( 8.749999999999953815, 12.50000000000000000, 6.495190528383297135 ) ) ;
#18508 = CARTESIAN_POINT ( 'NONE',  ( -12.89999999999999147, 2.500000000000000000, -0.09999999999999815981 ) ) ;
#18509 = AXIS2_PLACEMENT_3D ( 'NONE', #52701, #92631, #124019 ) ;
#18510 = VERTEX_POINT ( 'NONE', #16236 ) ;
#18511 = LINE ( 'NONE', #79380, #126240 ) ;
#18512 = CARTESIAN_POINT ( 'NONE',  ( 186.7760416670080588, 6.551208109652274736, 3.782341765625001351 ) ) ;
#18513 = AXIS2_PLACEMENT_3D ( 'NONE', #103482, #123126, #23627 ) ;
#18514 = DIRECTION ( 'NONE',  ( 0.000000000000000000, 0.000000000000000000, 1.000000000000000000 ) ) ;
#18515 = CARTESIAN_POINT ( 'NONE',  ( 103.0082443037310611, 8.695253764606311719, -0.3321859063348441832 ) ) ;
#18516 = LINE ( 'NONE', #86606, #103190 ) ;
#18517 = DIRECTION ( 'NONE',  ( -0.000000000000000000, -1.000000000000000000, -0.000000000000000000 ) ) ;
#18518 = DIRECTION ( 'NONE',  ( 0.000000000000000000, 1.000000000000000000, 0.000000000000000000 ) ) ;
#18519 = CIRCLE ( 'NONE', #100007, 0.06509327318403745899 ) ;
#18520 = ORIENTED_EDGE ( 'NONE', *, *, #99106, .T. ) ;
#18521 = ORIENTED_EDGE ( 'NONE', *, *, #82137, .T. ) ;
#18522 = VERTEX_POINT ( 'NONE', #56172 ) ;
#18523 = EDGE_LOOP ( 'NONE', ( #45384, #50290 ) ) ;
#18524 = DIRECTION ( 'NONE',  ( -4.274815082592931898E-19, -0.9999939076577903929, -0.003490651415223739937 ) ) ;
#18525 = FACE_OUTER_BOUND ( 'NONE', #48553, .T. ) ;
#18526 = FACE_OUTER_BOUND ( 'NONE', #72709, .T. ) ;
#18527 = AXIS2_PLACEMENT_3D ( 'NONE', #120277, #49613, #20137 ) ;
#18528 = ORIENTED_EDGE ( 'NONE', *, *, #128148, .F. ) ;
#18529 = FACE_BOUND ( 'NONE', #81500, .T. ) ;
#18530 = EDGE_LOOP ( 'NONE', ( #24570, #41127, #88867, #29475 ) ) ;
#18531 = DIRECTION ( 'NONE',  ( -4.274815082592931898E-19, -0.9999939076577903929, -0.003490651415223739937 ) ) ;
#18532 = DIRECTION ( 'NONE',  ( -0.000000000000000000, 1.000000000000000000, -0.000000000000000000 ) ) ;
#18533 = CARTESIAN_POINT ( 'NONE',  ( -5.650000000000019895, 2.500000000000000000, 2.611473670974873151 ) ) ;
#18535 = CONICAL_SURFACE ( 'NONE', #68704, 0.1000000000000002554, 0.003490658503988666988 ) ;
#18534 = AXIS2_PLACEMENT_3D ( 'NONE', #113503, #63776, #103700 ) ;
#18536 = DIRECTION ( 'NONE',  ( 0.000000000000000000, 0.000000000000000000, 1.000000000000000000 ) ) ;
#18537 = CARTESIAN_POINT ( 'NONE',  ( 16.32066102237038052, -2.500000000000000000, -4.877377760480627877 ) ) ;
#18538 = CARTESIAN_POINT ( 'NONE',  ( -6.650000000000019007, 12.50000000000000000, -1.537336459617587581 ) ) ;
#18539 = LINE ( 'NONE', #119309, #22722 ) ;
#18540 = LINE ( 'NONE', #58492, #9569 ) ;
#18541 = CARTESIAN_POINT ( 'NONE',  ( 2.949999999999943334, 12.50000000000000000, 6.430097255199259010 ) ) ;
#18542 = DIRECTION ( 'NONE',  ( 0.000000000000000000, 0.000000000000000000, -1.000000000000000000 ) ) ;
#18543 = ORIENTED_EDGE ( 'NONE', *, *, #127627, .F. ) ;
#18544 = ORIENTED_EDGE ( 'NONE', *, *, #123486, .F. ) ;
#18545 = EDGE_LOOP ( 'NONE', ( #39049, #36035, #61146, #4149 ) ) ;
#18546 = ORIENTED_EDGE ( 'NONE', *, *, #92244, .T. ) ;
#18547 = DIRECTION ( 'NONE',  ( 0.000000000000000000, 0.000000000000000000, 1.000000000000000000 ) ) ;
#18548 = EDGE_CURVE ( 'NONE', #128192, #58954, #36151, .T. ) ;
#18549 = AXIS2_PLACEMENT_3D ( 'NONE', #104638, #112553, #75192 ) ;
#18550 = DIRECTION ( 'NONE',  ( -0.000000000000000000, 1.000000000000000000, -0.000000000000000000 ) ) ;
#18551 = ADVANCED_FACE ( 'NONE', ( #47027 ), #128087, .T. ) ;
#18553 = ORIENTED_EDGE ( 'NONE', *, *, #93943, .T. ) ;
#18552 = ORIENTED_EDGE ( 'NONE', *, *, #128642, .F. ) ;
#18554 = ORIENTED_EDGE ( 'NONE', *, *, #42349, .F. ) ;
#18555 = EDGE_CURVE ( 'NONE', #3435, #13662, #100877, .T. ) ;
#18556 = CYLINDRICAL_SURFACE ( 'NONE', #4097, 7.699999999999999289 ) ;
#18557 = AXIS2_PLACEMENT_3D ( 'NONE', #113117, #90908, #52280 ) ;
#18558 = CONICAL_SURFACE ( 'NONE', #85450, 0.09999999999999982514, 0.003490658503988666988 ) ;
#18559 = PLANE ( 'NONE',  #80184 ) ;
#18560 = CARTESIAN_POINT ( 'NONE',  ( 185.7500000000000000, 9.429780353434619030E-16, -7.700000000000000178 ) ) ;
#18562 = PLANE ( 'NONE',  #73084 ) ;
#18561 = AXIS2_PLACEMENT_3D ( 'NONE', #46926, #113726, #105180 ) ;
#18563 = ADVANCED_FACE ( 'NONE', ( #87567 ), #127511, .T. ) ;
#18564 = CARTESIAN_POINT ( 'NONE',  ( -1.050000000000038236, 12.50000000000000000, -1.883746621131363597 ) ) ;
#18565 = CARTESIAN_POINT ( 'NONE',  ( -8.749999999999975131, 2.500000000000000000, -2.165063509461101710 ) ) ;
#18566 = CARTESIAN_POINT ( 'NONE',  ( 7.299999999999927880, 2.500000000000000000, -4.676537180435977881 ) ) ;
#18567 = ORIENTED_EDGE ( 'NONE', *, *, #46424, .T. ) ;
#18570 = ADVANCED_FACE ( 'NONE', ( #77741 ), #28020, .T. ) ;
#18569 = DIRECTION ( 'NONE',  ( -0.000000000000000000, 1.000000000000000000, -0.000000000000000000 ) ) ;
#18568 = VECTOR ( 'NONE', #116449, 1000.000000000000000 ) ;
#18571 = ORIENTED_EDGE ( 'NONE', *, *, #91259, .F. ) ;
#18572 = AXIS2_PLACEMENT_3D ( 'NONE', #104544, #74446, #6957 ) ;
#18573 = EDGE_CURVE ( 'NONE', #120803, #38135, #109805, .T. ) ;
#18574 = EDGE_LOOP ( 'NONE', ( #75497, #6215, #88448, #25602 ) ) ;
#18575 = VERTEX_POINT ( 'NONE', #79066 ) ;
#18576 = CARTESIAN_POINT ( 'NONE',  ( 11.04999999999990656, 2.500000000000000000, -6.048780366869526581 ) ) ;
#18577 = ORIENTED_EDGE ( 'NONE', *, *, #79558, .F. ) ;
#18578 = EDGE_LOOP ( 'NONE', ( #32570, #122849, #77306, #110469 ) ) ;
#18579 = EDGE_CURVE ( 'NONE', #10886, #29292, #36053, .T. ) ;
#18580 = AXIS2_PLACEMENT_3D ( 'NONE', #9490, #57952, #107021 ) ;
#18581 = DIRECTION ( 'NONE',  ( -0.000000000000000000, -1.000000000000000000, -0.000000000000000000 ) ) ;
#18582 = AXIS2_PLACEMENT_3D ( 'NONE', #69977, #39250, #118417 ) ;
#18583 = LINE ( 'NONE', #77495, #7790 ) ;
#18584 = FACE_OUTER_BOUND ( 'NONE', #74217, .T. ) ;
#18585 = CARTESIAN_POINT ( 'NONE',  ( -7.500000000000015099, 12.50000000000000000, -5.022947341949754119 ) ) ;
#18586 = DIRECTION ( 'NONE',  ( -0.000000000000000000, -1.000000000000000000, -0.000000000000000000 ) ) ;
#18587 = VERTEX_POINT ( 'NONE', #118972 ) ;
#18588 = CARTESIAN_POINT ( 'NONE',  ( 10.19999999999991047, 2.500000000000000000, 4.776537180435972196 ) ) ;
#18589 = CIRCLE ( 'NONE', #91745, 0.1000000000000002554 ) ;
#18590 = VERTEX_POINT ( 'NONE', #40437 ) ;
#18591 = CARTESIAN_POINT ( 'NONE',  ( 11.24999999999994316, 2.500000000000000000, 2.165063509461097713 ) ) ;
#18592 = EDGE_LOOP ( 'NONE', ( #18571, #54827, #20337, #94269 ) ) ;
#18593 = CARTESIAN_POINT ( 'NONE',  ( -3.750000000000027534, 2.500000000000000000, -1.472243186433550122 ) ) ;
#18594 = DIRECTION ( 'NONE',  ( 0.000000000000000000, -0.000000000000000000, 1.000000000000000000 ) ) ;
#18595 = VECTOR ( 'NONE', #108752, 1000.000000000000000 ) ;
#18596 = ORIENTED_EDGE ( 'NONE', *, *, #55304, .T. ) ;
#18597 = CARTESIAN_POINT ( 'NONE',  ( 10.64999999999990976, 2.500000000000000000, -6.148780366869526226 ) ) ;
#18598 = DIRECTION ( 'NONE',  ( -0.000000000000000000, 1.000000000000000000, -0.000000000000000000 ) ) ;
#18599 = EDGE_LOOP ( 'NONE', ( #71382, #127309, #21671, #99524 ) ) ;
#18600 = AXIS2_PLACEMENT_3D ( 'NONE', #23255, #52728, #103119 ) ;
#18601 = DIRECTION ( 'NONE',  ( 0.000000000000000000, 0.000000000000000000, 1.000000000000000000 ) ) ;
#18602 = VERTEX_POINT ( 'NONE', #117653 ) ;
#18603 = EDGE_LOOP ( 'NONE', ( #115761, #6895, #34353, #38959 ) ) ;
#18604 = DIRECTION ( 'NONE',  ( -0.000000000000000000, -1.000000000000000000, -0.000000000000000000 ) ) ;
#18605 = DIRECTION ( 'NONE',  ( 1.000000000000000000, 0.000000000000000000, 0.000000000000000000 ) ) ;
#18606 = CARTESIAN_POINT ( 'NONE',  ( 186.1718750003414016, 9.264065473108010111E-16, -7.564683531250000925 ) ) ;
#18608 = AXIS2_PLACEMENT_3D ( 'NONE', #33709, #113558, #91985 ) ;
#18607 = DIRECTION ( 'NONE',  ( 0.000000000000000000, 0.000000000000000000, 1.000000000000000000 ) ) ;
#18609 = AXIS2_PLACEMENT_3D ( 'NONE', #48426, #7194, #118448 ) ;
#18611 = ADVANCED_FACE ( 'NONE', ( #107861 ), #105071, .T. ) ;
#18610 = CARTESIAN_POINT ( 'NONE',  ( -11.25000000000000178, 2.500000000000000000, -5.702370205355745902 ) ) ;
#18612 = CARTESIAN_POINT ( 'NONE',  ( 0.6499999999999543920, 2.500000000000000000, 6.148780366869520897 ) ) ;
#18613 = AXIS2_PLACEMENT_3D ( 'NONE', #1640, #112263, #42897 ) ;
#18614 = ORIENTED_EDGE ( 'NONE', *, *, #85736, .F. ) ;
#18615 = CARTESIAN_POINT ( 'NONE',  ( 2.499999999999945377, 2.500000000000000000, 5.122947341949749323 ) ) ;
#18616 = FACE_OUTER_BOUND ( 'NONE', #37833, .T. ) ;
#18617 = EDGE_LOOP ( 'NONE', ( #45672, #41954 ) ) ;
#18618 = AXIS2_PLACEMENT_3D ( 'NONE', #121043, #91588, #42504 ) ;
#18619 = CIRCLE ( 'NONE', #27035, 0.06509327318403745899 ) ;
#18620 = CARTESIAN_POINT ( 'NONE',  ( -1.650000000000034328, 12.50000000000000000, -2.857883832488653741 ) ) ;
#18621 = DIRECTION ( 'NONE',  ( 0.000000000000000000, 0.000000000000000000, 1.000000000000000000 ) ) ;
#18622 = DIRECTION ( 'NONE',  ( 0.000000000000000000, 0.000000000000000000, -1.000000000000000000 ) ) ;
#18623 = DIRECTION ( 'NONE',  ( 0.000000000000000000, 0.000000000000000000, 1.000000000000000000 ) ) ;
#18624 = DIRECTION ( 'NONE',  ( -0.000000000000000000, 1.000000000000000000, -0.000000000000000000 ) ) ;
#18625 = ORIENTED_EDGE ( 'NONE', *, *, #3429, .T. ) ;
#18627 = CIRCLE ( 'NONE', #81336, 0.09999999999999982514 ) ;
#18626 = AXIS2_PLACEMENT_3D ( 'NONE', #112466, #120984, #120351 ) ;
#18628 = DIRECTION ( 'NONE',  ( -0.000000000000000000, 1.000000000000000000, -0.000000000000000000 ) ) ;
#18629 = ORIENTED_EDGE ( 'NONE', *, *, #105223, .F. ) ;
#18630 = DIRECTION ( 'NONE',  ( 0.000000000000000000, -0.000000000000000000, 1.000000000000000000 ) ) ;
#18631 = EDGE_LOOP ( 'NONE', ( #75650, #39003 ) ) ;
#18632 = EDGE_LOOP ( 'NONE', ( #59240, #78890, #16554, #124288 ) ) ;
#18633 = LINE ( 'NONE', #88672, #111462 ) ;
#18634 = VECTOR ( 'NONE', #124625, 1000.000000000000000 ) ;
#18635 = ORIENTED_EDGE ( 'NONE', *, *, #96176, .F. ) ;
#18636 = CARTESIAN_POINT ( 'NONE',  ( 9.799999999999913669, 12.50000000000000000, 4.676537180435972552 ) ) ;
#18637 = FACE_OUTER_BOUND ( 'NONE', #28058, .T. ) ;
#18638 = EDGE_LOOP ( 'NONE', ( #126585, #120510, #32192, #24815 ) ) ;
#18639 = ADVANCED_FACE ( 'NONE', ( #8361 ), #13035, .T. ) ;
#18640 = CARTESIAN_POINT ( 'NONE',  ( 1.649999999999951505, 2.500000000000000000, -1.472243186433550122 ) ) ;
#18641 = AXIS2_PLACEMENT_3D ( 'NONE', #28105, #37921, #56888 ) ;
#18643 = ORIENTED_EDGE ( 'NONE', *, *, #94948, .F. ) ;
#18642 = CARTESIAN_POINT ( 'NONE',  ( 6.649999999999927525, 2.500000000000000000, 2.265063509461097357 ) ) ;
#18644 = DIRECTION ( 'NONE',  ( -4.274815082592931898E-19, -0.9999939076577903929, -0.003490651415223739937 ) ) ;
#18645 = EDGE_CURVE ( 'NONE', #120001, #97971, #88194, .T. ) ;
#18646 = CARTESIAN_POINT ( 'NONE',  ( 10.19999999999991580, 12.50000000000000000, -0.3464101615137783474 ) ) ;
#18647 = EDGE_CURVE ( 'NONE', #115023, #127206, #105181, .T. ) ;
#18648 = AXIS2_PLACEMENT_3D ( 'NONE', #56584, #57249, #116155 ) ;
#18649 = ORIENTED_EDGE ( 'NONE', *, *, #12144, .T. ) ;
#18650 = CIRCLE ( 'NONE', #31289, 0.09999999999999999167 ) ;
#18651 = AXIS2_PLACEMENT_3D ( 'NONE', #127082, #46560, #37414 ) ;
#18652 = ORIENTED_EDGE ( 'NONE', *, *, #75545, .F. ) ;
#18653 = ORIENTED_EDGE ( 'NONE', *, *, #40994, .T. ) ;
#18654 = DIRECTION ( 'NONE',  ( 0.000000000000000000, 1.000000000000000000, 0.000000000000000000 ) ) ;
#18655 = CARTESIAN_POINT ( 'NONE',  ( -5.450000000000019718, 12.50000000000000000, 2.165063509461097713 ) ) ;
#18656 = EDGE_CURVE ( 'NONE', #98821, #43976, #99989, .T. ) ;
#18657 = EDGE_CURVE ( 'NONE', #121861, #1292, #128155, .T. ) ;
#18658 = LINE ( 'NONE', #116849, #100694 ) ;
#18659 = ADVANCED_FACE ( 'NONE', ( #78433 ), #67508, .T. ) ;
#18660 = FACE_BOUND ( 'NONE', #119961, .T. ) ;
#18662 = ADVANCED_FACE ( 'NONE', ( #119610 ), #98928, .T. ) ;
#18661 = EDGE_LOOP ( 'NONE', ( #42686, #18232 ) ) ;
#18663 = ADVANCED_FACE ( 'NONE', ( #29960 ), #49610, .T. ) ;
#18664 = CIRCLE ( 'NONE', #39626, 0.09999999999999999167 ) ;
#18665 = DIRECTION ( 'NONE',  ( 0.000000000000000000, 0.000000000000000000, -1.000000000000000000 ) ) ;
#18666 = LINE ( 'NONE', #89346, #68977 ) ;
#18667 = ORIENTED_EDGE ( 'NONE', *, *, #68463, .T. ) ;
#18668 = CYLINDRICAL_SURFACE ( 'NONE', #29927, 7.699999999999999289 ) ;
#18669 = FACE_OUTER_BOUND ( 'NONE', #9388, .T. ) ;
#18670 = DIRECTION ( 'NONE',  ( -0.000000000000000000, -1.000000000000000000, -0.000000000000000000 ) ) ;
#18671 = CARTESIAN_POINT ( 'NONE',  ( -7.500000000000015099, 12.50000000000000000, -0.6277270498435166823 ) ) ;
#18672 = DIRECTION ( 'NONE',  ( 0.000000000000000000, 0.000000000000000000, 1.000000000000000000 ) ) ;
#18673 = EDGE_CURVE ( 'NONE', #23087, #107893, #13132, .T. ) ;
#18674 = DIRECTION ( 'NONE',  ( -4.274815082592931898E-19, -0.9999939076577903929, -0.003490651415223739937 ) ) ;
#18675 = DIRECTION ( 'NONE',  ( 0.000000000000000000, 1.000000000000000000, 0.000000000000000000 ) ) ;
#18676 = VERTEX_POINT ( 'NONE', #70511 ) ;
#18677 = ORIENTED_EDGE ( 'NONE', *, *, #20763, .T. ) ;
#18678 = ORIENTED_EDGE ( 'NONE', *, *, #121124, .T. ) ;
#18679 = ORIENTED_EDGE ( 'NONE', *, *, #74890, .F. ) ;
#18680 = VERTEX_POINT ( 'NONE', #79689 ) ;
#18681 = AXIS2_PLACEMENT_3D ( 'NONE', #86210, #80286, #79628 ) ;
#18682 = CARTESIAN_POINT ( 'NONE',  ( 9.999999999999912959, 2.500000000000000000, 3.537306695894645081 ) ) ;
#18683 = DIRECTION ( 'NONE',  ( 0.000000000000000000, 1.000000000000000000, 0.000000000000000000 ) ) ;
#18684 = ORIENTED_EDGE ( 'NONE', *, *, #634, .F. ) ;
#18685 = FACE_BOUND ( 'NONE', #82515, .T. ) ;
#18686 = DIRECTION ( 'NONE',  ( 0.000000000000000000, 0.000000000000000000, -1.000000000000000000 ) ) ;
#18687 = DIRECTION ( 'NONE',  ( 0.000000000000000000, 1.000000000000000000, 0.000000000000000000 ) ) ;
#18688 = DIRECTION ( 'NONE',  ( 0.000000000000000000, -0.000000000000000000, 1.000000000000000000 ) ) ;
#18689 = CARTESIAN_POINT ( 'NONE',  ( -1.450000000000036371, 12.50000000000000000, 2.511473670974873507 ) ) ;
#18690 = CARTESIAN_POINT ( 'NONE',  ( -2.950000000000030376, 2.500000000000000000, 6.495190528383297135 ) ) ;
#18691 = ORIENTED_EDGE ( 'NONE', *, *, #1378, .F. ) ;
#18692 = AXIS2_PLACEMENT_3D ( 'NONE', #36141, #46592, #27582 ) ;
#18693 = EDGE_LOOP ( 'NONE', ( #84986, #79542, #2009, #96102 ) ) ;
#18694 = ORIENTED_EDGE ( 'NONE', *, *, #89057, .T. ) ;
#18695 = ORIENTED_EDGE ( 'NONE', *, *, #72, .F. ) ;
#18696 = CARTESIAN_POINT ( 'NONE',  ( -5.000000000000023093, 12.50000000000000000, 5.022947341949748790 ) ) ;
#18697 = CARTESIAN_POINT ( 'NONE',  ( 8.920123399827135202, 2.500000000000000444, 8.410822907074514632 ) ) ;
#18698 = DIRECTION ( 'NONE',  ( 0.000000000000000000, 1.000000000000000000, 0.000000000000000000 ) ) ;
#18699 = EDGE_CURVE ( 'NONE', #32827, #27222, #48762, .T. ) ;
#18700 = AXIS2_PLACEMENT_3D ( 'NONE', #19182, #9396, #126592 ) ;
#18701 = ORIENTED_EDGE ( 'NONE', *, *, #19892, .F. ) ;
#18702 = CARTESIAN_POINT ( 'NONE',  ( -12.69999999999999218, 2.500000000000000000, 4.676537180435972552 ) ) ;
#18703 = EDGE_CURVE ( 'NONE', #79119, #4868, #9005, .T. ) ;
#18704 = FACE_OUTER_BOUND ( 'NONE', #12966, .T. ) ;
#18705 = ADVANCED_FACE ( 'NONE', ( #467 ), #60708, .F. ) ;
#18708 = CIRCLE ( 'NONE', #35446, 0.06509327318403745899 ) ;
#18707 = LINE ( 'NONE', #107077, #60354 ) ;
#18706 = VECTOR ( 'NONE', #27958, 1000.000000000000000 ) ;
#18709 = CARTESIAN_POINT ( 'NONE',  ( 185.2343750003414016, 8.734944146203032389, 5.348610694689227483E-16 ) ) ;
#18710 = FACE_OUTER_BOUND ( 'NONE', #35915, .T. ) ;
#18711 = DIRECTION ( 'NONE',  ( 0.000000000000000000, 0.000000000000000000, 1.000000000000000000 ) ) ;
#18712 = CIRCLE ( 'NONE', #121123, 0.06509327318403745899 ) ;
#18713 = DIRECTION ( 'NONE',  ( 0.000000000000000000, 0.000000000000000000, -1.000000000000000000 ) ) ;
#18714 = ADVANCED_FACE ( 'NONE', ( #83576 ), #34092, .T. ) ;
#18715 = VERTEX_POINT ( 'NONE', #31254 ) ;
#18716 = CARTESIAN_POINT ( 'NONE',  ( 1.249999999999952038, 2.500000000000000000, -1.472243186433550122 ) ) ;
#18717 = EDGE_CURVE ( 'NONE', #94678, #26454, #42357, .T. ) ;
#18719 = AXIS2_PLACEMENT_3D ( 'NONE', #106377, #35083, #76280 ) ;
#18718 = AXIS2_PLACEMENT_3D ( 'NONE', #69137, #10847, #61926 ) ;
#18720 = EDGE_CURVE ( 'NONE', #93687, #62761, #52870, .T. ) ;
#18721 = ORIENTED_EDGE ( 'NONE', *, *, #86837, .F. ) ;
#18722 = EDGE_CURVE ( 'NONE', #102277, #78527, #82208, .T. ) ;
#18723 = VERTEX_POINT ( 'NONE', #111060 ) ;
#18724 = DIRECTION ( 'NONE',  ( 0.000000000000000000, 0.000000000000000000, 1.000000000000000000 ) ) ;
#18725 = CARTESIAN_POINT ( 'NONE',  ( 1.249999999999952038, 12.50000000000000000, -1.472243186433550122 ) ) ;
#18726 = DIRECTION ( 'NONE',  ( 0.000000000000000000, 1.000000000000000000, 0.000000000000000000 ) ) ;
#18727 = ORIENTED_EDGE ( 'NONE', *, *, #59483, .F. ) ;
#18728 = ADVANCED_FACE ( 'NONE', ( #92079 ), #82928, .T. ) ;
#18729 = ORIENTED_EDGE ( 'NONE', *, *, #31419, .T. ) ;
#18730 = CARTESIAN_POINT ( 'NONE',  ( -7.100000000000014744, 2.500000000000000000, 4.430127018922196847 ) ) ;
#18731 = DIRECTION ( 'NONE',  ( 0.000000000000000000, -0.000000000000000000, 1.000000000000000000 ) ) ;
#18732 = CARTESIAN_POINT ( 'NONE',  ( 0.1999999999999571565, 2.500000000000000000, 3.983716857408420076 ) ) ;
#18734 = EDGE_LOOP ( 'NONE', ( #114827, #10811 ) ) ;
#18733 = CONICAL_SURFACE ( 'NONE', #102279, 0.1000000000000002554, 0.003490658503988666988 ) ;
#18735 = ORIENTED_EDGE ( 'NONE', *, *, #106902, .T. ) ;
#18736 = DIRECTION ( 'NONE',  ( -0.000000000000000000, -1.000000000000000000, -0.000000000000000000 ) ) ;
#18737 = ORIENTED_EDGE ( 'NONE', *, *, #42194, .F. ) ;
#18738 = CARTESIAN_POINT ( 'NONE',  ( 6.249999999999928946, 2.500000000000000000, 2.857883832488649301 ) ) ;
#18739 = ORIENTED_EDGE ( 'NONE', *, *, #80298, .F. ) ;
#18740 = CARTESIAN_POINT ( 'NONE',  ( 5.649999999999932854, 2.500000000000000000, 1.818653347947321475 ) ) ;
#18741 = CARTESIAN_POINT ( 'NONE',  ( 184.5000000000000000, 0.000000000000000000, -5.200000000000000178 ) ) ;
#18742 = LINE ( 'NONE', #78974, #80357 ) ;
#18743 = EDGE_CURVE ( 'NONE', #12428, #99630, #29883, .T. ) ;
#18744 = FACE_OUTER_BOUND ( 'NONE', #125110, .T. ) ;
#18745 = AXIS2_PLACEMENT_3D ( 'NONE', #73500, #12008, #53239 ) ;
#18746 = ORIENTED_EDGE ( 'NONE', *, *, #113890, .F. ) ;
#18748 = AXIS2_PLACEMENT_3D ( 'NONE', #20349, #119831, #108717 ) ;
#18747 = AXIS2_PLACEMENT_3D ( 'NONE', #27134, #66401, #67029 ) ;
#18749 = ORIENTED_EDGE ( 'NONE', *, *, #118180, .F. ) ;
#18750 = ORIENTED_EDGE ( 'NONE', *, *, #51539, .T. ) ;
#18751 = CARTESIAN_POINT ( 'NONE',  ( -12.04999999999999538, 2.500000000000000000, 2.165063509461097713 ) ) ;
#18752 = DIRECTION ( 'NONE',  ( 0.000000000000000000, 1.000000000000000000, 0.000000000000000000 ) ) ;
#18753 = PLANE ( 'NONE',  #3025 ) ;
#18754 = CARTESIAN_POINT ( 'NONE',  ( 8.149999999999920419, 2.500000000000000000, -2.611473670974877592 ) ) ;
#18755 = CONICAL_SURFACE ( 'NONE', #50175, 0.1000000000000002554, 0.003490658503988666988 ) ;
#18756 = DIRECTION ( 'NONE',  ( 0.000000000000000000, 0.000000000000000000, 1.000000000000000000 ) ) ;
#18757 = CARTESIAN_POINT ( 'NONE',  ( 3.749999999999944045, 2.500000000000000000, -2.857883832488653741 ) ) ;
#18758 = CONICAL_SURFACE ( 'NONE', #91922, 0.1000000000000000056, 0.003490658503988666988 ) ;
#18759 = AXIS2_PLACEMENT_3D ( 'NONE', #103660, #15899, #13964 ) ;
#18761 = EDGE_CURVE ( 'NONE', #123229, #35564, #71158, .T. ) ;
#18760 = DIRECTION ( 'NONE',  ( 0.000000000000000000, 0.000000000000000000, 1.000000000000000000 ) ) ;
#18762 = CARTESIAN_POINT ( 'NONE',  ( 12.09999999999990550, 12.50000000000000000, -3.637306695894650055 ) ) ;
#18763 = FACE_OUTER_BOUND ( 'NONE', #122110, .T. ) ;
#18764 = DIRECTION ( 'NONE',  ( -0.000000000000000000, -1.000000000000000000, -0.000000000000000000 ) ) ;
#18765 = AXIS2_PLACEMENT_3D ( 'NONE', #26860, #34765, #46486 ) ;
#18766 = ORIENTED_EDGE ( 'NONE', *, *, #106417, .F. ) ;
#18767 = CIRCLE ( 'NONE', #68952, 0.06509327318403745899 ) ;
#18768 = CARTESIAN_POINT ( 'NONE',  ( 11.64999999999990621, 12.50000000000000000, -2.165063509461101710 ) ) ;
#18769 = EDGE_CURVE ( 'NONE', #111172, #26322, #54101, .T. ) ;
#18770 = DIRECTION ( 'NONE',  ( 0.000000000000000000, -0.000000000000000000, 1.000000000000000000 ) ) ;
#18771 = DIRECTION ( 'NONE',  ( -0.000000000000000000, -1.000000000000000000, -0.000000000000000000 ) ) ;
#18772 = DIRECTION ( 'NONE',  ( 0.000000000000000000, 1.000000000000000000, 0.000000000000000000 ) ) ;
#18773 = DIRECTION ( 'NONE',  ( -0.000000000000000000, -1.000000000000000000, -0.000000000000000000 ) ) ;
#18774 = VERTEX_POINT ( 'NONE', #33194 ) ;
#18775 = DIRECTION ( 'NONE',  ( 0.000000000000000000, 0.000000000000000000, 1.000000000000000000 ) ) ;
#18776 = LINE ( 'NONE', #56120, #65867 ) ;
#18778 = ORIENTED_EDGE ( 'NONE', *, *, #77905, .T. ) ;
#18777 = CARTESIAN_POINT ( 'NONE',  ( -14.39999999999998614, 2.500000000000000000, 0.3464101615137758494 ) ) ;
#18779 = ORIENTED_EDGE ( 'NONE', *, *, #6397, .T. ) ;
#18780 = CARTESIAN_POINT ( 'NONE',  ( 105.0000000000000142, 9.000000000000001776, 0.2500000000000003886 ) ) ;
#18781 = ORIENTED_EDGE ( 'NONE', *, *, #3234, .F. ) ;
#18782 = ORIENTED_EDGE ( 'NONE', *, *, #30336, .T. ) ;
#18783 = ORIENTED_EDGE ( 'NONE', *, *, #14336, .F. ) ;
#18784 = LINE ( 'NONE', #38456, #103359 ) ;
#18785 = CIRCLE ( 'NONE', #91962, 0.1000000000000002554 ) ;
#18786 = LINE ( 'NONE', #127468, #117744 ) ;
#18787 = DIRECTION ( 'NONE',  ( 0.000000000000000000, -0.000000000000000000, 1.000000000000000000 ) ) ;
#18788 = CARTESIAN_POINT ( 'NONE',  ( 16.87640210516320138, 2.500000000000000000, -4.436424697255190175 ) ) ;
#18789 = VERTEX_POINT ( 'NONE', #14156 ) ;
#18790 = EDGE_CURVE ( 'NONE', #123810, #56755, #52172, .T. ) ;
#18792 = AXIS2_PLACEMENT_3D ( 'NONE', #47492, #56002, #97227 ) ;
#18791 = CIRCLE ( 'NONE', #91965, 0.06509327318403745899 ) ;
#18793 = PLANE ( 'NONE',  #33612 ) ;
#18794 = ORIENTED_EDGE ( 'NONE', *, *, #61825, .T. ) ;
#18795 = DIRECTION ( 'NONE',  ( 0.000000000000000000, 0.000000000000000000, 1.000000000000000000 ) ) ;
#18796 = CARTESIAN_POINT ( 'NONE',  ( 19.40342015654457342, -2.551666867761286817, -4.359384978533091370 ) ) ;
#18797 = DIRECTION ( 'NONE',  ( -0.000000000000000000, 1.000000000000000000, -0.000000000000000000 ) ) ;
#18798 = CARTESIAN_POINT ( 'NONE',  ( -3.950000000000026379, 2.500000000000000000, -1.818653347947326138 ) ) ;
#18799 = DIRECTION ( 'NONE',  ( 0.000000000000000000, 0.000000000000000000, 1.000000000000000000 ) ) ;
#18800 = EDGE_LOOP ( 'NONE', ( #112911, #17433, #117356, #114410 ) ) ;
#18802 = AXIS2_PLACEMENT_3D ( 'NONE', #85767, #34113, #4609 ) ;
#18801 = VECTOR ( 'NONE', #51948, 1000.000000000000000 ) ;
#18803 = ORIENTED_EDGE ( 'NONE', *, *, #115388, .T. ) ;
#18804 = ORIENTED_EDGE ( 'NONE', *, *, #236, .T. ) ;
#18805 = ORIENTED_EDGE ( 'NONE', *, *, #20304, .T. ) ;
#18806 = EDGE_LOOP ( 'NONE', ( #117930, #95849 ) ) ;
#18807 = DIRECTION ( 'NONE',  ( -0.000000000000000000, -1.000000000000000000, -0.000000000000000000 ) ) ;
#18808 = CARTESIAN_POINT ( 'NONE',  ( -3.950000000000029932, 2.500000000000000000, -6.248780366869526759 ) ) ;
#18809 = EDGE_CURVE ( 'NONE', #8036, #87854, #43654, .T. ) ;
#18810 = EDGE_CURVE ( 'NONE', #48591, #91335, #92744, .T. ) ;
#18811 = DIRECTION ( 'NONE',  ( 0.000000000000000000, 0.000000000000000000, 1.000000000000000000 ) ) ;
#18812 = EDGE_CURVE ( 'NONE', #116552, #39180, #46601, .T. ) ;
#18813 = FACE_BOUND ( 'NONE', #69035, .T. ) ;
#18814 = ADVANCED_FACE ( 'NONE', ( #94022 ), #96758, .T. ) ;
#18815 = CARTESIAN_POINT ( 'NONE',  ( 8.549999999999920774, 12.50000000000000000, 6.148780366869520897 ) ) ;
#18816 = FACE_OUTER_BOUND ( 'NONE', #18940, .T. ) ;
#18817 = DIRECTION ( 'NONE',  ( 0.000000000000000000, -0.9999939076577903929, 0.003490651415223739937 ) ) ;
#18818 = CARTESIAN_POINT ( 'NONE',  ( -1.250000000000035749, 2.500000000000000000, -7.288010851410854585 ) ) ;
#18819 = ADVANCED_FACE ( 'NONE', ( #111731 ), #22082, .T. ) ;
#18820 = CARTESIAN_POINT ( 'NONE',  ( 186.1302083336747444, -4.367472073101514418, -7.564683531250002702 ) ) ;
#18821 = CARTESIAN_POINT ( 'NONE',  ( -2.050000000000033129, 2.500000000000000000, 6.495190528383297135 ) ) ;
#18822 = EDGE_CURVE ( 'NONE', #29211, #23253, #73099, .T. ) ;
#18823 = DIRECTION ( 'NONE',  ( -0.000000000000000000, -1.000000000000000000, -0.000000000000000000 ) ) ;
#18824 = EDGE_CURVE ( 'NONE', #127460, #109714, #90510, .T. ) ;
#18825 = AXIS2_PLACEMENT_3D ( 'NONE', #73299, #113222, #53669 ) ;
#18826 = ADVANCED_FACE ( 'NONE', ( #63274 ), #61284, .T. ) ;
#18827 = CARTESIAN_POINT ( 'NONE',  ( 13.14999999999989733, 12.50000000000000000, -2.446380397790840266 ) ) ;
#18828 = VERTEX_POINT ( 'NONE', #124121 ) ;
#18829 = ORIENTED_EDGE ( 'NONE', *, *, #98337, .T. ) ;
#18830 = VERTEX_POINT ( 'NONE', #76323 ) ;
#18831 = ORIENTED_EDGE ( 'NONE', *, *, #128245, .T. ) ;
#18832 = DIRECTION ( 'NONE',  ( -0.000000000000000000, -1.000000000000000000, -0.000000000000000000 ) ) ;
#18833 = CARTESIAN_POINT ( 'NONE',  ( -10.84999999999999964, 2.500000000000000000, 5.702370205355745014 ) ) ;
#18834 = FACE_BOUND ( 'NONE', #26503, .T. ) ;
#18835 = AXIS2_PLACEMENT_3D ( 'NONE', #106533, #29280, #98633 ) ;
#18836 = LINE ( 'NONE', #16869, #1702 ) ;
#18837 = VERTEX_POINT ( 'NONE', #126715 ) ;
#18838 = CARTESIAN_POINT ( 'NONE',  ( 10.64999999999990976, 2.500000000000000000, -6.148780366869526226 ) ) ;
#18839 = FACE_OUTER_BOUND ( 'NONE', #1758, .T. ) ;
#18840 = FACE_OUTER_BOUND ( 'NONE', #90497, .T. ) ;
#18841 = DIRECTION ( 'NONE',  ( 0.000000000000000000, 0.000000000000000000, 1.000000000000000000 ) ) ;
#18842 = CIRCLE ( 'NONE', #58575, 0.1000000000000002554 ) ;
#18843 = VERTEX_POINT ( 'NONE', #46868 ) ;
#18844 = FACE_OUTER_BOUND ( 'NONE', #115321, .T. ) ;
#18845 = CIRCLE ( 'NONE', #20912, 0.09999999999999982514 ) ;
#18846 = AXIS2_PLACEMENT_3D ( 'NONE', #104140, #94971, #123759 ) ;
#18847 = VERTEX_POINT ( 'NONE', #114938 ) ;
#18848 = ORIENTED_EDGE ( 'NONE', *, *, #30128, .F. ) ;
#18849 = CARTESIAN_POINT ( 'NONE',  ( -4.800000000000026468, 2.500000000000000000, -4.676537180435978769 ) ) ;
#18850 = LINE ( 'NONE', #128847, #39335 ) ;
#18851 = ORIENTED_EDGE ( 'NONE', *, *, #13405, .F. ) ;
#18852 = VECTOR ( 'NONE', #100738, 1000.000000000000000 ) ;
#18853 = CARTESIAN_POINT ( 'NONE',  ( -1.050000000000037348, 12.50000000000000000, -6.776507416713040577 ) ) ;
#18854 = DIRECTION ( 'NONE',  ( 0.000000000000000000, 1.000000000000000000, 0.000000000000000000 ) ) ;
#18855 = EDGE_LOOP ( 'NONE', ( #24640, #37583, #55404, #61190 ) ) ;
#18856 = PLANE ( 'NONE',  #95420 ) ;
#18857 = AXIS2_PLACEMENT_3D ( 'NONE', #114601, #124436, #24945 ) ;
#18858 = EDGE_LOOP ( 'NONE', ( #129272, #65600 ) ) ;
#18859 = FACE_OUTER_BOUND ( 'NONE', #43707, .T. ) ;
#18860 = ORIENTED_EDGE ( 'NONE', *, *, #28487, .T. ) ;
#18861 = FACE_OUTER_BOUND ( 'NONE', #15979, .T. ) ;
#18862 = FACE_BOUND ( 'NONE', #88647, .T. ) ;
#18863 = ADVANCED_FACE ( 'NONE', ( #106418 ), #5623, .T. ) ;
#18864 = ORIENTED_EDGE ( 'NONE', *, *, #7739, .F. ) ;
#18866 = ADVANCED_FACE ( 'NONE', ( #104483 ), #121918, .T. ) ;
#18865 = CARTESIAN_POINT ( 'NONE',  ( 4.149999999999941735, 12.50000000000000000, -5.867463478539787225 ) ) ;
#18867 = ORIENTED_EDGE ( 'NONE', *, *, #121524, .F. ) ;
#18868 = DIRECTION ( 'NONE',  ( 0.000000000000000000, 0.000000000000000000, 1.000000000000000000 ) ) ;
#18869 = DIRECTION ( 'NONE',  ( -0.000000000000000000, 1.000000000000000000, -0.000000000000000000 ) ) ;
#18870 = PLANE ( 'NONE',  #36238 ) ;
#18871 = CARTESIAN_POINT ( 'NONE',  ( -3.350000000000028955, 12.50000000000000000, 7.122917578226811486 ) ) ;
#18872 = CARTESIAN_POINT ( 'NONE',  ( 10.79999999999991012, 12.50000000000000000, 4.330127018922196314 ) ) ;
#18873 = VERTEX_POINT ( 'NONE', #75032 ) ;
#18874 = EDGE_CURVE ( 'NONE', #14289, #112256, #44933, .T. ) ;
#18875 = VERTEX_POINT ( 'NONE', #56019 ) ;
#18876 = ORIENTED_EDGE ( 'NONE', *, *, #3488, .F. ) ;
#18877 = DIRECTION ( 'NONE',  ( 0.000000000000000000, 1.000000000000000000, 0.000000000000000000 ) ) ;
#18878 = PLANE ( 'NONE',  #57794 ) ;
#18880 = DIRECTION ( 'NONE',  ( -0.000000000000000000, 1.000000000000000000, -0.000000000000000000 ) ) ;
#18879 = CONICAL_SURFACE ( 'NONE', #127555, 0.09999999999999999167, 0.003490658503988666988 ) ;
#18882 = ORIENTED_EDGE ( 'NONE', *, *, #3192, .F. ) ;
#18881 = EDGE_LOOP ( 'NONE', ( #98647, #103753 ) ) ;
#18883 = VERTEX_POINT ( 'NONE', #25261 ) ;
#18884 = DIRECTION ( 'NONE',  ( 0.000000000000000000, 0.000000000000000000, 1.000000000000000000 ) ) ;
#18885 = DIRECTION ( 'NONE',  ( -1.000000000000000000, -0.000000000000000000, -0.000000000000000000 ) ) ;
#18886 = CONTEXT_DEPENDENT_SHAPE_REPRESENTATION ( #127459, #85918 ) ;
#18887 = CONICAL_SURFACE ( 'NONE', #121304, 0.1000000000000002554, 0.003490658503988666988 ) ;
#18888 = DIRECTION ( 'NONE',  ( 0.000000000000000000, 0.000000000000000000, -1.000000000000000000 ) ) ;
#18889 = CARTESIAN_POINT ( 'NONE',  ( -10.85000000000000142, 2.500000000000000000, -1.472243186433546125 ) ) ;
#18890 = CARTESIAN_POINT ( 'NONE',  ( -6.250000000000017764, 2.500000000000000000, 2.857883832488649301 ) ) ;
#18891 = DIRECTION ( 'NONE',  ( -0.000000000000000000, -1.000000000000000000, -0.000000000000000000 ) ) ;
#18892 = CARTESIAN_POINT ( 'NONE',  ( 0.8499999999999553468, 12.50000000000000000, -2.099970236277064473 ) ) ;
#18893 = DIRECTION ( 'NONE',  ( 0.000000000000000000, -0.9999939076577903929, 0.003490651415223739937 ) ) ;
#18894 = ORIENTED_EDGE ( 'NONE', *, *, #67726, .F. ) ;
#18895 = ORIENTED_EDGE ( 'NONE', *, *, #45238, .F. ) ;
#18896 = DIRECTION ( 'NONE',  ( 0.000000000000000000, 1.000000000000000000, 0.000000000000000000 ) ) ;
#18897 = DIRECTION ( 'NONE',  ( -4.274815082592931898E-19, -0.9999939076577903929, -0.003490651415223739937 ) ) ;
#18898 = ORIENTED_EDGE ( 'NONE', *, *, #55092, .T. ) ;
#18899 = ORIENTED_EDGE ( 'NONE', *, *, #12512, .T. ) ;
#18900 = CARTESIAN_POINT ( 'NONE',  ( 185.9010416670080303, -4.367472073101519747, 7.564683531249999149 ) ) ;
#18901 = FACE_OUTER_BOUND ( 'NONE', #121687, .T. ) ;
#18902 = DIRECTION ( 'NONE',  ( 0.000000000000000000, 0.000000000000000000, -1.000000000000000000 ) ) ;
#18903 = DIRECTION ( 'NONE',  ( 0.000000000000000000, 0.000000000000000000, 1.000000000000000000 ) ) ;
#18904 = CARTESIAN_POINT ( 'NONE',  ( -1.450000000000035483, 12.50000000000000000, 1.753560074763284016 ) ) ;
#18905 = EDGE_CURVE ( 'NONE', #32401, #72821, #92668, .T. ) ;
#18906 = CARTESIAN_POINT ( 'NONE',  ( 14.54999999999989235, 12.50000000000000000, -2.099970236277064473 ) ) ;
#18907 = CARTESIAN_POINT ( 'NONE',  ( 7.299999999999926104, 2.500000000000000000, -0.3464101615137782364 ) ) ;
#18908 = DIRECTION ( 'NONE',  ( 1.000000000000000000, 0.000000000000000000, 0.000000000000000000 ) ) ;
#18909 = AXIS2_PLACEMENT_3D ( 'NONE', #49855, #89758, #11832 ) ;
#18911 = ORIENTED_EDGE ( 'NONE', *, *, #126272, .F. ) ;
#18910 = AXIS2_PLACEMENT_3D ( 'NONE', #61425, #120964, #60763 ) ;
#18912 = ORIENTED_EDGE ( 'NONE', *, *, #48422, .F. ) ;
#18913 = EDGE_CURVE ( 'NONE', #18680, #121502, #116231, .T. ) ;
#18914 = VERTEX_POINT ( 'NONE', #4981 ) ;
#18916 = ORIENTED_EDGE ( 'NONE', *, *, #20304, .F. ) ;
#18915 = EDGE_CURVE ( 'NONE', #60519, #66379, #94658, .T. ) ;
#18917 = DIRECTION ( 'NONE',  ( 0.000000000000000000, 1.000000000000000000, 0.000000000000000000 ) ) ;
#18918 = PLANE ( 'NONE',  #24839 ) ;
#18919 = CIRCLE ( 'NONE', #117189, 0.06509327318403745899 ) ;
#18920 = ORIENTED_EDGE ( 'NONE', *, *, #65683, .T. ) ;
#18921 = CARTESIAN_POINT ( 'NONE',  ( -10.60000000000000142, 2.500000000000000000, -0.4464101615137782142 ) ) ;
#18922 = FACE_OUTER_BOUND ( 'NONE', #105195, .T. ) ;
#18923 = PLANE ( 'NONE',  #26366 ) ;
#18925 = VERTEX_POINT ( 'NONE', #6903 ) ;
#18924 = DIRECTION ( 'NONE',  ( 0.000000000000000000, 1.000000000000000000, 0.000000000000000000 ) ) ;
#18926 = ADVANCED_FACE ( 'NONE', ( #84194 ), #57055, .T. ) ;
#18927 = CARTESIAN_POINT ( 'NONE',  ( 12.09999999999990550, 2.500000000000000000, 5.022947341949748790 ) ) ;
#18928 = CARTESIAN_POINT ( 'NONE',  ( 5.199999999999933564, 12.50000000000000000, 0.3464101615137735735 ) ) ;
#18929 = CIRCLE ( 'NONE', #112948, 0.1000000000000002554 ) ;
#18930 = ORIENTED_EDGE ( 'NONE', *, *, #22410, .F. ) ;
#18931 = AXIS2_PLACEMENT_3D ( 'NONE', #66618, #123601, #46335 ) ;
#18932 = ORIENTED_EDGE ( 'NONE', *, *, #80789, .F. ) ;
#18933 = EDGE_LOOP ( 'NONE', ( #10267, #14208, #79583, #89567 ) ) ;
#18934 = ORIENTED_EDGE ( 'NONE', *, *, #46428, .T. ) ;
#18935 = PLANE ( 'NONE',  #44775 ) ;
#18936 = CIRCLE ( 'NONE', #44086, 0.06509327318403745899 ) ;
#18937 = DIRECTION ( 'NONE',  ( 0.000000000000000000, 0.000000000000000000, 1.000000000000000000 ) ) ;
#18938 = EDGE_CURVE ( 'NONE', #7520, #7926, #115579, .T. ) ;
#18939 = AXIS2_PLACEMENT_3D ( 'NONE', #110279, #967, #119440 ) ;
#18940 = EDGE_LOOP ( 'NONE', ( #91829, #58214, #34205, #82778, #48164, #34402, #69224, #118172, #104712, #13365, #90243, #89668, #112364, #60147, #77509 ) ) ;
#18941 = DIRECTION ( 'NONE',  ( 0.000000000000000000, 1.000000000000000000, 0.000000000000000000 ) ) ;
#18942 = LINE ( 'NONE', #95590, #7778 ) ;
#18943 = DIRECTION ( 'NONE',  ( -0.000000000000000000, 1.000000000000000000, -0.000000000000000000 ) ) ;
#18944 = DIRECTION ( 'NONE',  ( 0.000000000000000000, 1.000000000000000000, 0.000000000000000000 ) ) ;
#18945 = ADVANCED_FACE ( 'NONE', ( #64557 ), #75931, .T. ) ;
#18946 = VERTEX_POINT ( 'NONE', #34478 ) ;
#18947 = DIRECTION ( 'NONE',  ( 0.000000000000000000, -0.000000000000000000, 1.000000000000000000 ) ) ;
#18948 = EDGE_LOOP ( 'NONE', ( #76792, #113315 ) ) ;
#18949 = ORIENTED_EDGE ( 'NONE', *, *, #58159, .F. ) ;
#18950 = DIRECTION ( 'NONE',  ( 0.000000000000000000, 0.000000000000000000, 1.000000000000000000 ) ) ;
#18951 = EDGE_CURVE ( 'NONE', #40089, #122097, #65464, .T. ) ;
#18952 = EDGE_CURVE ( 'NONE', #24264, #108022, #78092, .T. ) ;
#18953 = CARTESIAN_POINT ( 'NONE',  ( -8.750000000000008882, 2.500000000000000000, -2.857883832488653741 ) ) ;
#18954 = EDGE_CURVE ( 'NONE', #75945, #49108, #65841, .T. ) ;
#18955 = FACE_BOUND ( 'NONE', #112932, .T. ) ;
#18956 = ADVANCED_FACE ( 'NONE', ( #125418 ), #96581, .T. ) ;
#18957 = DIRECTION ( 'NONE',  ( 0.000000000000000000, 0.000000000000000000, -1.000000000000000000 ) ) ;
#18958 = DIRECTION ( 'NONE',  ( 1.000000000000000000, -0.000000000000000000, -0.000000000000000000 ) ) ;
#18959 = DIRECTION ( 'NONE',  ( 0.000000000000000000, 0.000000000000000000, 1.000000000000000000 ) ) ;
#18960 = EDGE_CURVE ( 'NONE', #108184, #62695, #53058, .T. ) ;
#18961 = CIRCLE ( 'NONE', #92125, 0.1000000000000000472 ) ;
#18963 = EDGE_LOOP ( 'NONE', ( #13628, #44121 ) ) ;
#18962 = VECTOR ( 'NONE', #110831, 1000.000000000000000 ) ;
#18965 = AXIS2_PLACEMENT_3D ( 'NONE', #108399, #128046, #50147 ) ;
#18964 = CARTESIAN_POINT ( 'NONE',  ( -2.700000000000030376, 12.50000000000000000, 3.983716857408420964 ) ) ;
#18966 = DIRECTION ( 'NONE',  ( 0.000000000000000000, 0.000000000000000000, 1.000000000000000000 ) ) ;
#18967 = ADVANCED_FACE ( 'NONE', ( #24643 ), #76965, .T. ) ;
#18968 = DIRECTION ( 'NONE',  ( 0.000000000000000000, 1.000000000000000000, 0.000000000000000000 ) ) ;
#18969 = CARTESIAN_POINT ( 'NONE',  ( -5.000000000000024869, 2.500000000000000000, -5.122947341949753763 ) ) ;
#18970 = ORIENTED_EDGE ( 'NONE', *, *, #105000, .F. ) ;
#18971 = DIRECTION ( 'NONE',  ( 0.000000000000000000, 0.000000000000000000, -1.000000000000000000 ) ) ;
#18972 = EDGE_CURVE ( 'NONE', #39660, #52720, #36349, .T. ) ;
#18974 = EDGE_CURVE ( 'NONE', #116295, #20224, #21664, .T. ) ;
#18973 = AXIS2_PLACEMENT_3D ( 'NONE', #42651, #93021, #41987 ) ;
#18975 = DIRECTION ( 'NONE',  ( 1.000000000000000000, 0.000000000000000000, 0.000000000000000000 ) ) ;
#18976 = ORIENTED_EDGE ( 'NONE', *, *, #22400, .T. ) ;
#18977 = EDGE_LOOP ( 'NONE', ( #49172, #18652, #38149, #127878 ) ) ;
#18978 = FACE_OUTER_BOUND ( 'NONE', #20022, .T. ) ;
#18979 = DIRECTION ( 'NONE',  ( 0.000000000000000000, 0.000000000000000000, 1.000000000000000000 ) ) ;
#18980 = FACE_BOUND ( 'NONE', #74132, .T. ) ;
#18981 = ADVANCED_FACE ( 'NONE', ( #98513 ), #71838, .T. ) ;
#18982 = FACE_OUTER_BOUND ( 'NONE', #10974, .T. ) ;
#18983 = ORIENTED_EDGE ( 'NONE', *, *, #39539, .T. ) ;
#18984 = DIRECTION ( 'NONE',  ( 0.000000000000000000, 0.000000000000000000, 1.000000000000000000 ) ) ;
#18985 = ORIENTED_EDGE ( 'NONE', *, *, #96856, .T. ) ;
#18986 = DIRECTION ( 'NONE',  ( -1.000000000000000000, 0.000000000000000000, 0.000000000000000000 ) ) ;
#18987 = CARTESIAN_POINT ( 'NONE',  ( 185.5000000000000000, 0.000000000000000000, 7.700000000000000178 ) ) ;
#18988 = ORIENTED_EDGE ( 'NONE', *, *, #102493, .F. ) ;
#18989 = CARTESIAN_POINT ( 'NONE',  ( -5.650000000000023448, 2.500000000000000000, -6.741600689897078169 ) ) ;
#18990 = CARTESIAN_POINT ( 'NONE',  ( -6.250000000000021316, 12.50000000000000000, -1.472243186433550122 ) ) ;
#18991 = AXIS2_PLACEMENT_3D ( 'NONE', #94214, #73930, #14349 ) ;
#18992 = CARTESIAN_POINT ( 'NONE',  ( -11.05000000000000071, 2.500000000000000000, 6.841600689897072485 ) ) ;
#18993 = CARTESIAN_POINT ( 'NONE',  ( 9.399999999999915090, 2.500000000000000000, -4.676537180435977881 ) ) ;
#18994 = CIRCLE ( 'NONE', #42003, 0.09999999999999982514 ) ;
#18995 = CIRCLE ( 'NONE', #92170, 0.09999999999999982514 ) ;
#18996 = VERTEX_POINT ( 'NONE', #89991 ) ;
#18997 = DIRECTION ( 'NONE',  ( 0.000000000000000000, 0.000000000000000000, 1.000000000000000000 ) ) ;
#18998 = CARTESIAN_POINT ( 'NONE',  ( 9.399999999999918643, 12.50000000000000000, -0.3464101615137782364 ) ) ;
#18999 = DIRECTION ( 'NONE',  ( 0.000000000000000000, 0.000000000000000000, 1.000000000000000000 ) ) ;
#19000 = CARTESIAN_POINT ( 'NONE',  ( -1.850000000000033840, 12.50000000000000000, 1.818653347947321475 ) ) ;
#19001 = ORIENTED_EDGE ( 'NONE', *, *, #68878, .T. ) ;
#19002 = ORIENTED_EDGE ( 'NONE', *, *, #41938, .F. ) ;
#19003 = DIRECTION ( 'NONE',  ( 0.000000000000000000, -0.9999939076577903929, 0.003490651415223739937 ) ) ;
#19004 = AXIS2_PLACEMENT_3D ( 'NONE', #72846, #12620, #22479 ) ;
#19005 = ORIENTED_EDGE ( 'NONE', *, *, #12472, .F. ) ;
#19006 = CARTESIAN_POINT ( 'NONE',  ( 9.399999999999918643, 12.50000000000000000, 0.3464101615137736845 ) ) ;
#19007 = AXIS2_PLACEMENT_3D ( 'NONE', #120498, #70751, #20998 ) ;
#19008 = CARTESIAN_POINT ( 'NONE',  ( 17.50000000000000000, -2.499999999999999556, -2.666666666666662522 ) ) ;
#19009 = EDGE_CURVE ( 'NONE', #56486, #24243, #59928, .T. ) ;
#19010 = FACE_OUTER_BOUND ( 'NONE', #12861, .T. ) ;
#19011 = CARTESIAN_POINT ( 'NONE',  ( -12.89999999999999325, 2.500000000000000000, 0.6928203230275535862 ) ) ;
#19012 = EDGE_LOOP ( 'NONE', ( #11790, #52183, #39715, #35882 ) ) ;
#19014 = EDGE_CURVE ( 'NONE', #6037, #94991, #17429, .T. ) ;
#19013 = DIRECTION ( 'NONE',  ( 0.000000000000000000, 1.000000000000000000, 0.000000000000000000 ) ) ;
#19015 = CARTESIAN_POINT ( 'NONE',  ( -12.69999999999999218, 2.500000000000000000, 4.676537180435972552 ) ) ;
#19016 = DIRECTION ( 'NONE',  ( 0.000000000000000000, 1.000000000000000000, 0.000000000000000000 ) ) ;
#19017 = CARTESIAN_POINT ( 'NONE',  ( 185.5677083336747160, -4.367472073101514418, -7.564683531250002702 ) ) ;
#19018 = CARTESIAN_POINT ( 'NONE',  ( 6.699999999999930012, 12.50000000000000000, 4.330127018922196314 ) ) ;
#19019 = FACE_OUTER_BOUND ( 'NONE', #17913, .T. ) ;
#19020 = EDGE_LOOP ( 'NONE', ( #79457, #98309 ) ) ;
#19021 = AXIS2_PLACEMENT_3D ( 'NONE', #108478, #128134, #98012 ) ;
#19022 = ORIENTED_EDGE ( 'NONE', *, *, #3044, .T. ) ;
#19023 = CARTESIAN_POINT ( 'NONE',  ( -12.69999999999999396, 12.50000000000000000, 0.3464101615137776813 ) ) ;
#19024 = ORIENTED_EDGE ( 'NONE', *, *, #59632, .T. ) ;
#19025 = LINE ( 'NONE', #58974, #105726 ) ;
#19027 = EDGE_LOOP ( 'NONE', ( #97000, #54917 ) ) ;
#19026 = ORIENTED_EDGE ( 'NONE', *, *, #16544, .F. ) ;
#19028 = EDGE_LOOP ( 'NONE', ( #25520, #70327 ) ) ;
#19029 = FACE_OUTER_BOUND ( 'NONE', #16467, .T. ) ;
#19030 = AXIS2_PLACEMENT_3D ( 'NONE', #84817, #45560, #95295 ) ;
#19031 = DIRECTION ( 'NONE',  ( 0.000000000000000000, -0.9999939076577903929, 0.003490651415223739937 ) ) ;
#19032 = DIRECTION ( 'NONE',  ( 0.000000000000000000, -0.000000000000000000, 1.000000000000000000 ) ) ;
#19033 = LINE ( 'NONE', #70732, #74478 ) ;
#19034 = CONICAL_SURFACE ( 'NONE', #117224, 0.1000000000000002554, 0.003490658503988666988 ) ;
#19035 = AXIS2_PLACEMENT_3D ( 'NONE', #42424, #82353, #32625 ) ;
#19036 = DIRECTION ( 'NONE',  ( -0.000000000000000000, -1.000000000000000000, -0.000000000000000000 ) ) ;
#19037 = DIRECTION ( 'NONE',  ( -4.274815082592931898E-19, -0.9999939076577903929, -0.003490651415223739937 ) ) ;
#19038 = DIRECTION ( 'NONE',  ( 0.000000000000000000, 0.000000000000000000, 1.000000000000000000 ) ) ;
#19039 = CARTESIAN_POINT ( 'NONE',  ( 10.39999999999991154, 2.500000000000000000, 5.022947341949748790 ) ) ;
#19040 = VERTEX_POINT ( 'NONE', #99191 ) ;
#19041 = ORIENTED_EDGE ( 'NONE', *, *, #49397, .T. ) ;
#19042 = DIRECTION ( 'NONE',  ( 0.000000000000000000, 0.000000000000000000, -1.000000000000000000 ) ) ;
#19043 = ORIENTED_EDGE ( 'NONE', *, *, #59802, .T. ) ;
#19044 = VERTEX_POINT ( 'NONE', #108977 ) ;
#19045 = DIRECTION ( 'NONE',  ( -0.000000000000000000, -1.000000000000000000, -0.000000000000000000 ) ) ;
#19046 = EDGE_CURVE ( 'NONE', #60091, #57903, #27862, .T. ) ;
#19047 = FACE_OUTER_BOUND ( 'NONE', #61451, .T. ) ;
#19048 = CARTESIAN_POINT ( 'NONE',  ( -2.900000000000029665, 12.50000000000000000, 3.637306695894644726 ) ) ;
#19049 = DIRECTION ( 'NONE',  ( 0.000000000000000000, 0.000000000000000000, 1.000000000000000000 ) ) ;
#19050 = AXIS2_PLACEMENT_3D ( 'NONE', #34047, #92310, #84430 ) ;
#19051 = CARTESIAN_POINT ( 'NONE',  ( -4.600000000000024514, 2.500000000000000000, 3.737306695894644371 ) ) ;
#19052 = ORIENTED_EDGE ( 'NONE', *, *, #83850, .F. ) ;
#19053 = CONICAL_SURFACE ( 'NONE', #104828, 0.09999999999999999167, 0.003490658503988666988 ) ;
#19054 = ORIENTED_EDGE ( 'NONE', *, *, #44438, .T. ) ;
#19055 = CARTESIAN_POINT ( 'NONE',  ( 5.399999999999936406, 2.500000000000000000, -5.022947341949754119 ) ) ;
#19056 = AXIS2_PLACEMENT_3D ( 'NONE', #75297, #68055, #115194 ) ;
#19057 = ORIENTED_EDGE ( 'NONE', *, *, #61655, .T. ) ;
#19058 = CARTESIAN_POINT ( 'NONE',  ( 6.049999999999934097, 2.500000000000000000, 6.148780366869520897 ) ) ;
#19059 = ORIENTED_EDGE ( 'NONE', *, *, #48590, .F. ) ;
#19061 = ADVANCED_FACE ( 'NONE', ( #59282 ), #79547, .T. ) ;
#19060 = AXIS2_PLACEMENT_3D ( 'NONE', #19873, #59826, #67010 ) ;
#19062 = ADVANCED_FACE ( 'NONE', ( #80195 ), #38343, .T. ) ;
#19063 = ORIENTED_EDGE ( 'NONE', *, *, #107956, .F. ) ;
#19064 = DIRECTION ( 'NONE',  ( 0.000000000000000000, 0.000000000000000000, 1.000000000000000000 ) ) ;
#19065 = DIRECTION ( 'NONE',  ( 0.000000000000000000, 0.000000000000000000, -1.000000000000000000 ) ) ;
#19066 = DIRECTION ( 'NONE',  ( 0.000000000000000000, 1.000000000000000000, 0.000000000000000000 ) ) ;
#19067 = CARTESIAN_POINT ( 'NONE',  ( 3.549999999999944755, 2.500000000000000000, -6.841600689897077814 ) ) ;
#19068 = B_SPLINE_CURVE_WITH_KNOTS ( 'NONE', 3,
 ( #126626, #117404, #116140, #16637, #27758, #67681, #17946, #97795, #48065, #87952, #28424, #108257, #20535, #80750, #38914, #60477, #59179, #69624, #40178, #99099, #49368, #50628, #99745, #90550, #58537, #9422, #113247, #888, #40837, #8750, #88623, #81397, #120022, #10065, #50012, #19894, #120666, #31019, #98423, #70921 ),
 .UNSPECIFIED., .F., .F.,
 ( 4, 2, 2, 2, 2, 2, 2, 2, 2, 2, 2, 2, 2, 2, 2, 2, 2, 2, 2, 4 ),
 ( 0.000000000000000000, 0.0009998201928524694596, 0.001999640385704938919, 0.002999460578557408812, 0.003999280771409877838, 0.004999100964262348165, 0.005998921157114817625, 0.006998741349967286217, 0.007998561542819755676, 0.008498471639245989973, 0.008998381735672226003, 0.009498291832098460299, 0.009998201928524696330, 0.01099802212137718053, 0.01199784231422966647, 0.01299766250708215241, 0.01399748269993463662, 0.01449739279636087959, 0.01499730289278712082, 0.01599712308563960503 ),
 .UNSPECIFIED. ) ;
#19069 = LINE ( 'NONE', #46614, #61695 ) ;
#19070 = ORIENTED_EDGE ( 'NONE', *, *, #28557, .F. ) ;
#19071 = CARTESIAN_POINT ( 'NONE',  ( -0.8500000000000386136, 2.500000000000000000, 7.088010851410848190 ) ) ;
#19072 = LINE ( 'NONE', #78680, #28600 ) ;
#19073 = EDGE_CURVE ( 'NONE', #125678, #72018, #13231, .T. ) ;
#19074 = LINE ( 'NONE', #38770, #62551 ) ;
#19075 = PLANE ( 'NONE',  #15857 ) ;
#19076 = CARTESIAN_POINT ( 'NONE',  ( 1.899999999999949507, 2.500000000000000000, 3.983716857408420964 ) ) ;
#19077 = ORIENTED_EDGE ( 'NONE', *, *, #62084, .F. ) ;
#19078 = ORIENTED_EDGE ( 'NONE', *, *, #116288, .T. ) ;
#19079 = DIRECTION ( 'NONE',  ( 0.000000000000000000, 0.000000000000000000, 1.000000000000000000 ) ) ;
#19080 = ORIENTED_EDGE ( 'NONE', *, *, #94206, .F. ) ;
#19081 = DIRECTION ( 'NONE',  ( 0.000000000000000000, 0.000000000000000000, 1.000000000000000000 ) ) ;
#19082 = DIRECTION ( 'NONE',  ( 0.000000000000000000, 1.000000000000000000, 0.000000000000000000 ) ) ;
#19083 = CIRCLE ( 'NONE', #79750, 0.06509327318403745899 ) ;
#19084 = VERTEX_POINT ( 'NONE', #110287 ) ;
#19085 = DIRECTION ( 'NONE',  ( 0.000000000000000000, 0.000000000000000000, 1.000000000000000000 ) ) ;
#19086 = DIRECTION ( 'NONE',  ( -0.000000000000000000, -1.000000000000000000, -0.000000000000000000 ) ) ;
#19087 = CARTESIAN_POINT ( 'NONE',  ( 108.0000000000000142, 8.500000000000000000, 0.000000000000000000 ) ) ;
#19088 = CARTESIAN_POINT ( 'NONE',  ( 5.399999999999935518, 2.500000000000000000, -4.230127018922201998 ) ) ;
#19089 = ORIENTED_EDGE ( 'NONE', *, *, #114552, .F. ) ;
#19090 = AXIS2_PLACEMENT_3D ( 'NONE', #90261, #39911, #37958 ) ;
#19091 = EDGE_CURVE ( 'NONE', #53683, #107604, #38404, .T. ) ;
#19092 = CARTESIAN_POINT ( 'NONE',  ( -2.300000000000033129, 2.500000000000000000, 4.083716857408420609 ) ) ;
#19093 = ORIENTED_EDGE ( 'NONE', *, *, #31860, .T. ) ;
#19094 = EDGE_CURVE ( 'NONE', #97989, #106677, #78272, .T. ) ;
#19095 = CARTESIAN_POINT ( 'NONE',  ( 4.399999999999937295, 2.500000000000000000, 4.676537180435972552 ) ) ;
#19096 = DIRECTION ( 'NONE',  ( 0.000000000000000000, 0.000000000000000000, -1.000000000000000000 ) ) ;
#19097 = EDGE_CURVE ( 'NONE', #84309, #89637, #97242, .T. ) ;
#19098 = DIRECTION ( 'NONE',  ( 0.000000000000000000, 0.000000000000000000, 1.000000000000000000 ) ) ;
#19099 = CIRCLE ( 'NONE', #23231, 0.1000000000000002554 ) ;
#19100 = PRODUCT_DEFINITION_FORMATION_WITH_SPECIFIED_SOURCE ( 'ANY', '', #126727, .NOT_KNOWN. ) ;
#19101 = EDGE_LOOP ( 'NONE', ( #29070, #122977, #50999, #2205 ) ) ;
#19102 = CARTESIAN_POINT ( 'NONE',  ( 3.349999999999944578, 2.500000000000000000, -5.702370205355749455 ) ) ;
#19103 = AXIS2_PLACEMENT_3D ( 'NONE', #74974, #55966, #15383 ) ;
#19104 = EDGE_CURVE ( 'NONE', #77225, #1350, #23723, .T. ) ;
#19105 = EDGE_CURVE ( 'NONE', #10534, #14739, #32145, .T. ) ;
#19106 = VERTEX_POINT ( 'NONE', #19316 ) ;
#19107 = DIRECTION ( 'NONE',  ( 0.000000000000000000, 0.000000000000000000, 1.000000000000000000 ) ) ;
#19108 = DIRECTION ( 'NONE',  ( 0.000000000000000000, 0.000000000000000000, 1.000000000000000000 ) ) ;
#19109 = ADVANCED_FACE ( 'NONE', ( #128675 ), #69675, .T. ) ;
#19110 = CONICAL_SURFACE ( 'NONE', #94432, 0.1000000000000000472, 0.003490658503988666988 ) ;
#19111 = FACE_OUTER_BOUND ( 'NONE', #80237, .T. ) ;
#19112 = ORIENTED_EDGE ( 'NONE', *, *, #116504, .F. ) ;
#19113 = DIRECTION ( 'NONE',  ( 0.000000000000000000, 0.000000000000000000, 1.000000000000000000 ) ) ;
#19114 = ADVANCED_FACE ( 'NONE', ( #39008 ), #90598, .T. ) ;
#19115 = DIRECTION ( 'NONE',  ( 0.000000000000000000, 1.000000000000000000, 0.000000000000000000 ) ) ;
#19116 = CIRCLE ( 'NONE', #109008, 0.1000000000000002554 ) ;
#19117 = CIRCLE ( 'NONE', #48392, 0.06509327318403745899 ) ;
#19118 = ORIENTED_EDGE ( 'NONE', *, *, #60247, .F. ) ;
#19119 = CARTESIAN_POINT ( 'NONE',  ( -8.350000000000013856, 2.500000000000000000, -7.188010851410848723 ) ) ;
#19120 = EDGE_LOOP ( 'NONE', ( #43335, #59011, #69081, #20477 ) ) ;
#19121 = ADVANCED_FACE ( 'NONE', ( #9514 ), #9135, .T. ) ;
#19122 = DIRECTION ( 'NONE',  ( 0.000000000000000000, 0.000000000000000000, 1.000000000000000000 ) ) ;
#19123 = ORIENTED_EDGE ( 'NONE', *, *, #103812, .F. ) ;
#19124 = FACE_OUTER_BOUND ( 'NONE', #85159, .T. ) ;
#19125 = PLANE ( 'NONE',  #49998 ) ;
#19126 = ORIENTED_EDGE ( 'NONE', *, *, #38452, .T. ) ;
#19127 = VERTEX_POINT ( 'NONE', #80841 ) ;
#19128 = CARTESIAN_POINT ( 'NONE',  ( -7.050000000000016698, 2.500000000000000000, -6.595190528383302109 ) ) ;
#19129 = DIRECTION ( 'NONE',  ( -0.000000000000000000, -1.000000000000000000, -0.000000000000000000 ) ) ;
#19130 = ORIENTED_EDGE ( 'NONE', *, *, #111194, .T. ) ;
#19131 = CARTESIAN_POINT ( 'NONE',  ( 185.6249999999999716, -8.891194145520236347, -1.633285867636356299E-15 ) ) ;
#19132 = PLANE ( 'NONE',  #1177 ) ;
#19133 = DIRECTION ( 'NONE',  ( -0.000000000000000000, -1.000000000000000000, -0.000000000000000000 ) ) ;
#19134 = VECTOR ( 'NONE', #22225, 1000.000000000000000 ) ;
#19135 = CARTESIAN_POINT ( 'NONE',  ( 103.1653408115099211, 8.605869126093731225, -1.317692694826197775 ) ) ;
#19136 = CARTESIAN_POINT ( 'NONE',  ( -4.600000000000028955, 2.500000000000000000, -4.230127018922201998 ) ) ;
#19137 = VECTOR ( 'NONE', #95398, 1000.000000000000000 ) ;
#19138 = AXIS2_PLACEMENT_3D ( 'NONE', #23097, #124530, #103602 ) ;
#19139 = LINE ( 'NONE', #97082, #41076 ) ;
#19140 = DIRECTION ( 'NONE',  ( 0.000000000000000000, 0.000000000000000000, -1.000000000000000000 ) ) ;
#19141 = CONICAL_SURFACE ( 'NONE', #90252, 0.09999999999999982514, 0.003490658503988666988 ) ;
#19142 = ORIENTED_EDGE ( 'NONE', *, *, #104767, .F. ) ;
#19144 = ORIENTED_EDGE ( 'NONE', *, *, #110163, .F. ) ;
#19143 = AXIS2_PLACEMENT_3D ( 'NONE', #81515, #99869, #10194 ) ;
#19145 = VERTEX_POINT ( 'NONE', #23188 ) ;
#19146 = VERTEX_POINT ( 'NONE', #101115 ) ;
#19147 = CARTESIAN_POINT ( 'NONE',  ( 14.54999999999989591, 2.500000000000000000, 2.065063509461097624 ) ) ;
#19148 = DIRECTION ( 'NONE',  ( 0.000000000000000000, -0.000000000000000000, 1.000000000000000000 ) ) ;
#19149 = VECTOR ( 'NONE', #80216, 1000.000000000000000 ) ;
#19150 = DIRECTION ( 'NONE',  ( 0.000000000000000000, 1.000000000000000000, 0.000000000000000000 ) ) ;
#19151 = ORIENTED_EDGE ( 'NONE', *, *, #43972, .T. ) ;
#19152 = FACE_BOUND ( 'NONE', #75832, .T. ) ;
#19153 = ORIENTED_EDGE ( 'NONE', *, *, #56398, .F. ) ;
#19154 = CARTESIAN_POINT ( 'NONE',  ( -5.000000000000022204, 2.500000000000000000, -0.7928203230275542301 ) ) ;
#19155 = PLANE ( 'NONE',  #5987 ) ;
#19156 = AXIS2_PLACEMENT_3D ( 'NONE', #62000, #22081, #52807 ) ;
#19157 = CARTESIAN_POINT ( 'NONE',  ( 7.499999999999925393, 12.50000000000000000, -3.637306695894650055 ) ) ;
#19158 = EDGE_CURVE ( 'NONE', #12823, #31364, #115732, .T. ) ;
#19159 = DIRECTION ( 'NONE',  ( 0.000000000000000000, 0.000000000000000000, 1.000000000000000000 ) ) ;
#19160 = CARTESIAN_POINT ( 'NONE',  ( 1.649999999999949729, 2.500000000000000000, 5.702370205355745014 ) ) ;
#19161 = CARTESIAN_POINT ( 'NONE',  ( 184.5000000000000000, 0.000000000000000000, 0.000000000000000000 ) ) ;
#19162 = DIRECTION ( 'NONE',  ( -0.000000000000000000, 1.000000000000000000, -0.000000000000000000 ) ) ;
#19163 = CARTESIAN_POINT ( 'NONE',  ( 14.14999999999989733, 12.50000000000000000, 1.537336459617582918 ) ) ;
#19164 = CARTESIAN_POINT ( 'NONE',  ( -7.300000000000018474, 2.500000000000000000, 0.4464101615137735513 ) ) ;
#19165 = DIRECTION ( 'NONE',  ( 0.000000000000000000, 0.000000000000000000, 1.000000000000000000 ) ) ;
#19166 = EDGE_CURVE ( 'NONE', #87864, #69735, #59338, .T. ) ;
#19167 = EDGE_LOOP ( 'NONE', ( #69551, #93479 ) ) ;
#19168 = ORIENTED_EDGE ( 'NONE', *, *, #74978, .T. ) ;
#19169 = ORIENTED_EDGE ( 'NONE', *, *, #102173, .T. ) ;
#19170 = ORIENTED_EDGE ( 'NONE', *, *, #19073, .F. ) ;
#19171 = CARTESIAN_POINT ( 'NONE',  ( 16.89179977596573323, -0.9177129796144657403, -5.694535519821270597 ) ) ;
#19172 = CARTESIAN_POINT ( 'NONE',  ( -12.09999999999999609, 12.50000000000000000, 1.734723475976807094E-15 ) ) ;
#19173 = UNCERTAINTY_MEASURE_WITH_UNIT (LENGTH_MEASURE( 1.000000000000000082E-05 ), #127086, 'distance_accuracy_value', 'NONE');
#19175 = EDGE_LOOP ( 'NONE', ( #26062, #113461 ) ) ;
#19174 = ORIENTED_EDGE ( 'NONE', *, *, #61461, .F. ) ;
#19176 = VERTEX_POINT ( 'NONE', #52648 ) ;
#19177 = DIRECTION ( 'NONE',  ( 0.000000000000000000, 0.000000000000000000, 1.000000000000000000 ) ) ;
#19178 = CIRCLE ( 'NONE', #29670, 0.06509327318403741736 ) ;
#19179 = CONICAL_SURFACE ( 'NONE', #92348, 0.1000000000000002554, 0.003490658503988666988 ) ;
#19180 = DIRECTION ( 'NONE',  ( 0.000000000000000000, -0.9999939076577903929, 0.003490651415223739937 ) ) ;
#19181 = CARTESIAN_POINT ( 'NONE',  ( -6.250000000000015987, 12.50000000000000000, 5.802370205355744659 ) ) ;
#19182 = CARTESIAN_POINT ( 'NONE',  ( -9.600000000000008527, 2.500000000000000000, -5.022947341949749678 ) ) ;
#19183 = CARTESIAN_POINT ( 'NONE',  ( 3.749999999999940492, 12.50000000000000000, 5.802370205355744659 ) ) ;
#19184 = CARTESIAN_POINT ( 'NONE',  ( 11.84999999999990372, 2.500000000000000000, -6.248780366869526759 ) ) ;
#19185 = CARTESIAN_POINT ( 'NONE',  ( -15.59999999999998010, 2.500000000000000000, -0.4464101615137759382 ) ) ;
#19186 = ORIENTED_EDGE ( 'NONE', *, *, #80038, .F. ) ;
#19187 = CIRCLE ( 'NONE', #117461, 0.1000000000000002554 ) ;
#19188 = CONICAL_SURFACE ( 'NONE', #8724, 0.1000000000000002554, 0.003490658503988666988 ) ;
#19189 = CARTESIAN_POINT ( 'NONE',  ( 11.84999999999990372, 12.50000000000000000, 2.511473670974873507 ) ) ;
#19190 = EDGE_LOOP ( 'NONE', ( #59348, #47705, #77584, #95564 ) ) ;
#19191 = CIRCLE ( 'NONE', #92357, 0.09999999999999982514 ) ;
#19192 = EDGE_LOOP ( 'NONE', ( #100633, #36353 ) ) ;
#19193 = CIRCLE ( 'NONE', #12934, 0.06509327318403745899 ) ;
#19194 = ORIENTED_EDGE ( 'NONE', *, *, #107649, .T. ) ;
#19195 = VECTOR ( 'NONE', #52506, 1000.000000000000000 ) ;
#19196 = CARTESIAN_POINT ( 'NONE',  ( -0.4500000000000402012, 12.50000000000000000, 6.495190528383297135 ) ) ;
#19197 =( BOUNDED_CURVE ( )  B_SPLINE_CURVE ( 2, ( #20877, #10404, #90898, #61462, #50336, #49709, #100708 ),
 .UNSPECIFIED., .F., .F. ) 
 B_SPLINE_CURVE_WITH_KNOTS ( ( 3, 2, 2, 3 ),
 ( 0.2857142857142859760, 0.3095238095238098119, 0.3333333333333335924, 0.3571428571428574283 ),
 .UNSPECIFIED. ) 
 CURVE ( )  GEOMETRIC_REPRESENTATION_ITEM ( )  RATIONAL_B_SPLINE_CURVE ( ( 0.9999999999999984457, 0.8660254037844402619, 1.000000000000000000, 0.8660254037844387076, 1.000000000000000000, 0.8660254037844371533, 1.000000000000001554 ) ) 
 REPRESENTATION_ITEM ( '' )  );
#19198 = VERTEX_POINT ( 'NONE', #121392 ) ;
#19199 = ORIENTED_EDGE ( 'NONE', *, *, #70323, .T. ) ;
#19200 = CONICAL_SURFACE ( 'NONE', #46307, 0.09999999999999999167, 0.003490658503988666988 ) ;
#19201 = DIRECTION ( 'NONE',  ( 0.000000000000000000, 0.000000000000000000, 1.000000000000000000 ) ) ;
#19202 = CONICAL_SURFACE ( 'NONE', #58940, 0.1000000000000002554, 0.003490658503988666988 ) ;
#19203 = EDGE_CURVE ( 'NONE', #100401, #20290, #2250, .T. ) ;
#19204 = CARTESIAN_POINT ( 'NONE',  ( -2.900000000000029665, 12.50000000000000000, 4.395220292106234439 ) ) ;
#19205 = DIRECTION ( 'NONE',  ( -1.000000000000000000, 0.000000000000000000, 1.224646799147352221E-16 ) ) ;
#19206 = CARTESIAN_POINT ( 'NONE',  ( -1.650000000000034328, 2.500000000000000000, -7.188010851410854052 ) ) ;
#19207 = VECTOR ( 'NONE', #74861, 1000.000000000000000 ) ;
#19208 = AXIS2_PLACEMENT_3D ( 'NONE', #44663, #114051, #63668 ) ;
#19209 = CIRCLE ( 'NONE', #115642, 0.06509327318403745899 ) ;
#19210 = DIRECTION ( 'NONE',  ( -1.000000000000000000, -0.000000000000000000, -0.000000000000000000 ) ) ;
#19211 = CONICAL_SURFACE ( 'NONE', #65279, 0.1000000000000000472, 0.003490658503988666988 ) ;
#19212 = ORIENTED_EDGE ( 'NONE', *, *, #95301, .T. ) ;
#19213 = DIRECTION ( 'NONE',  ( -0.000000000000000000, 1.000000000000000000, -0.000000000000000000 ) ) ;
#19214 = EDGE_CURVE ( 'NONE', #60736, #124494, #122686, .T. ) ;
#19215 = EDGE_LOOP ( 'NONE', ( #82591, #124154 ) ) ;
#19216 = DIRECTION ( 'NONE',  ( 0.000000000000000000, 0.000000000000000000, -1.000000000000000000 ) ) ;
#19217 = ORIENTED_EDGE ( 'NONE', *, *, #87183, .T. ) ;
#19218 = CARTESIAN_POINT ( 'NONE',  ( 5.849999999999934808, 2.500000000000000000, -5.802370205355749988 ) ) ;
#19219 = AXIS2_PLACEMENT_3D ( 'NONE', #86449, #53776, #85804 ) ;
#19220 = DIRECTION ( 'NONE',  ( 0.000000000000000000, 0.000000000000000000, -1.000000000000000000 ) ) ;
#19221 = ORIENTED_EDGE ( 'NONE', *, *, #42360, .F. ) ;
#19223 = EDGE_CURVE ( 'NONE', #52767, #20628, #110917, .T. ) ;
#19222 = PLANE ( 'NONE',  #63419 ) ;
#19224 = DIRECTION ( 'NONE',  ( 0.000000000000000000, -0.9999939076577903929, 0.003490651415223739937 ) ) ;
#19225 = EDGE_CURVE ( 'NONE', #88967, #112846, #92585, .T. ) ;
#19226 = ORIENTED_EDGE ( 'NONE', *, *, #120792, .T. ) ;
#19227 = EDGE_CURVE ( 'NONE', #81889, #55268, #123333, .T. ) ;
#19228 = FACE_OUTER_BOUND ( 'NONE', #4870, .T. ) ;
#19229 = ORIENTED_EDGE ( 'NONE', *, *, #127851, .F. ) ;
#19230 = VERTEX_POINT ( 'NONE', #51392 ) ;
#19231 = DIRECTION ( 'NONE',  ( 0.000000000000000000, 0.000000000000000000, 1.000000000000000000 ) ) ;
#19232 = DIRECTION ( 'NONE',  ( 0.000000000000000000, 0.000000000000000000, 1.000000000000000000 ) ) ;
#19233 = EDGE_CURVE ( 'NONE', #77871, #15508, #82118, .T. ) ;
#19234 = FACE_OUTER_BOUND ( 'NONE', #1926, .T. ) ;
#19235 = DIRECTION ( 'NONE',  ( 0.000000000000000000, 1.000000000000000000, 0.000000000000000000 ) ) ;
#19236 = LINE ( 'NONE', #248, #116840 ) ;
#19237 = ORIENTED_EDGE ( 'NONE', *, *, #2018, .F. ) ;
#19238 = CARTESIAN_POINT ( 'NONE',  ( -4.150000000000025224, 2.500000000000000000, 2.757883832488649656 ) ) ;
#19239 = CIRCLE ( 'NONE', #123784, 0.06509327318403745899 ) ;
#19240 = AXIS2_PLACEMENT_3D ( 'NONE', #122439, #35346, #13745 ) ;
#19241 = ORIENTED_EDGE ( 'NONE', *, *, #20031, .F. ) ;
#19242 = CARTESIAN_POINT ( 'NONE',  ( -3.550000000000028244, 12.50000000000000000, -1.883746621131363597 ) ) ;
#19243 = CARTESIAN_POINT ( 'NONE',  ( 7.949999999999922018, 12.50000000000000000, -2.230156782645139391 ) ) ;
#19244 = AXIS2_PLACEMENT_3D ( 'NONE', #55206, #54531, #4782 ) ;
#19245 = CIRCLE ( 'NONE', #92412, 0.1000000000000000472 ) ;
#19246 = CIRCLE ( 'NONE', #113340, 0.06509327318403745899 ) ;
#19247 = AXIS2_PLACEMENT_3D ( 'NONE', #97113, #29036, #27720 ) ;
#19248 = AXIS2_PLACEMENT_3D ( 'NONE', #127157, #117284, #55186 ) ;
#19249 = CARTESIAN_POINT ( 'NONE',  ( 0.1999999999999636513, 2.500000000000000000, -0.2464101615137760659 ) ) ;
#19250 = DIRECTION ( 'NONE',  ( 0.000000000000000000, 1.000000000000000000, 0.000000000000000000 ) ) ;
#19251 = LINE ( 'NONE', #59215, #63205 ) ;
#19252 = DIRECTION ( 'NONE',  ( 0.000000000000000000, 1.000000000000000000, 0.000000000000000000 ) ) ;
#19253 = DIRECTION ( 'NONE',  ( 0.000000000000000000, 0.000000000000000000, 1.000000000000000000 ) ) ;
#19254 = ORIENTED_EDGE ( 'NONE', *, *, #57822, .T. ) ;
#19255 = AXIS2_PLACEMENT_3D ( 'NONE', #84924, #16798, #44349 ) ;
#19256 = CARTESIAN_POINT ( 'NONE',  ( 184.3333333333333144, 6.668395609140177704, -3.849999999999998312 ) ) ;
#19257 = DIRECTION ( 'NONE',  ( 0.000000000000000000, -0.9999939076577903929, 0.003490651415223739937 ) ) ;
#19258 = FILL_AREA_STYLE ('',( #127308 ) ) ;
#19259 = ORIENTED_EDGE ( 'NONE', *, *, #18960, .F. ) ;
#19260 = EDGE_CURVE ( 'NONE', #84685, #14124, #25863, .T. ) ;
#19261 = DIRECTION ( 'NONE',  ( 0.000000000000000000, -0.9999939076577903929, 0.003490651415223739937 ) ) ;
#19262 = ORIENTED_EDGE ( 'NONE', *, *, #75531, .F. ) ;
#19263 = ORIENTED_EDGE ( 'NONE', *, *, #217, .T. ) ;
#19264 = CARTESIAN_POINT ( 'NONE',  ( -12.94999999999999218, 2.500000000000000000, -2.265063509461099578 ) ) ;
#19265 = EDGE_CURVE ( 'NONE', #107104, #14028, #50911, .T. ) ;
#19266 = EDGE_CURVE ( 'NONE', #57219, #114003, #126111, .T. ) ;
#19267 = VERTEX_POINT ( 'NONE', #42870 ) ;
#19268 = CARTESIAN_POINT ( 'NONE',  ( 7.699999999999923794, 2.500000000000000000, -0.3464101615137783474 ) ) ;
#19270 = EDGE_CURVE ( 'NONE', #54425, #41455, #41572, .T. ) ;
#19269 = CARTESIAN_POINT ( 'NONE',  ( -7.900000000000014566, 2.500000000000000000, 0.5928203230275495006 ) ) ;
#19271 = EDGE_CURVE ( 'NONE', #113210, #19759, #109483, .T. ) ;
#19272 = VECTOR ( 'NONE', #69817, 1000.000000000000000 ) ;
#19273 = VERTEX_POINT ( 'NONE', #31731 ) ;
#19274 = CARTESIAN_POINT ( 'NONE',  ( 8.949999999999921130, 12.50000000000000000, -6.841600689897078702 ) ) ;
#19275 = ADVANCED_FACE ( 'NONE', ( #71652 ), #33040, .T. ) ;
#19277 = ORIENTED_EDGE ( 'NONE', *, *, #13971, .T. ) ;
#19276 = CARTESIAN_POINT ( 'NONE',  ( 4.599999999999935696, 2.500000000000000000, 4.922947341949748257 ) ) ;
#19278 = CARTESIAN_POINT ( 'NONE',  ( 13.94999999999989804, 2.500000000000000000, 1.818653347947321475 ) ) ;
#19279 = DIRECTION ( 'NONE',  ( 0.000000000000000000, 1.000000000000000000, 0.000000000000000000 ) ) ;
#19280 = CIRCLE ( 'NONE', #107113, 0.09999999999999999167 ) ;
#19281 = ORIENTED_EDGE ( 'NONE', *, *, #120745, .T. ) ;
#19282 = AXIS2_PLACEMENT_3D ( 'NONE', #128565, #66386, #76861 ) ;
#19283 = ADVANCED_FACE ( 'NONE', ( #22578 ), #46697, .T. ) ;
#19284 = CIRCLE ( 'NONE', #44436, 0.06509327318403741736 ) ;
#19285 = EDGE_CURVE ( 'NONE', #95487, #79569, #86393, .T. ) ;
#19286 = CONICAL_SURFACE ( 'NONE', #6749, 0.1000000000000002554, 0.003490658503988666988 ) ;
#19287 = ORIENTED_EDGE ( 'NONE', *, *, #101124, .F. ) ;
#19288 = ORIENTED_EDGE ( 'NONE', *, *, #123934, .T. ) ;
#19289 = CARTESIAN_POINT ( 'NONE',  ( 9.799999999999913669, 2.500000000000000000, 4.576537180435972019 ) ) ;
#19290 = DIRECTION ( 'NONE',  ( 0.000000000000000000, 0.000000000000000000, -1.000000000000000000 ) ) ;
#19291 = CARTESIAN_POINT ( 'NONE',  ( 5.199999999999931788, 2.500000000000000000, 4.576537180435972019 ) ) ;
#19292 = FACE_BOUND ( 'NONE', #113965, .T. ) ;
#19293 = ORIENTED_EDGE ( 'NONE', *, *, #13608, .T. ) ;
#19294 = DIRECTION ( 'NONE',  ( -4.274815082592931898E-19, -0.9999939076577903929, -0.003490651415223739937 ) ) ;
#19295 = DIRECTION ( 'NONE',  ( 0.000000000000000000, 0.000000000000000000, -1.000000000000000000 ) ) ;
#19296 = CONICAL_SURFACE ( 'NONE', #17125, 0.1000000000000000472, 0.003490658503988666988 ) ;
#19297 = ORIENTED_EDGE ( 'NONE', *, *, #94333, .F. ) ;
#19298 = DIRECTION ( 'NONE',  ( 0.000000000000000000, -0.9999939076577903929, 0.003490651415223739937 ) ) ;
#19299 = CARTESIAN_POINT ( 'NONE',  ( 17.45652781226509731, 2.453230724138542485, 4.494708854620872884 ) ) ;
#19300 = CIRCLE ( 'NONE', #79953, 0.06509327318403745899 ) ;
#19301 = CIRCLE ( 'NONE', #123860, 0.1000000000000002554 ) ;
#19302 = AXIS2_PLACEMENT_3D ( 'NONE', #7265, #86479, #47216 ) ;
#19303 = DIRECTION ( 'NONE',  ( -4.274815082592931898E-19, -0.9999939076577903929, -0.003490651415223739937 ) ) ;
#19304 = CARTESIAN_POINT ( 'NONE',  ( -6.900000000000019007, 12.50000000000000000, -3.983716857408426293 ) ) ;
#19305 = CARTESIAN_POINT ( 'NONE',  ( -8.350000000000012079, 2.500000000000000000, -2.957883832488653830 ) ) ;
#19306 = DIRECTION ( 'NONE',  ( 0.000000000000000000, 0.000000000000000000, 1.000000000000000000 ) ) ;
#19307 = VECTOR ( 'NONE', #62161, 1000.000000000000000 ) ;
#19308 = DIRECTION ( 'NONE',  ( 0.000000000000000000, 0.000000000000000000, -1.000000000000000000 ) ) ;
#19309 = VERTEX_POINT ( 'NONE', #3556 ) ;
#19310 = AXIS2_PLACEMENT_3D ( 'NONE', #45748, #46369, #33367 ) ;
#19311 = ORIENTED_EDGE ( 'NONE', *, *, #30963, .T. ) ;
#19312 = ORIENTED_EDGE ( 'NONE', *, *, #118379, .F. ) ;
#19313 = ORIENTED_EDGE ( 'NONE', *, *, #67618, .T. ) ;
#19314 = ORIENTED_EDGE ( 'NONE', *, *, #103584, .T. ) ;
#19315 = CARTESIAN_POINT ( 'NONE',  ( -8.350000000000008527, 2.500000000000000000, 5.702370205355745014 ) ) ;
#19316 = CARTESIAN_POINT ( 'NONE',  ( -10.65000000000000391, 2.500000000000000000, -1.918653347947322230 ) ) ;
#19317 = ORIENTED_EDGE ( 'NONE', *, *, #16120, .F. ) ;
#19318 = FACE_BOUND ( 'NONE', #71941, .T. ) ;
#19319 = CARTESIAN_POINT ( 'NONE',  ( 7.099999999999927702, 2.500000000000000000, -3.537306695894649966 ) ) ;
#19320 = DIRECTION ( 'NONE',  ( 0.000000000000000000, 1.000000000000000000, 0.000000000000000000 ) ) ;
#19321 = CARTESIAN_POINT ( 'NONE',  ( 2.299999999999948752, 12.50000000000000000, -3.983716857408426293 ) ) ;
#19322 = FACE_OUTER_BOUND ( 'NONE', #85181, .T. ) ;
#19323 = CARTESIAN_POINT ( 'NONE',  ( -4.400000000000025224, 2.500000000000000000, 3.983716857408420076 ) ) ;
#19324 = AXIS2_PLACEMENT_3D ( 'NONE', #18447, #68834, #108749 ) ;
#19325 = CARTESIAN_POINT ( 'NONE',  ( 0.3999999999999555023, 2.500000000000000000, 4.330127018922196314 ) ) ;
#19326 = ORIENTED_EDGE ( 'NONE', *, *, #40152, .F. ) ;
#19327 = ORIENTED_EDGE ( 'NONE', *, *, #67334, .T. ) ;
#19328 = EDGE_CURVE ( 'NONE', #24109, #71913, #32406, .T. ) ;
#19329 = EDGE_LOOP ( 'NONE', ( #82085, #28850 ) ) ;
#19330 = AXIS2_PLACEMENT_3D ( 'NONE', #46195, #75644, #17360 ) ;
#19331 = EDGE_LOOP ( 'NONE', ( #43766, #98215 ) ) ;
#19332 = CONICAL_SURFACE ( 'NONE', #29819, 0.1000000000000000472, 0.003490658503988666988 ) ;
#19333 = VECTOR ( 'NONE', #17616, 1000.000000000000000 ) ;
#19334 = CARTESIAN_POINT ( 'NONE',  ( 10.84999999999990905, 12.50000000000000000, -6.495190528383302464 ) ) ;
#19335 = DIRECTION ( 'NONE',  ( 0.000000000000000000, 1.000000000000000000, 0.000000000000000000 ) ) ;
#19336 = ORIENTED_EDGE ( 'NONE', *, *, #106012, .F. ) ;
#19337 = DIRECTION ( 'NONE',  ( 0.000000000000000000, 0.000000000000000000, -1.000000000000000000 ) ) ;
#19338 = LINE ( 'NONE', #27233, #17728 ) ;
#19339 = CIRCLE ( 'NONE', #113442, 0.06509327318403745899 ) ;
#19340 = CIRCLE ( 'NONE', #40297, 0.06509327318403745899 ) ;
#19341 = CIRCLE ( 'NONE', #15117, 0.06509327318403745899 ) ;
#19342 = CARTESIAN_POINT ( 'NONE',  ( -4.200000000000025935, 12.50000000000000000, 4.265033745738159077 ) ) ;
#19343 = CARTESIAN_POINT ( 'NONE',  ( 184.2343750003414016, 8.734944146203032389, 5.348610694689227483E-16 ) ) ;
#19344 = DIRECTION ( 'NONE',  ( 0.000000000000000000, 0.000000000000000000, -1.000000000000000000 ) ) ;
#19345 = CARTESIAN_POINT ( 'NONE',  ( 11.04999999999990656, 12.50000000000000000, -6.148780366869526226 ) ) ;
#19346 = CIRCLE ( 'NONE', #71684, 0.06509327318403745899 ) ;
#19347 = FACE_OUTER_BOUND ( 'NONE', #110322, .T. ) ;
#19348 = VERTEX_POINT ( 'NONE', #123964 ) ;
#19349 = CARTESIAN_POINT ( 'NONE',  ( -1.050000000000037348, 2.500000000000000000, -6.841600689897078702 ) ) ;
#19350 = CIRCLE ( 'NONE', #54958, 0.06509327318403745899 ) ;
#19351 = ORIENTED_EDGE ( 'NONE', *, *, #63764, .F. ) ;
#19352 = ORIENTED_EDGE ( 'NONE', *, *, #24449, .T. ) ;
#19353 = DIRECTION ( 'NONE',  ( 0.000000000000000000, 0.000000000000000000, 1.000000000000000000 ) ) ;
#19354 = CARTESIAN_POINT ( 'NONE',  ( 14.99999999999989342, 2.500000000000000000, -0.7928203230275542301 ) ) ;
#19355 = CARTESIAN_POINT ( 'NONE',  ( 12.89999999999990266, 2.500000000000000000, 4.922947341949748257 ) ) ;
#19356 = ORIENTED_EDGE ( 'NONE', *, *, #55873, .T. ) ;
#19357 = ORIENTED_EDGE ( 'NONE', *, *, #92082, .F. ) ;
#19358 = AXIS2_PLACEMENT_3D ( 'NONE', #96535, #27172, #120714 ) ;
#19359 = DIRECTION ( 'NONE',  ( 0.000000000000000000, 0.000000000000000000, -1.000000000000000000 ) ) ;
#19360 = CARTESIAN_POINT ( 'NONE',  ( -12.09999999999999432, 2.500000000000000000, 3.537306695894645081 ) ) ;
#19361 = DIRECTION ( 'NONE',  ( 1.000000000000000000, 0.000000000000000000, 0.000000000000000000 ) ) ;
#19362 = ORIENTED_EDGE ( 'NONE', *, *, #117460, .F. ) ;
#19363 = CARTESIAN_POINT ( 'NONE',  ( 8.349999999999923261, 2.500000000000000000, 2.857883832488649301 ) ) ;
#19365 = ORIENTED_EDGE ( 'NONE', *, *, #24125, .T. ) ;
#19364 = CIRCLE ( 'NONE', #2638, 0.09999999999999999167 ) ;
#19366 = CARTESIAN_POINT ( 'NONE',  ( -2.900000000000030553, 2.500000000000000000, 5.022947341949748790 ) ) ;
#19367 = AXIS2_PLACEMENT_3D ( 'NONE', #52013, #42860, #3545 ) ;
#19368 = EDGE_CURVE ( 'NONE', #54276, #9000, #46705, .T. ) ;
#19369 = COLOUR_RGB ( '', 0.72549020, 0.75294118, 0.79215686) ;
#19370 = EDGE_LOOP ( 'NONE', ( #82256, #106139, #122895, #41029 ) ) ;
#19371 = CARTESIAN_POINT ( 'NONE',  ( 186.5000000000000000, 0.000000000000000000, 7.700000000000000178 ) ) ;
#19372 = DIRECTION ( 'NONE',  ( 0.000000000000000000, 0.000000000000000000, 1.000000000000000000 ) ) ;
#19373 = CARTESIAN_POINT ( 'NONE',  ( -7.900000000000011013, 2.500000000000000000, 3.637306695894644726 ) ) ;
#19374 = ADVANCED_FACE ( 'NONE', ( #104334 ), #19699, .T. ) ;
#19376 = VECTOR ( 'NONE', #94305, 1000.000000000000000 ) ;
#19375 = DIRECTION ( 'NONE',  ( 0.000000000000000000, -0.000000000000000000, 1.000000000000000000 ) ) ;
#19377 = ADVANCED_FACE ( 'NONE', ( #86620 ), #103701, .T. ) ;
#19378 = VERTEX_POINT ( 'NONE', #16574 ) ;
#19379 = DIRECTION ( 'NONE',  ( 0.000000000000000000, 1.000000000000000000, 0.000000000000000000 ) ) ;
#19380 = AXIS2_PLACEMENT_3D ( 'NONE', #60499, #38938, #30400 ) ;
#19381 = EDGE_CURVE ( 'NONE', #22835, #59380, #4180, .T. ) ;
#19382 = ORIENTED_EDGE ( 'NONE', *, *, #118544, .T. ) ;
#19383 = EDGE_CURVE ( 'NONE', #117981, #27458, #21752, .T. ) ;
#19384 = VERTEX_POINT ( 'NONE', #56514 ) ;
#19385 = EDGE_CURVE ( 'NONE', #1350, #77225, #115832, .T. ) ;
#19386 = LINE ( 'NONE', #59352, #62533 ) ;
#19387 = CARTESIAN_POINT ( 'NONE',  ( 0.1999999999999562961, 12.50000000000000000, 4.741630453620009789 ) ) ;
#19388 = LINE ( 'NONE', #50172, #111783 ) ;
#19389 = EDGE_CURVE ( 'NONE', #34614, #15166, #114787, .T. ) ;
#19390 = CARTESIAN_POINT ( 'NONE',  ( 186.9427083336747160, -6.551208109652278289, 3.782341765624995134 ) ) ;
#19391 = AXIS2_PLACEMENT_3D ( 'NONE', #17675, #126355, #77881 ) ;
#19392 = DIRECTION ( 'NONE',  ( -0.000000000000000000, 1.000000000000000000, -0.000000000000000000 ) ) ;
#19393 = DIRECTION ( 'NONE',  ( 0.000000000000000000, 1.000000000000000000, 0.000000000000000000 ) ) ;
#19394 = AXIS2_PLACEMENT_3D ( 'NONE', #115901, #47178, #26888 ) ;
#19395 = DIRECTION ( 'NONE',  ( -0.000000000000000000, -1.000000000000000000, -0.000000000000000000 ) ) ;
#19396 = DIRECTION ( 'NONE',  ( 0.000000000000000000, -0.000000000000000000, 1.000000000000000000 ) ) ;
#19397 = AXIS2_PLACEMENT_3D ( 'NONE', #121448, #79137, #19552 ) ;
#19398 = VECTOR ( 'NONE', #18384, 1000.000000000000000 ) ;
#19399 = DIRECTION ( 'NONE',  ( 0.000000000000000000, -0.9999939076577903929, 0.003490651415223739937 ) ) ;
#19400 = EDGE_CURVE ( 'NONE', #114757, #57762, #24488, .T. ) ;
#19401 = AXIS2_PLACEMENT_3D ( 'NONE', #5772, #126869, #26096 ) ;
#19402 = CONICAL_SURFACE ( 'NONE', #11083, 0.1000000000000002554, 0.003490658503988666988 ) ;
#19403 = ORIENTED_EDGE ( 'NONE', *, *, #117219, .T. ) ;
#19404 = CYLINDRICAL_SURFACE ( 'NONE', #117385, 3.000000000000000000 ) ;
#19405 = CARTESIAN_POINT ( 'NONE',  ( 7.299999999999927880, 12.50000000000000000, 4.048810130592458201 ) ) ;
#19406 = DIRECTION ( 'NONE',  ( 0.000000000000000000, -0.9999939076577903929, 0.003490651415223739937 ) ) ;
#19407 = CARTESIAN_POINT ( 'NONE',  ( 9.149999999999916866, 2.500000000000000000, 7.188010851410848723 ) ) ;
#19408 = DIRECTION ( 'NONE',  ( 0.000000000000000000, 0.000000000000000000, 1.000000000000000000 ) ) ;
#19409 = VERTEX_POINT ( 'NONE', #14641 ) ;
#19410 = DIRECTION ( 'NONE',  ( 0.000000000000000000, 1.000000000000000000, 0.000000000000000000 ) ) ;
#19411 = CARTESIAN_POINT ( 'NONE',  ( 7.049999999999926992, 12.50000000000000000, 2.165063509461097713 ) ) ;
#19413 = EDGE_LOOP ( 'NONE', ( #85917, #84895 ) ) ;
#19412 = DIRECTION ( 'NONE',  ( 0.000000000000000000, 0.000000000000000000, -1.000000000000000000 ) ) ;
#19414 = CONICAL_SURFACE ( 'NONE', #92597, 0.09999999999999982514, 0.003490658503988666988 ) ;
#19416 = ADVANCED_FACE ( 'NONE', ( #54572 ), #64404, .T. ) ;
#19415 = AXIS2_PLACEMENT_3D ( 'NONE', #64810, #33442, #3318 ) ;
#19417 = VERTEX_POINT ( 'NONE', #53950 ) ;
#19418 = CARTESIAN_POINT ( 'NONE',  ( -5.200000000000025935, 12.50000000000000000, -4.048810130592463530 ) ) ;
#19419 = AXIS2_PLACEMENT_3D ( 'NONE', #64669, #65957, #85598 ) ;
#19420 = ORIENTED_EDGE ( 'NONE', *, *, #42036, .T. ) ;
#19421 = EDGE_LOOP ( 'NONE', ( #25905, #22781 ) ) ;
#19422 = VECTOR ( 'NONE', #51058, 1000.000000000000000 ) ;
#19423 = ORIENTED_EDGE ( 'NONE', *, *, #2357, .F. ) ;
#19424 = LINE ( 'NONE', #78379, #109317 ) ;
#19425 = AXIS2_PLACEMENT_3D ( 'NONE', #70550, #43063, #2441 ) ;
#19426 = AXIS2_PLACEMENT_3D ( 'NONE', #4897, #36964, #65105 ) ;
#19427 = EDGE_CURVE ( 'NONE', #53009, #39225, #93872, .T. ) ;
#19428 = CARTESIAN_POINT ( 'NONE',  ( 1.449999999999952660, 2.500000000000000000, -6.741600689897078169 ) ) ;
#19430 = ADVANCED_FACE ( 'NONE', ( #124622 ), #11271, .T. ) ;
#19429 = DIRECTION ( 'NONE',  ( -0.000000000000000000, 1.000000000000000000, -0.000000000000000000 ) ) ;
#19431 = DIRECTION ( 'NONE',  ( 0.000000000000000000, 1.000000000000000000, 0.000000000000000000 ) ) ;
#19433 = ORIENTED_EDGE ( 'NONE', *, *, #84749, .T. ) ;
#19432 = AXIS2_PLACEMENT_3D ( 'NONE', #110698, #41346, #43278 ) ;
#19434 = AXIS2_PLACEMENT_3D ( 'NONE', #69156, #10254, #50198 ) ;
#19435 = EDGE_CURVE ( 'NONE', #98451, #88829, #125264, .T. ) ;
#19436 = CIRCLE ( 'NONE', #96701, 0.06509327318403745899 ) ;
#19437 = DIRECTION ( 'NONE',  ( 0.000000000000000000, 0.000000000000000000, 1.000000000000000000 ) ) ;
#19439 = ORIENTED_EDGE ( 'NONE', *, *, #19711, .F. ) ;
#19438 = CIRCLE ( 'NONE', #75883, 0.06509327318403745899 ) ;
#19440 = PLANE ( 'NONE',  #9894 ) ;
#19441 = CONICAL_SURFACE ( 'NONE', #46533, 0.09999999999999982514, 0.003490658503988666988 ) ;
#19442 = DIRECTION ( 'NONE',  ( 0.000000000000000000, 0.000000000000000000, 1.000000000000000000 ) ) ;
#19443 = DIRECTION ( 'NONE',  ( 0.000000000000000000, 1.000000000000000000, 0.000000000000000000 ) ) ;
#19444 = EDGE_CURVE ( 'NONE', #30572, #40528, #5006, .T. ) ;
#19445 = FACE_OUTER_BOUND ( 'NONE', #116202, .T. ) ;
#19446 = AXIS2_PLACEMENT_3D ( 'NONE', #100859, #19066, #110054 ) ;
#19447 = EDGE_CURVE ( 'NONE', #117733, #1262, #15285, .T. ) ;
#19448 = ORIENTED_EDGE ( 'NONE', *, *, #13068, .F. ) ;
#19449 = EDGE_CURVE ( 'NONE', #69211, #30852, #55244, .T. ) ;
#19450 = EDGE_CURVE ( 'NONE', #127530, #96634, #117880, .T. ) ;
#19451 = EDGE_LOOP ( 'NONE', ( #13786, #59411, #38414, #79764 ) ) ;
#19452 = ORIENTED_EDGE ( 'NONE', *, *, #25619, .T. ) ;
#19453 = EDGE_LOOP ( 'NONE', ( #6844, #92308 ) ) ;
#19454 = ORIENTED_EDGE ( 'NONE', *, *, #47959, .T. ) ;
#19455 = DIRECTION ( 'NONE',  ( 0.000000000000000000, 1.000000000000000000, 0.000000000000000000 ) ) ;
#19456 = CARTESIAN_POINT ( 'NONE',  ( -4.150000000000024336, 2.500000000000000000, -2.757883832488654097 ) ) ;
#19457 = CARTESIAN_POINT ( 'NONE',  ( -7.900000000000014566, 2.500000000000000000, -3.637306695894650055 ) ) ;
#19458 = FACE_BOUND ( 'NONE', #39096, .T. ) ;
#19459 = CARTESIAN_POINT ( 'NONE',  ( 0.5999999999999551248, 12.50000000000000000, -4.676537180435978769 ) ) ;
#19460 = PLANE ( 'NONE',  #81886 ) ;
#19461 = EDGE_CURVE ( 'NONE', #100426, #103079, #122106, .T. ) ;
#19462 = DIRECTION ( 'NONE',  ( -0.000000000000000000, 1.000000000000000000, -0.000000000000000000 ) ) ;
#19463 = FACE_OUTER_BOUND ( 'NONE', #57604, .T. ) ;
#19464 = DIRECTION ( 'NONE',  ( -0.000000000000000000, 1.000000000000000000, -0.000000000000000000 ) ) ;
#19465 = CARTESIAN_POINT ( 'NONE',  ( -9.350000000000004974, 2.500000000000000000, 6.841600689897072485 ) ) ;
#19466 = FACE_OUTER_BOUND ( 'NONE', #25061, .T. ) ;
#19467 = AXIS2_PLACEMENT_3D ( 'NONE', #39904, #81729, #62756 ) ;
#19468 = AXIS2_PLACEMENT_3D ( 'NONE', #38838, #118000, #87882 ) ;
#19469 = CARTESIAN_POINT ( 'NONE',  ( 7.899999999999923084, 2.500000000000000000, -0.7928203230275543412 ) ) ;
#19470 = ORIENTED_EDGE ( 'NONE', *, *, #65269, .T. ) ;
#19471 = ORIENTED_EDGE ( 'NONE', *, *, #19557, .T. ) ;
#19472 = ORIENTED_EDGE ( 'NONE', *, *, #81741, .F. ) ;
#19473 = EDGE_LOOP ( 'NONE', ( #80709, #41385, #88456, #76562 ) ) ;
#19474 = DIRECTION ( 'NONE',  ( 0.000000000000000000, 0.000000000000000000, 1.000000000000000000 ) ) ;
#19475 = DIRECTION ( 'NONE',  ( -4.274815082592931898E-19, -0.9999939076577903929, -0.003490651415223739937 ) ) ;
#19476 = FACE_BOUND ( 'NONE', #53766, .T. ) ;
#19477 = CIRCLE ( 'NONE', #34164, 0.1000000000000002554 ) ;
#19478 = VECTOR ( 'NONE', #23405, 1000.000000000000000 ) ;
#19479 = FACE_OUTER_BOUND ( 'NONE', #363, .T. ) ;
#19480 = AXIS2_PLACEMENT_3D ( 'NONE', #119161, #80538, #98871 ) ;
#19481 = VECTOR ( 'NONE', #119887, 1000.000000000000000 ) ;
#19482 = ORIENTED_EDGE ( 'NONE', *, *, #50915, .T. ) ;
#19483 = DIRECTION ( 'NONE',  ( -0.000000000000000000, -1.000000000000000000, -0.000000000000000000 ) ) ;
#19484 = DIRECTION ( 'NONE',  ( 0.000000000000000000, 0.000000000000000000, -1.000000000000000000 ) ) ;
#19485 = DIRECTION ( 'NONE',  ( 0.000000000000000000, 0.000000000000000000, 1.000000000000000000 ) ) ;
#19486 = DIRECTION ( 'NONE',  ( 0.000000000000000000, 0.000000000000000000, 1.000000000000000000 ) ) ;
#19487 = DIRECTION ( 'NONE',  ( 0.000000000000000000, 0.000000000000000000, 1.000000000000000000 ) ) ;
#19488 = ORIENTED_EDGE ( 'NONE', *, *, #64158, .F. ) ;
#19489 = AXIS2_PLACEMENT_3D ( 'NONE', #40418, #48286, #28000 ) ;
#19490 = DIRECTION ( 'NONE',  ( 0.000000000000000000, 0.000000000000000000, 1.000000000000000000 ) ) ;
#19491 = EDGE_CURVE ( 'NONE', #124192, #17292, #107427, .T. ) ;
#19492 = AXIS2_PLACEMENT_3D ( 'NONE', #51990, #111542, #101078 ) ;
#19493 = AXIS2_PLACEMENT_3D ( 'NONE', #66400, #25842, #56570 ) ;
#19494 = CONICAL_SURFACE ( 'NONE', #67505, 0.1000000000000002554, 0.003490658503988666988 ) ;
#19495 = ORIENTED_EDGE ( 'NONE', *, *, #88891, .T. ) ;
#19496 = ORIENTED_EDGE ( 'NONE', *, *, #119756, .T. ) ;
#19497 = DIRECTION ( 'NONE',  ( -0.000000000000000000, -1.000000000000000000, -0.000000000000000000 ) ) ;
#19498 = DIRECTION ( 'NONE',  ( 0.000000000000000000, -0.9999939076577903929, 0.003490651415223739937 ) ) ;
#19499 = AXIS2_PLACEMENT_3D ( 'NONE', #10922, #41085, #123471 ) ;
#19500 = VERTEX_POINT ( 'NONE', #87258 ) ;
#19501 = FACE_OUTER_BOUND ( 'NONE', #19413, .T. ) ;
#19502 = DIRECTION ( 'NONE',  ( 0.000000000000000000, 0.000000000000000000, 1.000000000000000000 ) ) ;
#19503 = ORIENTED_EDGE ( 'NONE', *, *, #108097, .T. ) ;
#19504 = DIRECTION ( 'NONE',  ( 0.000000000000000000, 0.000000000000000000, -1.000000000000000000 ) ) ;
#19505 = EDGE_LOOP ( 'NONE', ( #103192, #97868, #89992, #40928 ) ) ;
#19506 = EDGE_CURVE ( 'NONE', #112250, #40839, #47354, .T. ) ;
#19507 = CARTESIAN_POINT ( 'NONE',  ( -9.350000000000008527, 2.500000000000000000, -6.148780366869520897 ) ) ;
#19508 = EDGE_LOOP ( 'NONE', ( #58858, #90991, #115167, #97260 ) ) ;
#19509 = CARTESIAN_POINT ( 'NONE',  ( -0.2000000000000404232, 2.500000000000000000, 4.083716857408421497 ) ) ;
#19510 = FACE_BOUND ( 'NONE', #119146, .T. ) ;
#19511 = EDGE_LOOP ( 'NONE', ( #51870, #72439 ) ) ;
#19512 = CARTESIAN_POINT ( 'NONE',  ( 5.399999999999933742, 2.500000000000000000, 0.09999999999999761857 ) ) ;
#19513 = ORIENTED_EDGE ( 'NONE', *, *, #58525, .F. ) ;
#19514 = DIRECTION ( 'NONE',  ( -1.445602896647339656E-16, 0.000000000000000000, -1.000000000000000000 ) ) ;
#19515 = CARTESIAN_POINT ( 'NONE',  ( -10.80000000000000249, 2.500000000000000000, -4.330127018922197202 ) ) ;
#19516 = CIRCLE ( 'NONE', #21577, 0.06509327318403745899 ) ;
#19517 = CARTESIAN_POINT ( 'NONE',  ( 4.199999999999938005, 2.500000000000000000, 4.330127018922196314 ) ) ;
#19518 = AXIS2_PLACEMENT_3D ( 'NONE', #111238, #22897, #41895 ) ;
#19519 = DIRECTION ( 'NONE',  ( -1.445602896647339656E-16, 0.000000000000000000, -1.000000000000000000 ) ) ;
#19520 = DIRECTION ( 'NONE',  ( 0.000000000000000000, 0.000000000000000000, 1.000000000000000000 ) ) ;
#19521 = VERTEX_POINT ( 'NONE', #68913 ) ;
#19522 = ORIENTED_EDGE ( 'NONE', *, *, #23625, .F. ) ;
#19523 = ORIENTED_EDGE ( 'NONE', *, *, #66114, .F. ) ;
#19524 = DIRECTION ( 'NONE',  ( 0.000000000000000000, 0.000000000000000000, 1.000000000000000000 ) ) ;
#19525 = CIRCLE ( 'NONE', #119879, 0.06509327318403745899 ) ;
#19526 = CIRCLE ( 'NONE', #76062, 0.06509327318403741736 ) ;
#19527 = DIRECTION ( 'NONE',  ( -0.000000000000000000, -1.000000000000000000, -0.000000000000000000 ) ) ;
#19528 = AXIS2_PLACEMENT_3D ( 'NONE', #4361, #84229, #126758 ) ;
#19529 = CARTESIAN_POINT ( 'NONE',  ( 1.049999999999952971, 2.500000000000000000, 6.248780366869521430 ) ) ;
#19531 = ORIENTED_EDGE ( 'NONE', *, *, #73398, .F. ) ;
#19530 = EDGE_LOOP ( 'NONE', ( #46823, #81014 ) ) ;
#19532 = EDGE_LOOP ( 'NONE', ( #59531, #123960 ) ) ;
#19533 = CARTESIAN_POINT ( 'NONE',  ( 97.50000000000000000, 2.449293598294706414E-16, -2.000000000000000000 ) ) ;
#19534 = CARTESIAN_POINT ( 'NONE',  ( 11.89999999999990798, 2.500000000000000000, 4.676537180435972552 ) ) ;
#19535 = AXIS2_PLACEMENT_3D ( 'NONE', #38617, #109255, #29427 ) ;
#19536 = VECTOR ( 'NONE', #19180, 1000.000000000000000 ) ;
#19538 = EDGE_CURVE ( 'NONE', #86078, #28471, #128384, .T. ) ;
#19537 = AXIS2_PLACEMENT_3D ( 'NONE', #2902, #43481, #42856 ) ;
#19539 = CONTEXT_DEPENDENT_SHAPE_REPRESENTATION ( #104881, #24231 ) ;
#19540 = CARTESIAN_POINT ( 'NONE',  ( 1.899999999999951283, 2.500000000000000000, 0.3464101615137736845 ) ) ;
#19541 = CARTESIAN_POINT ( 'NONE',  ( -2.100000000000033840, 2.500000000000000000, 3.537306695894645081 ) ) ;
#19542 = FACE_OUTER_BOUND ( 'NONE', #74126, .T. ) ;
#19543 = CIRCLE ( 'NONE', #126151, 0.06509327318403745899 ) ;
#19544 = CARTESIAN_POINT ( 'NONE',  ( 2.899999999999943956, 2.500000000000000000, 4.230127018922196669 ) ) ;
#19545 = PLANE ( 'NONE',  #115654 ) ;
#19546 = DIRECTION ( 'NONE',  ( 0.000000000000000000, 1.000000000000000000, 0.000000000000000000 ) ) ;
#19548 = EDGE_CURVE ( 'NONE', #94029, #30530, #80249, .T. ) ;
#19547 = AXIS2_PLACEMENT_3D ( 'NONE', #121788, #62887, #112635 ) ;
#19549 = ORIENTED_EDGE ( 'NONE', *, *, #104637, .T. ) ;
#19550 = ORIENTED_EDGE ( 'NONE', *, *, #38222, .T. ) ;
#19551 = CARTESIAN_POINT ( 'NONE',  ( 9.149999999999920419, 2.500000000000000000, 2.857883832488649301 ) ) ;
#19552 = DIRECTION ( 'NONE',  ( 0.000000000000000000, 0.000000000000000000, 1.000000000000000000 ) ) ;
#19553 = EDGE_CURVE ( 'NONE', #123660, #106056, #86491, .T. ) ;
#19554 = ORIENTED_EDGE ( 'NONE', *, *, #24859, .T. ) ;
#19555 = EDGE_CURVE ( 'NONE', #93259, #41595, #124146, .T. ) ;
#19556 = EDGE_LOOP ( 'NONE', ( #46189, #40892 ) ) ;
#19557 = EDGE_CURVE ( 'NONE', #106765, #66380, #84445, .T. ) ;
#19558 = CARTESIAN_POINT ( 'NONE',  ( 186.2343750003414016, 8.734944146203032389, 5.348610694689227483E-16 ) ) ;
#19560 = ADVANCED_FACE ( 'NONE', ( #9358 ), #28009, .T. ) ;
#19559 = DIRECTION ( 'NONE',  ( -0.000000000000000000, 1.000000000000000000, -0.000000000000000000 ) ) ;
#19561 = ADVANCED_FACE ( 'NONE', ( #28361 ), #71937, .T. ) ;
#19562 = CARTESIAN_POINT ( 'NONE',  ( 2.500000000000002220, 1.500000000000000444, -9.999999999999998224 ) ) ;
#19563 = CONICAL_SURFACE ( 'NONE', #92726, 0.1000000000000000472, 0.003490658503988666988 ) ;
#19564 = CARTESIAN_POINT ( 'NONE',  ( -2.050000000000032685, 2.500000000000000000, -2.165063509461101710 ) ) ;
#19565 = DIRECTION ( 'NONE',  ( 0.000000000000000000, 0.000000000000000000, 1.000000000000000000 ) ) ;
#19566 = CARTESIAN_POINT ( 'NONE',  ( 2.499999999999948930, 2.500000000000000000, -5.122947341949753763 ) ) ;
#19567 = DIRECTION ( 'NONE',  ( -0.000000000000000000, 1.000000000000000000, -0.000000000000000000 ) ) ;
#19568 = EDGE_CURVE ( 'NONE', #101562, #116228, #69870, .T. ) ;
#19569 = CIRCLE ( 'NONE', #94781, 0.1000000000000002554 ) ;
#19572 = EDGE_CURVE ( 'NONE', #70666, #69440, #99121, .T. ) ;
#19571 = CIRCLE ( 'NONE', #92734, 0.1000000000000002554 ) ;
#19570 = CARTESIAN_POINT ( 'NONE',  ( 149.5981739382431783, 2.500000000000000000, 1.703575533167231537 ) ) ;
#19573 = AXIS2_PLACEMENT_3D ( 'NONE', #91743, #83223, #102836 ) ;
#19574 = ADVANCED_FACE ( 'NONE', ( #87893 ), #127839, .T. ) ;
#19575 = ORIENTED_EDGE ( 'NONE', *, *, #71733, .F. ) ;
#19576 = ORIENTED_EDGE ( 'NONE', *, *, #114404, .F. ) ;
#19577 = ORIENTED_EDGE ( 'NONE', *, *, #98575, .T. ) ;
#19578 = VERTEX_POINT ( 'NONE', #89202 ) ;
#19579 = VECTOR ( 'NONE', #36558, 1000.000000000000000 ) ;
#19580 = CARTESIAN_POINT ( 'NONE',  ( 1.699999999999950218, 2.500000000000000000, 4.230127018922196669 ) ) ;
#19581 = DIRECTION ( 'NONE',  ( 0.000000000000000000, 0.000000000000000000, -1.000000000000000000 ) ) ;
#19582 = AXIS2_PLACEMENT_3D ( 'NONE', #63841, #105033, #113584 ) ;
#19583 = CONICAL_SURFACE ( 'NONE', #36224, 0.09999999999999982514, 0.003490658503988666988 ) ;
#19584 = ORIENTED_EDGE ( 'NONE', *, *, #28109, .T. ) ;
#19585 = DIRECTION ( 'NONE',  ( -4.274815082592931898E-19, -0.9999939076577903929, -0.003490651415223739937 ) ) ;
#19586 = CIRCLE ( 'NONE', #78069, 0.06509327318403745899 ) ;
#19587 = CARTESIAN_POINT ( 'NONE',  ( 4.799999999999935874, 2.500000000000000000, 4.083716857408421497 ) ) ;
#19588 = CARTESIAN_POINT ( 'NONE',  ( 2.099999999999950351, 12.50000000000000000, -5.088040615133791356 ) ) ;
#19590 = EDGE_LOOP ( 'NONE', ( #126768, #95847, #41194, #17640 ) ) ;
#19589 = DIRECTION ( 'NONE',  ( 0.000000000000000000, 1.000000000000000000, 0.000000000000000000 ) ) ;
#19591 = DIRECTION ( 'NONE',  ( 0.000000000000000000, 0.000000000000000000, 1.000000000000000000 ) ) ;
#19592 = CIRCLE ( 'NONE', #13312, 0.09999999999999982514 ) ;
#19593 = DIRECTION ( 'NONE',  ( -0.000000000000000000, 1.000000000000000000, -0.000000000000000000 ) ) ;
#19594 = ORIENTED_EDGE ( 'NONE', *, *, #118546, .F. ) ;
#19595 = AXIS2_PLACEMENT_3D ( 'NONE', #119263, #40075, #19113 ) ;
#19596 = AXIS2_PLACEMENT_3D ( 'NONE', #651, #57655, #28193 ) ;
#19597 = AXIS2_PLACEMENT_3D ( 'NONE', #59325, #99232, #27247 ) ;
#19598 = EDGE_LOOP ( 'NONE', ( #55170, #63083 ) ) ;
#19599 = EDGE_LOOP ( 'NONE', ( #45999, #37101, #75251, #58764 ) ) ;
#19600 = VERTEX_POINT ( 'NONE', #78104 ) ;
#19601 = CARTESIAN_POINT ( 'NONE',  ( -2.700000000000030376, 12.50000000000000000, 3.983716857408420964 ) ) ;
#19602 = AXIS2_PLACEMENT_3D ( 'NONE', #12081, #60569, #72311 ) ;
#19603 = CARTESIAN_POINT ( 'NONE',  ( 108.0000000000000142, 9.000000000000001776, -5.000000000000004441 ) ) ;
#19604 = LINE ( 'NONE', #69326, #73239 ) ;
#19605 = AXIS2_PLACEMENT_3D ( 'NONE', #18507, #127815, #17857 ) ;
#19606 = ORIENTED_EDGE ( 'NONE', *, *, #71310, .T. ) ;
#19607 = CARTESIAN_POINT ( 'NONE',  ( -9.600000000000008527, 2.500000000000000000, 4.430127018922196847 ) ) ;
#19608 = DIRECTION ( 'NONE',  ( 0.000000000000000000, 0.000000000000000000, -1.000000000000000000 ) ) ;
#19609 = CARTESIAN_POINT ( 'NONE',  ( -10.65000000000000213, 2.500000000000000000, 6.248780366869520542 ) ) ;
#19610 = DIRECTION ( 'NONE',  ( -0.000000000000000000, 1.000000000000000000, -0.000000000000000000 ) ) ;
#19611 = EDGE_CURVE ( 'NONE', #98546, #52824, #7056, .T. ) ;
#19612 = ADVANCED_FACE ( 'NONE', ( #18526 ), #53145, .T. ) ;
#19613 = ORIENTED_EDGE ( 'NONE', *, *, #53378, .F. ) ;
#19614 = CARTESIAN_POINT ( 'NONE',  ( 187.4166666666666856, 6.668395609140176816, 3.850000000000000977 ) ) ;
#19615 = EDGE_CURVE ( 'NONE', #77606, #64779, #8685, .T. ) ;
#19616 = EDGE_LOOP ( 'NONE', ( #94872, #78363, #95697, #59410 ) ) ;
#19617 = EDGE_LOOP ( 'NONE', ( #38079, #2624 ) ) ;
#19619 = AXIS2_PLACEMENT_3D ( 'NONE', #34548, #124842, #16143 ) ;
#19618 = FACE_OUTER_BOUND ( 'NONE', #48682, .T. ) ;
#19620 = CIRCLE ( 'NONE', #117791, 0.1000000000000002554 ) ;
#19621 = CARTESIAN_POINT ( 'NONE',  ( 9.549999999999918998, 2.500000000000000000, -6.595190528383302109 ) ) ;
#19622 = FACE_BOUND ( 'NONE', #102299, .T. ) ;
#19623 = CARTESIAN_POINT ( 'NONE',  ( 3.749999999999975131, 12.50000000000000000, 6.560283801567334372 ) ) ;
#19624 = CARTESIAN_POINT ( 'NONE',  ( 165.4999999999999716, 0.000000000000000000, -2.000000000000000000 ) ) ;
#19625 = ADVANCED_FACE ( 'NONE', ( #78762 ), #86576, .T. ) ;
#19626 = DIRECTION ( 'NONE',  ( 0.000000000000000000, 0.000000000000000000, 1.000000000000000000 ) ) ;
#19627 = CIRCLE ( 'NONE', #7077, 0.1000000000000002554 ) ;
#19628 = AXIS2_PLACEMENT_3D ( 'NONE', #116305, #26018, #26659 ) ;
#19629 = AXIS2_PLACEMENT_3D ( 'NONE', #101705, #80784, #90578 ) ;
#19630 = CONICAL_SURFACE ( 'NONE', #124179, 0.09999999999999999167, 0.003490658503988666988 ) ;
#19631 = VECTOR ( 'NONE', #70137, 1000.000000000000000 ) ;
#19632 = EDGE_LOOP ( 'NONE', ( #111815, #75720, #61324, #11660 ) ) ;
#19633 = FACE_OUTER_BOUND ( 'NONE', #74323, .T. ) ;
#19634 = FACE_OUTER_BOUND ( 'NONE', #67407, .T. ) ;
#19635 = FACE_OUTER_BOUND ( 'NONE', #8386, .T. ) ;
#19636 = DIRECTION ( 'NONE',  ( -0.000000000000000000, -1.000000000000000000, -0.000000000000000000 ) ) ;
#19637 = ORIENTED_EDGE ( 'NONE', *, *, #52778, .F. ) ;
#19639 = DIRECTION ( 'NONE',  ( 0.000000000000000000, -0.000000000000000000, 1.000000000000000000 ) ) ;
#19638 = CONICAL_SURFACE ( 'NONE', #36375, 0.1000000000000002554, 0.003490658503988666988 ) ;
#19640 = AXIS2_PLACEMENT_3D ( 'NONE', #66071, #73969, #85074 ) ;
#19641 = AXIS2_PLACEMENT_3D ( 'NONE', #6098, #126545, #25753 ) ;
#19642 = DIRECTION ( 'NONE',  ( 0.000000000000000000, 0.000000000000000000, -1.000000000000000000 ) ) ;
#19643 = EDGE_LOOP ( 'NONE', ( #98365, #10971, #29002, #129560 ) ) ;
#19644 = VERTEX_POINT ( 'NONE', #119299 ) ;
#19645 = AXIS2_PLACEMENT_3D ( 'NONE', #19731, #11178, #59675 ) ;
#19646 = CARTESIAN_POINT ( 'NONE',  ( 4.549999999999935874, 12.50000000000000000, 6.495190528383297135 ) ) ;
#19647 = DIRECTION ( 'NONE',  ( 0.000000000000000000, 1.000000000000000000, 0.000000000000000000 ) ) ;
#19648 = EDGE_CURVE ( 'NONE', #40995, #64274, #17527, .T. ) ;
#19649 = FACE_BOUND ( 'NONE', #14100, .T. ) ;
#19650 = CARTESIAN_POINT ( 'NONE',  ( 10.04522989427051982, -2.499999999999999112, -8.164691043833789408 ) ) ;
#19651 = CARTESIAN_POINT ( 'NONE',  ( 4.999999999999935163, 2.500000000000000000, 0.6928203230275494784 ) ) ;
#19652 = ORIENTED_EDGE ( 'NONE', *, *, #117855, .F. ) ;
#19653 = CARTESIAN_POINT ( 'NONE',  ( 9.149999999999920419, 12.50000000000000000, 1.407149913249508000 ) ) ;
#19654 = CARTESIAN_POINT ( 'NONE',  ( 184.6250000000000000, -8.891194145520236347, -1.633285867636356693E-15 ) ) ;
#19656 = EDGE_LOOP ( 'NONE', ( #14533, #11589 ) ) ;
#19655 = AXIS2_PLACEMENT_3D ( 'NONE', #77887, #29455, #39303 ) ;
#19657 = DIRECTION ( 'NONE',  ( -0.000000000000000000, -1.000000000000000000, -0.000000000000000000 ) ) ;
#19658 = CARTESIAN_POINT ( 'NONE',  ( -8.100000000000013856, 12.50000000000000000, -4.676537180435977881 ) ) ;
#19659 = EDGE_CURVE ( 'NONE', #77218, #115634, #111636, .T. ) ;
#19660 = DIRECTION ( 'NONE',  ( 0.000000000000000000, 1.000000000000000000, 0.000000000000000000 ) ) ;
#19661 = DIRECTION ( 'NONE',  ( 0.000000000000000000, 0.000000000000000000, 1.000000000000000000 ) ) ;
#19662 = CONICAL_SURFACE ( 'NONE', #111696, 0.1000000000000002554, 0.003490658503988666988 ) ;
#19663 = AXIS2_PLACEMENT_3D ( 'NONE', #115213, #28164, #37349 ) ;
#19664 = ORIENTED_EDGE ( 'NONE', *, *, #45144, .F. ) ;
#19665 = CARTESIAN_POINT ( 'NONE',  ( -7.900000000000014566, 2.500000000000000000, 0.6928203230275494784 ) ) ;
#19666 = DIRECTION ( 'NONE',  ( -0.000000000000000000, -1.000000000000000000, -0.000000000000000000 ) ) ;
#19667 = CARTESIAN_POINT ( 'NONE',  ( 8.349999999999923261, 2.500000000000000000, -6.495190528383302464 ) ) ;
#19668 = DIRECTION ( 'NONE',  ( -0.000000000000000000, -1.000000000000000000, -0.000000000000000000 ) ) ;
#19669 = VERTEX_POINT ( 'NONE', #97093 ) ;
#19670 = ORIENTED_EDGE ( 'NONE', *, *, #40152, .T. ) ;
#19671 = EDGE_CURVE ( 'NONE', #42458, #40528, #110765, .T. ) ;
#19672 = AXIS2_PLACEMENT_3D ( 'NONE', #127502, #60066, #79678 ) ;
#19673 = CARTESIAN_POINT ( 'NONE',  ( 6.699999999999930012, 12.50000000000000000, 4.330127018922196314 ) ) ;
#19674 = ORIENTED_EDGE ( 'NONE', *, *, #104362, .F. ) ;
#19676 = DIRECTION ( 'NONE',  ( 0.000000000000000000, 0.000000000000000000, -1.000000000000000000 ) ) ;
#19675 = CIRCLE ( 'NONE', #40535, 0.1000000000000002554 ) ;
#19677 = DIRECTION ( 'NONE',  ( 0.000000000000000000, 0.000000000000000000, -1.000000000000000000 ) ) ;
#19678 = AXIS2_PLACEMENT_3D ( 'NONE', #129423, #111011, #111690 ) ;
#19679 = CARTESIAN_POINT ( 'NONE',  ( -1.250000000000037526, 12.50000000000000000, -1.472243186433550122 ) ) ;
#19680 = ORIENTED_EDGE ( 'NONE', *, *, #111436, .T. ) ;
#19681 = CARTESIAN_POINT ( 'NONE',  ( 187.5000000000000000, 0.000000000000000000, 0.000000000000000000 ) ) ;
#19682 = CARTESIAN_POINT ( 'NONE',  ( 8.749999999999918288, 2.500000000000000000, -1.472243186433550122 ) ) ;
#19683 = CARTESIAN_POINT ( 'NONE',  ( 12.09999999999990550, 12.50000000000000000, 4.330127018922196314 ) ) ;
#19684 = EDGE_CURVE ( 'NONE', #85856, #55123, #92956, .T. ) ;
#19685 = FACE_OUTER_BOUND ( 'NONE', #78952, .T. ) ;
#19686 = CARTESIAN_POINT ( 'NONE',  ( 1.649999999999951505, 12.50000000000000000, 1.472243186433545459 ) ) ;
#19687 = DIRECTION ( 'NONE',  ( 0.000000000000000000, 1.000000000000000000, 0.000000000000000000 ) ) ;
#19688 = ORIENTED_EDGE ( 'NONE', *, *, #4010, .T. ) ;
#19689 = ORIENTED_EDGE ( 'NONE', *, *, #100437, .T. ) ;
#19690 = DIRECTION ( 'NONE',  ( 0.000000000000000000, -0.000000000000000000, 1.000000000000000000 ) ) ;
#19692 = ORIENTED_EDGE ( 'NONE', *, *, #115021, .T. ) ;
#19691 = VECTOR ( 'NONE', #25566, 1000.000000000000000 ) ;
#19693 = AXIS2_PLACEMENT_3D ( 'NONE', #99934, #29896, #129419 ) ;
#19694 = CIRCLE ( 'NONE', #90700, 0.06509327318403743123 ) ;
#19695 = DIRECTION ( 'NONE',  ( -0.000000000000000000, -1.000000000000000000, -0.000000000000000000 ) ) ;
#19697 = ORIENTED_EDGE ( 'NONE', *, *, #127276, .F. ) ;
#19696 = ORIENTED_EDGE ( 'NONE', *, *, #4625, .F. ) ;
#19698 = ORIENTED_EDGE ( 'NONE', *, *, #41322, .T. ) ;
#19699 = CONICAL_SURFACE ( 'NONE', #9230, 0.09999999999999982514, 0.003490658503988666988 ) ;
#19700 = CARTESIAN_POINT ( 'NONE',  ( 13.34999999999990017, 12.50000000000000000, 2.165063509461097713 ) ) ;
#19701 = CARTESIAN_POINT ( 'NONE',  ( -10.60000000000000142, 2.500000000000000000, 0.3464101615137736845 ) ) ;
#19702 = CARTESIAN_POINT ( 'NONE',  ( 6.849999999999930367, 2.500000000000000000, -6.148780366869526226 ) ) ;
#19703 = EDGE_CURVE ( 'NONE', #58714, #48991, #38590, .T. ) ;
#19704 = DIRECTION ( 'NONE',  ( -0.000000000000000000, -1.000000000000000000, -0.000000000000000000 ) ) ;
#19705 = CARTESIAN_POINT ( 'NONE',  ( -14.79999999999998472, 2.500000000000000000, 0.4464101615137758272 ) ) ;
#19706 = CARTESIAN_POINT ( 'NONE',  ( 185.7916666666666856, 4.445597072760072876, -7.700000000000080114 ) ) ;
#19707 = DIRECTION ( 'NONE',  ( -0.000000000000000000, -1.000000000000000000, -0.000000000000000000 ) ) ;
#19708 = DIRECTION ( 'NONE',  ( -0.000000000000000000, -1.000000000000000000, -0.000000000000000000 ) ) ;
#19709 = FACE_OUTER_BOUND ( 'NONE', #127559, .T. ) ;
#19710 = ORIENTED_EDGE ( 'NONE', *, *, #111809, .T. ) ;
#19711 = EDGE_CURVE ( 'NONE', #89250, #47871, #86675, .T. ) ;
#19712 = ORIENTED_EDGE ( 'NONE', *, *, #83699, .F. ) ;
#19713 = CONICAL_SURFACE ( 'NONE', #111736, 0.1000000000000002554, 0.003490658503988666988 ) ;
#19714 = FACE_OUTER_BOUND ( 'NONE', #88999, .T. ) ;
#19715 = AXIS2_PLACEMENT_3D ( 'NONE', #37750, #88101, #49515 ) ;
#19716 = EDGE_CURVE ( 'NONE', #73117, #89300, #97051, .T. ) ;
#19717 = AXIS2_PLACEMENT_3D ( 'NONE', #100628, #10332, #10945 ) ;
#19718 = ORIENTED_EDGE ( 'NONE', *, *, #31540, .T. ) ;
#19719 = EDGE_CURVE ( 'NONE', #74320, #86613, #55292, .T. ) ;
#19720 = ORIENTED_EDGE ( 'NONE', *, *, #1118, .F. ) ;
#19721 = EDGE_CURVE ( 'NONE', #125242, #7618, #122537, .T. ) ;
#19722 = CARTESIAN_POINT ( 'NONE',  ( 11.64999999999990798, 2.500000000000000000, -1.472243186433550122 ) ) ;
#19723 = ADVANCED_FACE ( 'NONE', ( #100944 ), #7154, .T. ) ;
#19724 = CIRCLE ( 'NONE', #92891, 0.06509327318403745899 ) ;
#19725 = AXIS2_PLACEMENT_3D ( 'NONE', #31186, #39729, #50180 ) ;
#19726 = DIRECTION ( 'NONE',  ( -0.000000000000000000, 1.000000000000000000, -0.000000000000000000 ) ) ;
#19728 = DIRECTION ( 'NONE',  ( -0.000000000000000000, -1.000000000000000000, -0.000000000000000000 ) ) ;
#19727 = CIRCLE ( 'NONE', #122224, 0.1000000000000002554 ) ;
#19729 = CARTESIAN_POINT ( 'NONE',  ( -4.550000000000022915, 2.500000000000000000, 6.495190528383297135 ) ) ;
#19730 = EDGE_CURVE ( 'NONE', #125465, #13400, #26046, .T. ) ;
#19731 = CARTESIAN_POINT ( 'NONE',  ( 13.09999999999990195, 12.50000000000000000, 4.676537180435972552 ) ) ;
#19732 = EDGE_LOOP ( 'NONE', ( #45833, #83758 ) ) ;
#19733 = EDGE_CURVE ( 'NONE', #48204, #86305, #32333, .T. ) ;
#19734 = ADVANCED_FACE ( 'NONE', ( #70856 ), #81326, .T. ) ;
#19735 = VECTOR ( 'NONE', #21371, 1000.000000000000000 ) ;
#19736 = ADVANCED_FACE ( 'NONE', ( #60412 ), #36525, .T. ) ;
#19737 = ORIENTED_EDGE ( 'NONE', *, *, #69680, .F. ) ;
#19738 = DIRECTION ( 'NONE',  ( -0.000000000000000000, -1.000000000000000000, -0.000000000000000000 ) ) ;
#19739 = CIRCLE ( 'NONE', #115863, 0.09999999999999982514 ) ;
#19740 = ADVANCED_FACE ( 'NONE', ( #112719 ), #120598, .T. ) ;
#19741 = VERTEX_POINT ( 'NONE', #23045 ) ;
#19742 = CARTESIAN_POINT ( 'NONE',  ( 13.09999999999989839, 2.500000000000000000, 0.3464101615137735735 ) ) ;
#19743 = ORIENTED_EDGE ( 'NONE', *, *, #10574, .F. ) ;
#19744 = VECTOR ( 'NONE', #6481, 1000.000000000000000 ) ;
#19745 = ORIENTED_EDGE ( 'NONE', *, *, #96121, .T. ) ;
#19746 = ADVANCED_FACE ( 'NONE', ( #112072 ), #62335, .T. ) ;
#19747 = PLANE ( 'NONE',  #125526 ) ;
#19748 = CARTESIAN_POINT ( 'NONE',  ( 5.199999999999933564, 2.500000000000000000, 0.2464101615137735679 ) ) ;
#19749 = CARTESIAN_POINT ( 'NONE',  ( -8.300000000000009592, 12.50000000000000000, 4.330127018922196314 ) ) ;
#19750 = DIRECTION ( 'NONE',  ( -4.274815082592931898E-19, -0.9999939076577903929, -0.003490651415223739937 ) ) ;
#19751 = DIRECTION ( 'NONE',  ( 0.000000000000000000, 0.000000000000000000, 1.000000000000000000 ) ) ;
#19752 = ORIENTED_EDGE ( 'NONE', *, *, #70959, .T. ) ;
#19753 = DIRECTION ( 'NONE',  ( 0.000000000000000000, 0.000000000000000000, -1.000000000000000000 ) ) ;
#19754 = CARTESIAN_POINT ( 'NONE',  ( 8.149999999999923972, 2.500000000000000000, -6.841600689897077814 ) ) ;
#19755 = DIRECTION ( 'NONE',  ( 0.000000000000000000, 0.000000000000000000, 1.000000000000000000 ) ) ;
#19756 = CARTESIAN_POINT ( 'NONE',  ( 14.39999999999989555, 12.50000000000000000, -0.3464101615137782364 ) ) ;
#19757 = FACE_OUTER_BOUND ( 'NONE', #10532, .T. ) ;
#19758 = VERTEX_POINT ( 'NONE', #62964 ) ;
#19759 = VERTEX_POINT ( 'NONE', #52493 ) ;
#19760 = CARTESIAN_POINT ( 'NONE',  ( -10.40000000000000213, 2.500000000000000000, -4.430127018922197735 ) ) ;
#19761 = ORIENTED_EDGE ( 'NONE', *, *, #103584, .F. ) ;
#19762 = AXIS2_PLACEMENT_3D ( 'NONE', #126721, #76973, #67112 ) ;
#19763 = CARTESIAN_POINT ( 'NONE',  ( 13.34999999999989662, 2.500000000000000000, -2.957883832488653830 ) ) ;
#19764 = CARTESIAN_POINT ( 'NONE',  ( -13.14999999999999147, 12.50000000000000000, 2.446380397790839822 ) ) ;
#19765 = VECTOR ( 'NONE', #112536, 1000.000000000000000 ) ;
#19766 = EDGE_LOOP ( 'NONE', ( #113661, #2123, #18677, #32329 ) ) ;
#19767 = FACE_OUTER_BOUND ( 'NONE', #83306, .T. ) ;
#19768 = DIRECTION ( 'NONE',  ( -0.000000000000000000, 1.000000000000000000, -0.000000000000000000 ) ) ;
#19769 = CARTESIAN_POINT ( 'NONE',  ( 8.749999999999918288, 12.50000000000000000, 7.188010851410848723 ) ) ;
#19770 = DIRECTION ( 'NONE',  ( 0.000000000000000000, 0.000000000000000000, 1.000000000000000000 ) ) ;
#19771 = CONICAL_SURFACE ( 'NONE', #128455, 0.09999999999999982514, 0.003490658503988666988 ) ;
#19772 = EDGE_CURVE ( 'NONE', #78977, #98217, #124249, .T. ) ;
#19773 = DIRECTION ( 'NONE',  ( 0.000000000000000000, 0.000000000000000000, 1.000000000000000000 ) ) ;
#19775 = EDGE_CURVE ( 'NONE', #85514, #87169, #63608, .T. ) ;
#19774 = CIRCLE ( 'NONE', #53232, 0.09999999999999982514 ) ;
#19776 = ORIENTED_EDGE ( 'NONE', *, *, #11944, .F. ) ;
#19777 = DIRECTION ( 'NONE',  ( 0.000000000000000000, 0.000000000000000000, -1.000000000000000000 ) ) ;
#19778 = DIRECTION ( 'NONE',  ( -0.000000000000000000, 1.000000000000000000, -0.000000000000000000 ) ) ;
#19779 = DIRECTION ( 'NONE',  ( -0.000000000000000000, 1.000000000000000000, -0.000000000000000000 ) ) ;
#19780 = EDGE_CURVE ( 'NONE', #83439, #89946, #117967, .T. ) ;
#19781 = ORIENTED_EDGE ( 'NONE', *, *, #31835, .F. ) ;
#19782 = VECTOR ( 'NONE', #78574, 1000.000000000000000 ) ;
#19783 = CIRCLE ( 'NONE', #7233, 7.699999999999999289 ) ;
#19784 = CARTESIAN_POINT ( 'NONE',  ( 11.64999999999990621, 2.500000000000000000, -2.065063509461102065 ) ) ;
#19786 = ORIENTED_EDGE ( 'NONE', *, *, #71988, .F. ) ;
#19785 = CONICAL_SURFACE ( 'NONE', #126391, 0.09999999999999982514, 0.003490658503988666988 ) ;
#19787 = CARTESIAN_POINT ( 'NONE',  ( -6.650000000000014566, 2.500000000000000000, 1.472243186433545459 ) ) ;
#19788 = LINE ( 'NONE', #18485, #6914 ) ;
#19789 = DIRECTION ( 'NONE',  ( 0.000000000000000000, 1.000000000000000000, 0.000000000000000000 ) ) ;
#19790 = AXIS2_PLACEMENT_3D ( 'NONE', #91919, #71629, #41550 ) ;
#19791 = VERTEX_POINT ( 'NONE', #93086 ) ;
#19792 = DIRECTION ( 'NONE',  ( 0.000000000000000000, 0.000000000000000000, -1.000000000000000000 ) ) ;
#19793 = CARTESIAN_POINT ( 'NONE',  ( -13.09999999999999254, 2.500000000000000000, 0.3464101615137777923 ) ) ;
#19794 = ORIENTED_EDGE ( 'NONE', *, *, #104993, .T. ) ;
#19795 = CARTESIAN_POINT ( 'NONE',  ( 3.349999999999943689, 2.500000000000000000, 2.065063509461097624 ) ) ;
#19796 = VERTEX_POINT ( 'NONE', #3399 ) ;
#19797 = CARTESIAN_POINT ( 'NONE',  ( 1.049999999999954081, 2.500000000000000000, -6.248780366869526759 ) ) ;
#19798 = VECTOR ( 'NONE', #31337, 1000.000000000000000 ) ;
#19799 = ORIENTED_EDGE ( 'NONE', *, *, #79658, .T. ) ;
#19800 = DIRECTION ( 'NONE',  ( -0.000000000000000000, 1.000000000000000000, -0.000000000000000000 ) ) ;
#19801 = CARTESIAN_POINT ( 'NONE',  ( 9.149999999999916866, 2.500000000000000000, 5.902370205355745192 ) ) ;
#19802 = AXIS2_PLACEMENT_3D ( 'NONE', #1053, #77670, #49526 ) ;
#19803 = AXIS2_PLACEMENT_3D ( 'NONE', #29079, #78826, #79463 ) ;
#19804 = AXIS2_PLACEMENT_3D ( 'NONE', #24031, #65213, #105806 ) ;
#19805 = ORIENTED_EDGE ( 'NONE', *, *, #22918, .F. ) ;
#19806 = EDGE_LOOP ( 'NONE', ( #97022, #113275 ) ) ;
#19807 = DIRECTION ( 'NONE',  ( 0.000000000000000000, -0.000000000000000000, 1.000000000000000000 ) ) ;
#19808 = CARTESIAN_POINT ( 'NONE',  ( -6.650000000000018119, 2.500000000000000000, -7.188010851410854052 ) ) ;
#19809 = ORIENTED_EDGE ( 'NONE', *, *, #17602, .F. ) ;
#19811 = EDGE_CURVE ( 'NONE', #74459, #115955, #44837, .T. ) ;
#19810 = DIRECTION ( 'NONE',  ( 0.000000000000000000, 1.000000000000000000, 0.000000000000000000 ) ) ;
#19812 = CARTESIAN_POINT ( 'NONE',  ( -9.150000000000009237, 2.500000000000000000, -6.495190528383297135 ) ) ;
#19813 = AXIS2_PLACEMENT_3D ( 'NONE', #54167, #31954, #93440 ) ;
#19814 = AXIS2_PLACEMENT_3D ( 'NONE', #75845, #115781, #34670 ) ;
#19815 = AXIS2_PLACEMENT_3D ( 'NONE', #46768, #4879, #74294 ) ;
#19816 = DIRECTION ( 'NONE',  ( 0.000000000000000000, 0.000000000000000000, 1.000000000000000000 ) ) ;
#19817 = CARTESIAN_POINT ( 'NONE',  ( -12.29999999999999716, 2.500000000000000000, -3.983716857408423628 ) ) ;
#19818 = DIRECTION ( 'NONE',  ( 0.000000000000000000, -0.9999939076577903929, 0.003490651415223739937 ) ) ;
#19819 = AXIS2_PLACEMENT_3D ( 'NONE', #50337, #90238, #20879 ) ;
#19820 = DIRECTION ( 'NONE',  ( -0.000000000000000000, 1.000000000000000000, -0.000000000000000000 ) ) ;
#19821 = CARTESIAN_POINT ( 'NONE',  ( -3.100000000000028511, 2.500000000000000000, -3.983716857408426293 ) ) ;
#19822 = VECTOR ( 'NONE', #92012, 1000.000000000000000 ) ;
#19823 = ORIENTED_EDGE ( 'NONE', *, *, #3542, .T. ) ;
#19824 = VERTEX_POINT ( 'NONE', #43341 ) ;
#19825 = ORIENTED_EDGE ( 'NONE', *, *, #25416, .T. ) ;
#19826 = ORIENTED_EDGE ( 'NONE', *, *, #76141, .F. ) ;
#19827 = DIRECTION ( 'NONE',  ( 0.000000000000000000, 0.000000000000000000, 1.000000000000000000 ) ) ;
#19828 = DIRECTION ( 'NONE',  ( 0.000000000000000000, 0.000000000000000000, 1.000000000000000000 ) ) ;
#19829 = CIRCLE ( 'NONE', #128518, 0.1000000000000002554 ) ;
#19830 = EDGE_CURVE ( 'NONE', #21708, #67757, #49051, .T. ) ;
#19831 = CARTESIAN_POINT ( 'NONE',  ( -5.000000000000026645, 2.500000000000000000, -3.637306695894650055 ) ) ;
#19832 = ORIENTED_EDGE ( 'NONE', *, *, #110608, .F. ) ;
#19833 = FACE_BOUND ( 'NONE', #44160, .T. ) ;
#19834 = ORIENTED_EDGE ( 'NONE', *, *, #48232, .F. ) ;
#19835 = ADVANCED_FACE ( 'NONE', ( #73419 ), #115927, .T. ) ;
#19836 = DIRECTION ( 'NONE',  ( 0.000000000000000000, 1.000000000000000000, 0.000000000000000000 ) ) ;
#19837 = DIRECTION ( 'NONE',  ( 0.000000000000000000, 1.000000000000000000, 0.000000000000000000 ) ) ;
#19838 = DIRECTION ( 'NONE',  ( 0.000000000000000000, 1.000000000000000000, 0.000000000000000000 ) ) ;
#19839 = CARTESIAN_POINT ( 'NONE',  ( 16.56576425165006583, 1.500000000000000888, -6.084390597445814564 ) ) ;
#19840 = CARTESIAN_POINT ( 'NONE',  ( -6.650000000000014566, 2.500000000000000000, 1.372243186433545370 ) ) ;
#19841 = DIRECTION ( 'NONE',  ( 0.000000000000000000, -0.9999939076577903929, 0.003490651415223739937 ) ) ;
#19842 = CARTESIAN_POINT ( 'NONE',  ( 8.549999999999918998, 12.50000000000000000, -1.818653347947326138 ) ) ;
#19843 = CARTESIAN_POINT ( 'NONE',  ( -1.700000000000034817, 2.500000000000000000, -2.385244779468109755E-15 ) ) ;
#19844 = EDGE_CURVE ( 'NONE', #110912, #113131, #61567, .T. ) ;
#19845 = CARTESIAN_POINT ( 'NONE',  ( -5.200000000000022382, 12.50000000000000000, 0.3464101615137735735 ) ) ;
#19846 = CIRCLE ( 'NONE', #93008, 0.06509327318403745899 ) ;
#19847 = DIRECTION ( 'NONE',  ( -0.000000000000000000, 1.000000000000000000, -0.000000000000000000 ) ) ;
#19848 = ORIENTED_EDGE ( 'NONE', *, *, #5057, .F. ) ;
#19849 = EDGE_LOOP ( 'NONE', ( #15029, #50328 ) ) ;
#19850 = VERTEX_POINT ( 'NONE', #64246 ) ;
#19851 = VERTEX_POINT ( 'NONE', #66176 ) ;
#19852 = DIRECTION ( 'NONE',  ( 0.000000000000000000, 1.000000000000000000, 0.000000000000000000 ) ) ;
#19853 = CARTESIAN_POINT ( 'NONE',  ( -13.74999999999998757, 12.50000000000000000, 1.407149913249511997 ) ) ;
#19855 = ORIENTED_EDGE ( 'NONE', *, *, #83231, .T. ) ;
#19854 = ORIENTED_EDGE ( 'NONE', *, *, #21646, .F. ) ;
#19856 = ORIENTED_EDGE ( 'NONE', *, *, #106676, .T. ) ;
#19857 = FACE_OUTER_BOUND ( 'NONE', #31370, .T. ) ;
#19858 = AXIS2_PLACEMENT_3D ( 'NONE', #66346, #125279, #65706 ) ;
#19859 = VECTOR ( 'NONE', #9655, 1000.000000000000000 ) ;
#19860 = CARTESIAN_POINT ( 'NONE',  ( -12.09999999999999609, 2.500000000000000000, 0.1000000000000017403 ) ) ;
#19861 = CARTESIAN_POINT ( 'NONE',  ( 5.649999999999934630, 12.50000000000000000, 6.776507416713035248 ) ) ;
#19862 = CARTESIAN_POINT ( 'NONE',  ( -4.350000000000023626, 12.50000000000000000, 2.511473670974873507 ) ) ;
#19863 = DIRECTION ( 'NONE',  ( 0.000000000000000000, 1.000000000000000000, 0.000000000000000000 ) ) ;
#19864 = DIRECTION ( 'NONE',  ( -0.000000000000000000, -1.000000000000000000, -0.000000000000000000 ) ) ;
#19865 = DIRECTION ( 'NONE',  ( 0.000000000000000000, 0.000000000000000000, -1.000000000000000000 ) ) ;
#19866 = ORIENTED_EDGE ( 'NONE', *, *, #14133, .T. ) ;
#19867 = CARTESIAN_POINT ( 'NONE',  ( -0.6500000000000389910, 2.500000000000000000, -6.148780366869526226 ) ) ;
#19868 = ORIENTED_EDGE ( 'NONE', *, *, #2323, .F. ) ;
#19869 = AXIS2_PLACEMENT_3D ( 'NONE', #127165, #69501, #70802 ) ;
#19870 = EDGE_CURVE ( 'NONE', #22721, #11513, #24971, .T. ) ;
#19871 = ORIENTED_EDGE ( 'NONE', *, *, #4506, .T. ) ;
#19872 = VERTEX_POINT ( 'NONE', #53784 ) ;
#19873 = CARTESIAN_POINT ( 'NONE',  ( 1.249999999999952482, 2.500000000000000000, -5.802370205355749988 ) ) ;
#19874 = ORIENTED_EDGE ( 'NONE', *, *, #121641, .T. ) ;
#19875 = EDGE_CURVE ( 'NONE', #37705, #4176, #75349, .T. ) ;
#19876 = ORIENTED_EDGE ( 'NONE', *, *, #84315, .T. ) ;
#19877 = ADVANCED_FACE ( 'NONE', ( #15124 ), #120046, .T. ) ;
#19878 = DIRECTION ( 'NONE',  ( -0.000000000000000000, -1.000000000000000000, -0.000000000000000000 ) ) ;
#19880 = CIRCLE ( 'NONE', #103497, 0.1000000000000000472 ) ;
#19879 = CARTESIAN_POINT ( 'NONE',  ( -1.850000000000033840, 2.500000000000000000, 2.411473670974873862 ) ) ;
#19881 = DIRECTION ( 'NONE',  ( -0.000000000000000000, -1.000000000000000000, -0.000000000000000000 ) ) ;
#19882 = CONICAL_SURFACE ( 'NONE', #47072, 0.1000000000000002554, 0.003490658503988666988 ) ;
#19883 = DIRECTION ( 'NONE',  ( 0.000000000000000000, 0.000000000000000000, -1.000000000000000000 ) ) ;
#19884 = EDGE_CURVE ( 'NONE', #19791, #55495, #72028, .T. ) ;
#19885 = FACE_OUTER_BOUND ( 'NONE', #84153, .T. ) ;
#19886 = EDGE_CURVE ( 'NONE', #81561, #47875, #43983, .T. ) ;
#19887 = ADVANCED_FACE ( 'NONE', ( #13853 ), #115918, .T. ) ;
#19888 = VERTEX_POINT ( 'NONE', #55079 ) ;
#19889 = CARTESIAN_POINT ( 'NONE',  ( -6.450000000000014388, 2.500000000000000000, 1.918653347947321564 ) ) ;
#19890 = ORIENTED_EDGE ( 'NONE', *, *, #85311, .F. ) ;
#19891 = FACE_OUTER_BOUND ( 'NONE', #54961, .T. ) ;
#19892 = EDGE_CURVE ( 'NONE', #34472, #107528, #21859, .T. ) ;
#19893 = ORIENTED_EDGE ( 'NONE', *, *, #117850, .F. ) ;
#19894 = CARTESIAN_POINT ( 'NONE',  ( 109.3219936376940495, 7.239736399353564167, 4.824898011458333968 ) ) ;
#19895 = CARTESIAN_POINT ( 'NONE',  ( 1.649999999999951950, 12.50000000000000000, -5.802370205355749988 ) ) ;
#19896 = ORIENTED_EDGE ( 'NONE', *, *, #41928, .T. ) ;
#19897 = DIRECTION ( 'NONE',  ( 0.000000000000000000, 0.000000000000000000, 1.000000000000000000 ) ) ;
#19898 = DIRECTION ( 'NONE',  ( 0.000000000000000000, 1.000000000000000000, 0.000000000000000000 ) ) ;
#19899 = CIRCLE ( 'NONE', #128679, 0.06509327318403745899 ) ;
#19900 = ORIENTED_EDGE ( 'NONE', *, *, #21955, .T. ) ;
#19901 = ADVANCED_FACE ( 'NONE', ( #54423 ), #94347, .T. ) ;
#19902 = CIRCLE ( 'NONE', #9430, 0.1000000000000002554 ) ;
#19904 = DIRECTION ( 'NONE',  ( 0.000000000000000000, 1.000000000000000000, 0.000000000000000000 ) ) ;
#19903 = CONICAL_SURFACE ( 'NONE', #109776, 0.09999999999999982514, 0.003490658503988666988 ) ;
#19905 = EDGE_LOOP ( 'NONE', ( #126154, #21488 ) ) ;
#19906 = AXIS2_PLACEMENT_3D ( 'NONE', #12585, #83904, #2124 ) ;
#19907 = ORIENTED_EDGE ( 'NONE', *, *, #42280, .T. ) ;
#19908 = CARTESIAN_POINT ( 'NONE',  ( 1.849999999999950573, 12.50000000000000000, 2.511473670974873507 ) ) ;
#19909 = LINE ( 'NONE', #119373, #65963 ) ;
#19910 = DIRECTION ( 'NONE',  ( 0.000000000000000000, -0.000000000000000000, 1.000000000000000000 ) ) ;
#19911 = DIRECTION ( 'NONE',  ( 0.000000000000000000, 1.000000000000000000, 0.000000000000000000 ) ) ;
#19912 = CARTESIAN_POINT ( 'NONE',  ( 12.69999999999990159, 12.50000000000000000, -4.048810130592463530 ) ) ;
#19913 = CONICAL_SURFACE ( 'NONE', #101473, 0.09999999999999982514, 0.003490658503988666988 ) ;
#19914 = ORIENTED_EDGE ( 'NONE', *, *, #124164, .T. ) ;
#19915 = AXIS2_PLACEMENT_3D ( 'NONE', #25036, #45976, #64944 ) ;
#19916 = DIRECTION ( 'NONE',  ( -0.000000000000000000, 1.000000000000000000, -0.000000000000000000 ) ) ;
#19917 = AXIS2_PLACEMENT_3D ( 'NONE', #11537, #118918, #61943 ) ;
#19918 = EDGE_LOOP ( 'NONE', ( #27382, #128493, #96272, #87917 ) ) ;
#19919 = CIRCLE ( 'NONE', #49180, 0.09999999999999982514 ) ;
#19920 = CARTESIAN_POINT ( 'NONE',  ( 6.849999999999929479, 2.500000000000000000, 6.248780366869520542 ) ) ;
#19922 = CIRCLE ( 'NONE', #30402, 0.09999999999999999167 ) ;
#19921 = DIRECTION ( 'NONE',  ( -0.000000000000000000, 1.000000000000000000, -0.000000000000000000 ) ) ;
#19923 = CONICAL_SURFACE ( 'NONE', #30404, 0.09999999999999982514, 0.003490658503988666988 ) ;
#19924 = CARTESIAN_POINT ( 'NONE',  ( 3.749999999999944045, 2.500000000000000000, -7.188010851410854052 ) ) ;
#19925 = CARTESIAN_POINT ( 'NONE',  ( 12.09999999999990195, 12.50000000000000000, -2.276824562219559311E-15 ) ) ;
#19926 = DIRECTION ( 'NONE',  ( 0.000000000000000000, -0.9999939076577903929, 0.003490651415223739937 ) ) ;
#19927 = CARTESIAN_POINT ( 'NONE',  ( -14.99999999999994671, 2.500000000000000000, 0.000000000000000000 ) ) ;
#19928 = PLANE ( 'NONE',  #36987 ) ;
#19929 = ORIENTED_EDGE ( 'NONE', *, *, #79605, .F. ) ;
#19931 = EDGE_CURVE ( 'NONE', #57931, #30852, #5097, .T. ) ;
#19930 = DIRECTION ( 'NONE',  ( -0.000000000000000000, -1.000000000000000000, -0.000000000000000000 ) ) ;
#19932 = DIRECTION ( 'NONE',  ( 0.000000000000000000, 0.000000000000000000, 1.000000000000000000 ) ) ;
#19933 = CARTESIAN_POINT ( 'NONE',  ( 12.94999999999990337, 2.500000000000000000, 2.265063509461097357 ) ) ;
#19934 = CONICAL_SURFACE ( 'NONE', #36671, 0.1000000000000002554, 0.003490658503988666988 ) ;
#19935 = ORIENTED_EDGE ( 'NONE', *, *, #115256, .F. ) ;
#19936 = DIRECTION ( 'NONE',  ( -0.000000000000000000, 1.000000000000000000, -0.000000000000000000 ) ) ;
#19937 = ADVANCED_FACE ( 'NONE', ( #74718 ), #19785, .T. ) ;
#19938 = ORIENTED_EDGE ( 'NONE', *, *, #80631, .T. ) ;
#19939 = EDGE_LOOP ( 'NONE', ( #122924, #81227 ) ) ;
#19940 = LINE ( 'NONE', #938, #23833 ) ;
#19941 = AXIS2_PLACEMENT_3D ( 'NONE', #64251, #106116, #104182 ) ;
#19942 = ORIENTED_EDGE ( 'NONE', *, *, #43455, .T. ) ;
#19943 = CARTESIAN_POINT ( 'NONE',  ( -5.400000000000019895, 12.50000000000000000, 4.265033745738159077 ) ) ;
#19944 = DIRECTION ( 'NONE',  ( 0.000000000000000000, 1.000000000000000000, 0.000000000000000000 ) ) ;
#19945 = CONICAL_SURFACE ( 'NONE', #57601, 0.1000000000000002554, 0.003490658503988666988 ) ;
#19946 = CIRCLE ( 'NONE', #70123, 0.06509327318403745899 ) ;
#19947 = EDGE_LOOP ( 'NONE', ( #36102, #4181 ) ) ;
#19948 = FACE_OUTER_BOUND ( 'NONE', #15952, .T. ) ;
#19949 = CARTESIAN_POINT ( 'NONE',  ( 3.949999999999941558, 2.500000000000000000, -1.818653347947326138 ) ) ;
#19950 = CARTESIAN_POINT ( 'NONE',  ( 10.59999999999990905, 2.500000000000000000, -4.083716857408426826 ) ) ;
#19951 = ORIENTED_EDGE ( 'NONE', *, *, #4954, .F. ) ;
#19952 = CIRCLE ( 'NONE', #28270, 0.06509327318403745899 ) ;
#19953 = VERTEX_POINT ( 'NONE', #95011 ) ;
#19954 = AXIS2_PLACEMENT_3D ( 'NONE', #110449, #41098, #20792 ) ;
#19955 = VERTEX_POINT ( 'NONE', #5322 ) ;
#19956 = DIRECTION ( 'NONE',  ( -4.274815082592931898E-19, -0.9999939076577903929, -0.003490651415223739937 ) ) ;
#19957 = DIRECTION ( 'NONE',  ( 0.000000000000000000, 1.000000000000000000, 0.000000000000000000 ) ) ;
#19958 = CARTESIAN_POINT ( 'NONE',  ( 5.399999999999936406, 12.50000000000000000, -3.572213422710612374 ) ) ;
#19959 = FACE_BOUND ( 'NONE', #49605, .T. ) ;
#19960 = VERTEX_POINT ( 'NONE', #45267 ) ;
#19961 = CARTESIAN_POINT ( 'NONE',  ( 5.449999999999934452, 2.500000000000000000, 2.165063509461097713 ) ) ;
#19962 = DIRECTION ( 'NONE',  ( 0.000000000000000000, 1.000000000000000000, 0.000000000000000000 ) ) ;
#19963 = EDGE_LOOP ( 'NONE', ( #39598, #124135, #91560, #67490 ) ) ;
#19965 = EDGE_CURVE ( 'NONE', #95189, #60634, #84528, .T. ) ;
#19964 = DIRECTION ( 'NONE',  ( 0.000000000000000000, 0.000000000000000000, 1.000000000000000000 ) ) ;
#19967 = FACE_OUTER_BOUND ( 'NONE', #126411, .T. ) ;
#19966 = CONICAL_SURFACE ( 'NONE', #78563, 0.09999999999999982514, 0.003490658503988666988 ) ;
#19968 = CONICAL_SURFACE ( 'NONE', #61752, 0.09999999999999982514, 0.003490658503988666988 ) ;
#19969 = CARTESIAN_POINT ( 'NONE',  ( 3.149999999999946176, 2.500000000000000000, -6.148780366869526226 ) ) ;
#19970 = DIRECTION ( 'NONE',  ( 0.000000000000000000, 0.000000000000000000, 1.000000000000000000 ) ) ;
#19971 = PLANE ( 'NONE',  #13102 ) ;
#19972 = FACE_OUTER_BOUND ( 'NONE', #70764, .T. ) ;
#19973 = CARTESIAN_POINT ( 'NONE',  ( 187.5000000000000000, 0.000000000000000000, 0.000000000000000000 ) ) ;
#19974 = EDGE_CURVE ( 'NONE', #92776, #34089, #15785, .T. ) ;
#19975 = ORIENTED_EDGE ( 'NONE', *, *, #118115, .F. ) ;
#19976 = ORIENTED_EDGE ( 'NONE', *, *, #44728, .T. ) ;
#19977 = EDGE_LOOP ( 'NONE', ( #83533, #81975, #9263, #123466 ) ) ;
#19978 = AXIS2_PLACEMENT_3D ( 'NONE', #111774, #109173, #10344 ) ;
#19979 = ORIENTED_EDGE ( 'NONE', *, *, #54583, .F. ) ;
#19980 = ORIENTED_EDGE ( 'NONE', *, *, #51749, .T. ) ;
#19981 = DIRECTION ( 'NONE',  ( 0.000000000000000000, 1.000000000000000000, 0.000000000000000000 ) ) ;
#19982 = EDGE_CURVE ( 'NONE', #60636, #66637, #96271, .T. ) ;
#19983 = DIRECTION ( 'NONE',  ( 0.000000000000000000, 0.000000000000000000, -1.000000000000000000 ) ) ;
#19984 = ORIENTED_EDGE ( 'NONE', *, *, #42754, .F. ) ;
#19985 = FACE_BOUND ( 'NONE', #81919, .T. ) ;
#19986 = EDGE_CURVE ( 'NONE', #67674, #17430, #103413, .T. ) ;
#19987 = VECTOR ( 'NONE', #101981, 1000.000000000000000 ) ;
#19988 = FACE_OUTER_BOUND ( 'NONE', #81893, .T. ) ;
#19989 = CIRCLE ( 'NONE', #22156, 0.1000000000000000472 ) ;
#19990 = EDGE_CURVE ( 'NONE', #125138, #74230, #61647, .T. ) ;
#19991 = CARTESIAN_POINT ( 'NONE',  ( 0.3999999999999619971, 12.50000000000000000, -1.084202172485504434E-16 ) ) ;
#19992 = CIRCLE ( 'NONE', #126606, 0.06509327318403745899 ) ;
#19993 = CARTESIAN_POINT ( 'NONE',  ( 12.04999999999990479, 2.500000000000000000, 2.265063509461097357 ) ) ;
#19994 = DIRECTION ( 'NONE',  ( -0.000000000000000000, -1.000000000000000000, -0.000000000000000000 ) ) ;
#19995 =( BOUNDED_CURVE ( )  B_SPLINE_CURVE ( 2, ( #58438, #119265, #118624, #40076, #57127, #49911, #88512 ),
 .UNSPECIFIED., .F., .F. ) 
 B_SPLINE_CURVE_WITH_KNOTS ( ( 3, 2, 2, 3 ),
 ( 0.5000000000000004441, 0.5238095238095242800, 0.5476190476190482270, 0.5714285714285719520 ),
 .UNSPECIFIED. ) 
 CURVE ( )  GEOMETRIC_REPRESENTATION_ITEM ( )  RATIONAL_B_SPLINE_CURVE ( ( 0.9999999999999974465, 0.8660254037844412611, 1.000000000000000000, 0.8660254037844387076, 1.000000000000000000, 0.8660254037844355990, 1.000000000000003109 ) ) 
 REPRESENTATION_ITEM ( '' )  );
#19996 = DIRECTION ( 'NONE',  ( -0.000000000000000000, -1.000000000000000000, -0.000000000000000000 ) ) ;
#19997 = EDGE_CURVE ( 'NONE', #30351, #71261, #40732, .T. ) ;
#19998 = DIRECTION ( 'NONE',  ( -0.000000000000000000, 1.000000000000000000, -0.000000000000000000 ) ) ;
#19999 = EDGE_LOOP ( 'NONE', ( #74108, #74327 ) ) ;
#20000 = CONICAL_SURFACE ( 'NONE', #126612, 0.1000000000000002554, 0.003490658503988666988 ) ;
#20001 = ORIENTED_EDGE ( 'NONE', *, *, #106874, .F. ) ;
#20002 = ORIENTED_EDGE ( 'NONE', *, *, #106424, .T. ) ;
#20003 = VERTEX_POINT ( 'NONE', #118498 ) ;
#20004 = ORIENTED_EDGE ( 'NONE', *, *, #2117, .F. ) ;
#20005 = ORIENTED_EDGE ( 'NONE', *, *, #65374, .F. ) ;
#20006 = VECTOR ( 'NONE', #38283, 1000.000000000000000 ) ;
#20007 = DIRECTION ( 'NONE',  ( -1.000000000000000000, 0.000000000000000000, 1.224646799147352221E-16 ) ) ;
#20008 = DIRECTION ( 'NONE',  ( 0.000000000000000000, 1.000000000000000000, 0.000000000000000000 ) ) ;
#20009 = ORIENTED_EDGE ( 'NONE', *, *, #38190, .F. ) ;
#20010 = CARTESIAN_POINT ( 'NONE',  ( 6.249999999999968914, 2.500000000000000000, -6.495190528383302464 ) ) ;
#20011 = CIRCLE ( 'NONE', #91017, 0.1000000000000002554 ) ;
#20012 = DIRECTION ( 'NONE',  ( -0.000000000000000000, -1.000000000000000000, -0.000000000000000000 ) ) ;
#20013 = CONICAL_SURFACE ( 'NONE', #93179, 0.09999999999999999167, 0.003490658503988666988 ) ;
#20014 = DIRECTION ( 'NONE',  ( 0.000000000000000000, 1.000000000000000000, 0.000000000000000000 ) ) ;
#20015 = CARTESIAN_POINT ( 'NONE',  ( 185.7760416670080588, 6.551208109652274736, 3.782341765625001351 ) ) ;
#20016 = DIRECTION ( 'NONE',  ( 0.000000000000000000, 0.000000000000000000, 1.000000000000000000 ) ) ;
#20018 = VECTOR ( 'NONE', #11838, 1000.000000000000000 ) ;
#20017 = DIRECTION ( 'NONE',  ( 0.000000000000000000, 1.000000000000000000, 0.000000000000000000 ) ) ;
#20019 = CARTESIAN_POINT ( 'NONE',  ( -13.34999999999999076, 2.500000000000000000, 2.165063509461101265 ) ) ;
#20020 = ORIENTED_EDGE ( 'NONE', *, *, #88840, .F. ) ;
#20021 = CARTESIAN_POINT ( 'NONE',  ( -12.29999999999999538, 2.500000000000000000, -0.3464101615137741841 ) ) ;
#20022 = EDGE_LOOP ( 'NONE', ( #65956, #15152, #98745, #49067 ) ) ;
#20023 = EDGE_CURVE ( 'NONE', #52300, #25799, #44634, .T. ) ;
#20024 = VERTEX_POINT ( 'NONE', #17042 ) ;
#20025 = CARTESIAN_POINT ( 'NONE',  ( -3.950000000000028155, 12.50000000000000000, -6.906693963081115051 ) ) ;
#20026 = DIRECTION ( 'NONE',  ( -0.000000000000000000, -1.000000000000000000, -0.000000000000000000 ) ) ;
#20027 = CARTESIAN_POINT ( 'NONE',  ( -0.2000000000000404232, 2.500000000000000000, 3.983716857408420964 ) ) ;
#20028 = AXIS2_PLACEMENT_3D ( 'NONE', #4497, #54913, #94850 ) ;
#20029 = ORIENTED_EDGE ( 'NONE', *, *, #18224, .F. ) ;
#20031 = EDGE_CURVE ( 'NONE', #94655, #32380, #58953, .T. ) ;
#20030 = VERTEX_POINT ( 'NONE', #39333 ) ;
#20032 = CARTESIAN_POINT ( 'NONE',  ( 5.849999999999935696, 12.50000000000000000, -6.495190528383302464 ) ) ;
#20033 = CARTESIAN_POINT ( 'NONE',  ( 9.599999999999914380, 12.50000000000000000, 4.957854068765711553 ) ) ;
#20034 = DIRECTION ( 'NONE',  ( 0.000000000000000000, 1.000000000000000000, 0.000000000000000000 ) ) ;
#20035 = DIRECTION ( 'NONE',  ( -0.000000000000000000, -1.000000000000000000, -0.000000000000000000 ) ) ;
#20036 = EDGE_LOOP ( 'NONE', ( #97838, #87852, #44093, #23758 ) ) ;
#20037 = ADVANCED_FACE ( 'NONE', ( #117842 ), #90589, .T. ) ;
#20038 = LINE ( 'NONE', #118225, #79532 ) ;
#20039 = CIRCLE ( 'NONE', #26299, 0.1000000000000002554 ) ;
#20040 = EDGE_CURVE ( 'NONE', #2801, #27444, #17706, .T. ) ;
#20041 = VECTOR ( 'NONE', #77437, 1000.000000000000000 ) ;
#20042 = EDGE_CURVE ( 'NONE', #28525, #53869, #21652, .T. ) ;
#20043 = EDGE_LOOP ( 'NONE', ( #102926, #47898, #111579, #61654 ) ) ;
#20045 = AXIS2_PLACEMENT_3D ( 'NONE', #59917, #58614, #22565 ) ;
#20044 = LINE ( 'NONE', #99891, #1836 ) ;
#20046 = EDGE_LOOP ( 'NONE', ( #79737, #10232 ) ) ;
#20047 = CIRCLE ( 'NONE', #61909, 0.09999999999999999167 ) ;
#20048 = CARTESIAN_POINT ( 'NONE',  ( 8.099999999999923261, 2.500000000000000000, -4.083716857408426826 ) ) ;
#20049 = EDGE_CURVE ( 'NONE', #85597, #91594, #7898, .T. ) ;
#20050 = FACE_OUTER_BOUND ( 'NONE', #38631, .T. ) ;
#20051 = DIRECTION ( 'NONE',  ( -1.000000000000000000, -0.000000000000000000, -0.000000000000000000 ) ) ;
#20052 = DIRECTION ( 'NONE',  ( -0.000000000000000000, 1.000000000000000000, -0.000000000000000000 ) ) ;
#20053 = ORIENTED_EDGE ( 'NONE', *, *, #112275, .T. ) ;
#20054 = EDGE_CURVE ( 'NONE', #62991, #118696, #5188, .T. ) ;
#20055 = CONICAL_SURFACE ( 'NONE', #120395, 0.1000000000000002554, 0.003490658503988666988 ) ;
#20056 = LINE ( 'NONE', #21999, #21731 ) ;
#20057 = ADVANCED_FACE ( 'NONE', ( #68757 ), #46983, .T. ) ;
#20059 = CIRCLE ( 'NONE', #116172, 0.06509327318403745899 ) ;
#20058 = CIRCLE ( 'NONE', #24250, 0.1000000000000000472 ) ;
#20060 = ORIENTED_EDGE ( 'NONE', *, *, #89382, .T. ) ;
#20061 = ORIENTED_EDGE ( 'NONE', *, *, #33345, .T. ) ;
#20062 = CARTESIAN_POINT ( 'NONE',  ( -12.04999999999999716, 12.50000000000000000, -2.230156782645135394 ) ) ;
#20063 = DIRECTION ( 'NONE',  ( 0.000000000000000000, -0.9999939076577903929, 0.003490651415223739937 ) ) ;
#20064 = CARTESIAN_POINT ( 'NONE',  ( -4.150000000000025224, 12.50000000000000000, -1.472243186433550122 ) ) ;
#20065 = SURFACE_SIDE_STYLE ('',( #11517 ) ) ;
#20066 = CARTESIAN_POINT ( 'NONE',  ( 7.299999999999927880, 2.500000000000000000, 4.083716857408421497 ) ) ;
#20067 = FACE_OUTER_BOUND ( 'NONE', #45786, .T. ) ;
#20068 = VECTOR ( 'NONE', #125122, 1000.000000000000000 ) ;
#20069 = LINE ( 'NONE', #80918, #42732 ) ;
#20070 = LINE ( 'NONE', #110990, #47025 ) ;
#20071 = DIRECTION ( 'NONE',  ( -0.000000000000000000, -1.000000000000000000, -0.000000000000000000 ) ) ;
#20072 = ORIENTED_EDGE ( 'NONE', *, *, #111544, .F. ) ;
#20073 = DIRECTION ( 'NONE',  ( 0.000000000000000000, 1.000000000000000000, 0.000000000000000000 ) ) ;
#20074 = FACE_OUTER_BOUND ( 'NONE', #108974, .T. ) ;
#20075 = DIRECTION ( 'NONE',  ( 0.000000000000000000, 0.000000000000000000, 1.000000000000000000 ) ) ;
#20076 = CARTESIAN_POINT ( 'NONE',  ( -7.100000000000017408, 12.50000000000000000, -3.637306695894650055 ) ) ;
#20077 = FACE_OUTER_BOUND ( 'NONE', #63138, .T. ) ;
#20078 = EDGE_LOOP ( 'NONE', ( #106370, #21078 ) ) ;
#20079 = DIRECTION ( 'NONE',  ( 0.000000000000000000, -0.9999939076577903929, 0.003490651415223739937 ) ) ;
#20080 = CONICAL_SURFACE ( 'NONE', #59822, 0.09999999999999999167, 0.003490658503988666988 ) ;
#20081 = EDGE_CURVE ( 'NONE', #96072, #46924, #111826, .T. ) ;
#20082 = AXIS2_PLACEMENT_3D ( 'NONE', #62893, #21686, #32162 ) ;
#20083 = CARTESIAN_POINT ( 'NONE',  ( 1.849999999999950573, 2.500000000000000000, 2.611473670974873151 ) ) ;
#20085 = ORIENTED_EDGE ( 'NONE', *, *, #89308, .F. ) ;
#20084 = CARTESIAN_POINT ( 'NONE',  ( 0.3999999999999628852, 2.500000000000000000, 0.7928203230275517877 ) ) ;
#20086 = ORIENTED_EDGE ( 'NONE', *, *, #126692, .F. ) ;
#20087 = AXIS2_PLACEMENT_3D ( 'NONE', #71150, #109125, #129463 ) ;
#20088 = DIRECTION ( 'NONE',  ( -0.000000000000000000, 1.000000000000000000, -0.000000000000000000 ) ) ;
#20089 = EDGE_CURVE ( 'NONE', #89954, #48809, #88529, .T. ) ;
#20090 = EDGE_LOOP ( 'NONE', ( #45943, #86642, #53501, #6429 ) ) ;
#20091 = ORIENTED_EDGE ( 'NONE', *, *, #99667, .T. ) ;
#20092 = CARTESIAN_POINT ( 'NONE',  ( -6.250000000000015987, 2.500000000000000000, 5.802370205355744659 ) ) ;
#20093 = LINE ( 'NONE', #89473, #27972 ) ;
#20094 = CARTESIAN_POINT ( 'NONE',  ( 9.599999999999914380, 2.500000000000000000, 4.430127018922196847 ) ) ;
#20095 = VECTOR ( 'NONE', #105552, 1000.000000000000000 ) ;
#20096 = DIRECTION ( 'NONE',  ( -0.000000000000000000, 1.000000000000000000, -0.000000000000000000 ) ) ;
#20097 = ORIENTED_EDGE ( 'NONE', *, *, #62845, .T. ) ;
#20098 = AXIS2_PLACEMENT_3D ( 'NONE', #84573, #74758, #63656 ) ;
#20099 = DIRECTION ( 'NONE',  ( 0.000000000000000000, 0.000000000000000000, -1.000000000000000000 ) ) ;
#20100 = VERTEX_POINT ( 'NONE', #127678 ) ;
#20101 = CARTESIAN_POINT ( 'NONE',  ( 184.5000000000000000, 6.368163355566236381E-16, 5.200000000000000178 ) ) ;
#20102 = DIRECTION ( 'NONE',  ( -0.000000000000000000, -1.000000000000000000, -0.000000000000000000 ) ) ;
#20103 = FACE_OUTER_BOUND ( 'NONE', #14264, .T. ) ;
#20104 = ORIENTED_EDGE ( 'NONE', *, *, #70522, .F. ) ;
#20105 = VERTEX_POINT ( 'NONE', #79242 ) ;
#20106 = ORIENTED_EDGE ( 'NONE', *, *, #341, .T. ) ;
#20107 = ORIENTED_EDGE ( 'NONE', *, *, #82061, .F. ) ;
#20108 = EDGE_LOOP ( 'NONE', ( #93169, #2353 ) ) ;
#20109 = DIRECTION ( 'NONE',  ( -0.000000000000000000, -1.000000000000000000, -0.000000000000000000 ) ) ;
#20110 = CARTESIAN_POINT ( 'NONE',  ( 1.699999999999950218, 2.500000000000000000, 4.230127018922196669 ) ) ;
#20111 = FACE_OUTER_BOUND ( 'NONE', #37115, .T. ) ;
#20112 = FACE_BOUND ( 'NONE', #27970, .T. ) ;
#20113 = DIRECTION ( 'NONE',  ( 0.000000000000000000, -0.000000000000000000, 1.000000000000000000 ) ) ;
#20114 = AXIS2_PLACEMENT_3D ( 'NONE', #62818, #83742, #101450 ) ;
#20115 = CARTESIAN_POINT ( 'NONE',  ( 186.5312500006828031, 9.429780353434619030E-16, -7.700000000000000178 ) ) ;
#20116 = LINE ( 'NONE', #60063, #51106 ) ;
#20117 = DIRECTION ( 'NONE',  ( -4.274815082592931898E-19, -0.9999939076577903929, -0.003490651415223739937 ) ) ;
#20118 = CIRCLE ( 'NONE', #16169, 2.000000000000000000 ) ;
#20119 = DIRECTION ( 'NONE',  ( 0.000000000000000000, 0.000000000000000000, -1.000000000000000000 ) ) ;
#20120 = VECTOR ( 'NONE', #96767, 1000.000000000000000 ) ;
#20121 = DIRECTION ( 'NONE',  ( -0.000000000000000000, 1.000000000000000000, -0.000000000000000000 ) ) ;
#20122 = CARTESIAN_POINT ( 'NONE',  ( 13.74999999999993427, 2.500000000000000000, 2.165063509461097713 ) ) ;
#20123 = AXIS2_PLACEMENT_3D ( 'NONE', #90142, #121545, #19484 ) ;
#20124 = CIRCLE ( 'NONE', #91229, 0.1000000000000002554 ) ;
#20125 = EDGE_CURVE ( 'NONE', #13873, #89102, #36745, .T. ) ;
#20126 = CARTESIAN_POINT ( 'NONE',  ( 8.949999999999915801, 12.50000000000000000, 6.841600689897072485 ) ) ;
#20127 = ORIENTED_EDGE ( 'NONE', *, *, #64344, .T. ) ;
#20128 = ORIENTED_EDGE ( 'NONE', *, *, #38799, .F. ) ;
#20129 = ORIENTED_EDGE ( 'NONE', *, *, #92792, .T. ) ;
#20130 = ORIENTED_EDGE ( 'NONE', *, *, #81802, .F. ) ;
#20131 = FACE_OUTER_BOUND ( 'NONE', #107303, .T. ) ;
#20132 = ADVANCED_FACE ( 'NONE', ( #18365 ), #14978, .F. ) ;
#20133 = DIRECTION ( 'NONE',  ( 0.000000000000000000, -0.000000000000000000, 1.000000000000000000 ) ) ;
#20134 = FACE_BOUND ( 'NONE', #89518, .T. ) ;
#20135 = ADVANCED_FACE ( 'NONE', ( #122230 ), #78380, .T. ) ;
#20137 = DIRECTION ( 'NONE',  ( 0.000000000000000000, 0.000000000000000000, 1.000000000000000000 ) ) ;
#20136 = CIRCLE ( 'NONE', #93294, 0.1000000000000000472 ) ;
#20139 = VECTOR ( 'NONE', #31436, 1000.000000000000000 ) ;
#20138 = AXIS2_PLACEMENT_3D ( 'NONE', #78479, #119656, #128875 ) ;
#20140 = EDGE_CURVE ( 'NONE', #81254, #78428, #11170, .T. ) ;
#20141 = EDGE_CURVE ( 'NONE', #117403, #71756, #78078, .T. ) ;
#20142 = VERTEX_POINT ( 'NONE', #42375 ) ;
#20143 = CARTESIAN_POINT ( 'NONE',  ( -5.650000000000019895, 2.500000000000000000, 6.248780366869520542 ) ) ;
#20144 = DIRECTION ( 'NONE',  ( 0.000000000000000000, -0.000000000000000000, 1.000000000000000000 ) ) ;
#20145 = CARTESIAN_POINT ( 'NONE',  ( -3.749999999999991118, 2.500000000000000000, 2.265063509461097357 ) ) ;
#20146 = EDGE_CURVE ( 'NONE', #64905, #101430, #109984, .T. ) ;
#20147 = FACE_OUTER_BOUND ( 'NONE', #13145, .T. ) ;
#20148 = VERTEX_POINT ( 'NONE', #23352 ) ;
#20149 = CARTESIAN_POINT ( 'NONE',  ( 6.849999999999930367, 2.500000000000000000, -6.741600689897078169 ) ) ;
#20150 = VERTEX_POINT ( 'NONE', #63292 ) ;
#20151 = ORIENTED_EDGE ( 'NONE', *, *, #16884, .T. ) ;
#20152 = DIRECTION ( 'NONE',  ( -4.274815082592931898E-19, -0.9999939076577903929, -0.003490651415223739937 ) ) ;
#20153 = DIRECTION ( 'NONE',  ( 0.000000000000000000, 1.000000000000000000, 0.000000000000000000 ) ) ;
#20154 = ORIENTED_EDGE ( 'NONE', *, *, #121793, .F. ) ;
#20155 = DIRECTION ( 'NONE',  ( -0.000000000000000000, -1.000000000000000000, -0.000000000000000000 ) ) ;
#20156 = CARTESIAN_POINT ( 'NONE',  ( 4.549999999999935874, 2.500000000000000000, 6.595190528383296780 ) ) ;
#20157 = DIRECTION ( 'NONE',  ( 0.000000000000000000, 0.000000000000000000, 1.000000000000000000 ) ) ;
#20158 = ORIENTED_EDGE ( 'NONE', *, *, #29732, .T. ) ;
#20159 = CARTESIAN_POINT ( 'NONE',  ( 2.499999999999983569, 12.50000000000000000, -2.276824562219559311E-15 ) ) ;
#20160 = VERTEX_POINT ( 'NONE', #9843 ) ;
#20161 = DIRECTION ( 'NONE',  ( 0.000000000000000000, -0.9999939076577903929, 0.003490651415223739937 ) ) ;
#20162 = CIRCLE ( 'NONE', #89211, 0.06509327318403745899 ) ;
#20163 = ORIENTED_EDGE ( 'NONE', *, *, #31031, .F. ) ;
#20164 = AXIS2_PLACEMENT_3D ( 'NONE', #88976, #128931, #122316 ) ;
#20165 = CARTESIAN_POINT ( 'NONE',  ( 112.9585241711788512, 7.673121854575822631, 0.6644401856000232698 ) ) ;
#20166 = VERTEX_POINT ( 'NONE', #20313 ) ;
#20167 = DIRECTION ( 'NONE',  ( -0.000000000000000000, -1.000000000000000000, -0.000000000000000000 ) ) ;
#20168 = FACE_OUTER_BOUND ( 'NONE', #112177, .T. ) ;
#20169 = FACE_OUTER_BOUND ( 'NONE', #17298, .T. ) ;
#20170 = CARTESIAN_POINT ( 'NONE',  ( 10.64999999999990976, 12.50000000000000000, -6.083687093685488989 ) ) ;
#20171 = CARTESIAN_POINT ( 'NONE',  ( 15.19999999999989271, 2.500000000000000000, -0.3464101615137783474 ) ) ;
#20172 = EDGE_LOOP ( 'NONE', ( #115003, #15706 ) ) ;
#20174 = ORIENTED_EDGE ( 'NONE', *, *, #20354, .T. ) ;
#20173 = CIRCLE ( 'NONE', #41125, 0.1000000000000002554 ) ;
#20175 = EDGE_LOOP ( 'NONE', ( #117069, #2772 ) ) ;
#20176 = DIRECTION ( 'NONE',  ( 0.000000000000000000, 0.000000000000000000, -1.000000000000000000 ) ) ;
#20177 = DIRECTION ( 'NONE',  ( 0.000000000000000000, 0.000000000000000000, 1.000000000000000000 ) ) ;
#20179 = ADVANCED_FACE ( 'NONE', ( #24666 ), #93404, .T. ) ;
#20178 = CARTESIAN_POINT ( 'NONE',  ( -2.500000000000030642, 2.500000000000000000, -0.7928203230275542301 ) ) ;
#20181 = EDGE_LOOP ( 'NONE', ( #81629, #39152, #9003, #55222 ) ) ;
#20180 = ORIENTED_EDGE ( 'NONE', *, *, #120229, .F. ) ;
#20182 = EDGE_LOOP ( 'NONE', ( #19781, #113688, #116455, #36198 ) ) ;
#20183 = EDGE_CURVE ( 'NONE', #124893, #96482, #50898, .T. ) ;
#20184 = CARTESIAN_POINT ( 'NONE',  ( -8.750000000000008882, 2.500000000000000000, 1.572243186433545548 ) ) ;
#20185 = EDGE_CURVE ( 'NONE', #99762, #7788, #124341, .T. ) ;
#20187 = CIRCLE ( 'NONE', #80834, 0.1000000000000002554 ) ;
#20186 = AXIS2_PLACEMENT_3D ( 'NONE', #73997, #13773, #123101 ) ;
#20188 = ORIENTED_EDGE ( 'NONE', *, *, #112422, .T. ) ;
#20189 = PLANE ( 'NONE',  #27653 ) ;
#20190 = AXIS2_PLACEMENT_3D ( 'NONE', #62846, #83145, #92962 ) ;
#20191 = CARTESIAN_POINT ( 'NONE',  ( 1.049999999999954525, 12.50000000000000000, -2.511473670974877948 ) ) ;
#20192 = CARTESIAN_POINT ( 'NONE',  ( -8.150000000000014566, 2.500000000000000000, -6.248780366869521430 ) ) ;
#20193 = DIRECTION ( 'NONE',  ( 0.000000000000000000, 1.000000000000000000, 0.000000000000000000 ) ) ;
#20194 = CARTESIAN_POINT ( 'NONE',  ( 14.39999999999989555, 12.50000000000000000, -0.2813168883297408329 ) ) ;
#20195 = CARTESIAN_POINT ( 'NONE',  ( 195.5000000000000000, 4.592425496802573972E-16, 3.500000000000000000 ) ) ;
#20196 = EDGE_CURVE ( 'NONE', #47163, #110508, #120139, .T. ) ;
#20197 = EDGE_CURVE ( 'NONE', #59583, #93582, #84629, .T. ) ;
#20198 = DIRECTION ( 'NONE',  ( -1.000000000000000000, 0.000000000000000000, 0.000000000000000000 ) ) ;
#20199 = EDGE_CURVE ( 'NONE', #13310, #113079, #124145, .T. ) ;
#20200 = ORIENTED_EDGE ( 'NONE', *, *, #341, .F. ) ;
#20202 = ORIENTED_EDGE ( 'NONE', *, *, #76457, .F. ) ;
#20201 = EDGE_CURVE ( 'NONE', #43211, #112979, #7235, .T. ) ;
#20203 = CARTESIAN_POINT ( 'NONE',  ( -12.29999999999999716, 2.500000000000000000, 0.2464101615137776757 ) ) ;
#20204 = EDGE_CURVE ( 'NONE', #26160, #1788, #113876, .T. ) ;
#20205 = ORIENTED_EDGE ( 'NONE', *, *, #43829, .T. ) ;
#20206 = ORIENTED_EDGE ( 'NONE', *, *, #122870, .F. ) ;
#20207 = CARTESIAN_POINT ( 'NONE',  ( 185.1510416670080872, 4.367472073101518859, -7.564683531249999149 ) ) ;
#20208 = DIRECTION ( 'NONE',  ( 0.000000000000000000, -0.9999939076577903929, 0.003490651415223739937 ) ) ;
#20209 = CIRCLE ( 'NONE', #22280, 0.06509327318403745899 ) ;
#20210 = CARTESIAN_POINT ( 'NONE',  ( -3.100000000000028511, 12.50000000000000000, -4.611443907251939756 ) ) ;
#20211 = EDGE_CURVE ( 'NONE', #45293, #114782, #32135, .T. ) ;
#20212 = AXIS2_PLACEMENT_3D ( 'NONE', #117352, #49322, #78119 ) ;
#20213 = CARTESIAN_POINT ( 'NONE',  ( 15.59999999999988951, 12.50000000000000000, 0.2813168883297361700 ) ) ;
#20214 = DIRECTION ( 'NONE',  ( -0.000000000000000000, -1.000000000000000000, -0.000000000000000000 ) ) ;
#20215 = CIRCLE ( 'NONE', #15983, 0.1000000000000002554 ) ;
#20216 = CARTESIAN_POINT ( 'NONE',  ( -8.750000000000008882, 2.500000000000000000, 1.472243186433545459 ) ) ;
#20217 = CARTESIAN_POINT ( 'NONE',  ( 9.149999999999920419, 12.50000000000000000, -7.188010851410854052 ) ) ;
#20218 = AXIS2_PLACEMENT_3D ( 'NONE', #24009, #83583, #35135 ) ;
#20219 = CIRCLE ( 'NONE', #74683, 0.06509327318403745899 ) ;
#20220 = DIRECTION ( 'NONE',  ( -0.000000000000000000, -1.000000000000000000, -0.000000000000000000 ) ) ;
#20221 = VERTEX_POINT ( 'NONE', #84212 ) ;
#20222 = AXIS2_PLACEMENT_3D ( 'NONE', #66641, #107216, #85645 ) ;
#20223 = EDGE_LOOP ( 'NONE', ( #91936, #128985, #79393, #115592 ) ) ;
#20224 = VERTEX_POINT ( 'NONE', #52829 ) ;
#20225 = AXIS2_PLACEMENT_3D ( 'NONE', #34017, #64115, #114499 ) ;
#20226 = ORIENTED_EDGE ( 'NONE', *, *, #95489, .T. ) ;
#20227 = CARTESIAN_POINT ( 'NONE',  ( -14.39999999999998614, 12.50000000000000000, 0.2813168883297384459 ) ) ;
#20228 = CARTESIAN_POINT ( 'NONE',  ( 11.64999999999990443, 12.50000000000000000, 2.792790559304612064 ) ) ;
#20229 = VECTOR ( 'NONE', #31869, 1000.000000000000000 ) ;
#20230 = ORIENTED_EDGE ( 'NONE', *, *, #55766, .F. ) ;
#20231 = DIRECTION ( 'NONE',  ( -0.000000000000000000, -1.000000000000000000, -0.000000000000000000 ) ) ;
#20232 = CARTESIAN_POINT ( 'NONE',  ( -6.249999999999981348, 2.500000000000000000, 6.495190528383297135 ) ) ;
#20234 = AXIS2_PLACEMENT_3D ( 'NONE', #53787, #123805, #95650 ) ;
#20233 = AXIS2_PLACEMENT_3D ( 'NONE', #99885, #128724, #59332 ) ;
#20235 = CARTESIAN_POINT ( 'NONE',  ( 3.549999999999940314, 2.500000000000000000, 6.741600689897071952 ) ) ;
#20237 = ORIENTED_EDGE ( 'NONE', *, *, #26631, .F. ) ;
#20236 = CARTESIAN_POINT ( 'NONE',  ( 15.39999999999989022, 2.500000000000000000, -2.385244779468109755E-15 ) ) ;
#20238 = CARTESIAN_POINT ( 'NONE',  ( 4.149999999999941735, 2.500000000000000000, -5.902370205355750521 ) ) ;
#20239 = DIRECTION ( 'NONE',  ( 0.000000000000000000, 0.000000000000000000, 1.000000000000000000 ) ) ;
#20240 = ORIENTED_EDGE ( 'NONE', *, *, #46855, .T. ) ;
#20241 = EDGE_CURVE ( 'NONE', #7975, #118333, #48850, .T. ) ;
#20242 = EDGE_LOOP ( 'NONE', ( #20494, #91539, #65000, #126350 ) ) ;
#20243 = ORIENTED_EDGE ( 'NONE', *, *, #36845, .F. ) ;
#20244 = ORIENTED_EDGE ( 'NONE', *, *, #58988, .F. ) ;
#20245 = DIRECTION ( 'NONE',  ( 0.000000000000000000, 0.000000000000000000, 1.000000000000000000 ) ) ;
#20246 = AXIS2_PLACEMENT_3D ( 'NONE', #24676, #25292, #24037 ) ;
#20247 = DIRECTION ( 'NONE',  ( 0.000000000000000000, 0.000000000000000000, -1.000000000000000000 ) ) ;
#20248 = FACE_OUTER_BOUND ( 'NONE', #25470, .T. ) ;
#20249 = CARTESIAN_POINT ( 'NONE',  ( 3.549999999999942979, 2.500000000000000000, 1.818653347947321475 ) ) ;
#20250 = ORIENTED_EDGE ( 'NONE', *, *, #35826, .F. ) ;
#20251 = DIRECTION ( 'NONE',  ( 0.000000000000000000, 0.000000000000000000, 1.000000000000000000 ) ) ;
#20252 = DIRECTION ( 'NONE',  ( 0.000000000000000000, 1.000000000000000000, 0.000000000000000000 ) ) ;
#20253 = DIRECTION ( 'NONE',  ( -0.000000000000000000, -1.000000000000000000, -0.000000000000000000 ) ) ;
#20254 = FACE_OUTER_BOUND ( 'NONE', #28019, .T. ) ;
#20255 = ORIENTED_EDGE ( 'NONE', *, *, #57417, .F. ) ;
#20256 = CIRCLE ( 'NONE', #110143, 0.06509327318403745899 ) ;
#20257 = LINE ( 'NONE', #113632, #62540 ) ;
#20258 = AXIS2_PLACEMENT_3D ( 'NONE', #27792, #919, #57921 ) ;
#20259 = EDGE_LOOP ( 'NONE', ( #48934, #105451, #18596, #40704 ) ) ;
#20260 = VERTEX_POINT ( 'NONE', #112405 ) ;
#20261 = DIRECTION ( 'NONE',  ( 0.000000000000000000, 0.000000000000000000, 1.000000000000000000 ) ) ;
#20262 = DIRECTION ( 'NONE',  ( -0.000000000000000000, 1.000000000000000000, -0.000000000000000000 ) ) ;
#20263 = FACE_BOUND ( 'NONE', #50859, .T. ) ;
#20264 = DIRECTION ( 'NONE',  ( 0.000000000000000000, 1.000000000000000000, 0.000000000000000000 ) ) ;
#20265 = CARTESIAN_POINT ( 'NONE',  ( 9.999999999999911182, 2.500000000000000000, -3.637306695894650055 ) ) ;
#20266 = AXIS2_PLACEMENT_3D ( 'NONE', #13509, #43017, #103191 ) ;
#20267 = CARTESIAN_POINT ( 'NONE',  ( 9.399999999999915090, 2.500000000000000000, 4.576537180435972019 ) ) ;
#20268 = FACE_OUTER_BOUND ( 'NONE', #61761, .T. ) ;
#20269 = CARTESIAN_POINT ( 'NONE',  ( 7.699999999999925571, 12.50000000000000000, -4.676537180435978769 ) ) ;
#20270 = CARTESIAN_POINT ( 'NONE',  ( -9.400000000000009237, 2.500000000000000000, -3.983716857408421852 ) ) ;
#20271 = DIRECTION ( 'NONE',  ( 0.000000000000000000, 1.000000000000000000, 0.000000000000000000 ) ) ;
#20272 = VERTEX_POINT ( 'NONE', #33831 ) ;
#20274 = CONICAL_SURFACE ( 'NONE', #68292, 0.09999999999999982514, 0.003490658503988666988 ) ;
#20273 = AXIS2_PLACEMENT_3D ( 'NONE', #75275, #89451, #18122 ) ;
#20275 = CARTESIAN_POINT ( 'NONE',  ( 2.499999999999947153, 2.500000000000000000, 3.637306695894644726 ) ) ;
#20277 = EDGE_CURVE ( 'NONE', #90767, #91316, #101362, .T. ) ;
#20276 = CONICAL_SURFACE ( 'NONE', #97641, 0.1000000000000000472, 0.003490658503988666988 ) ;
#20278 = DIRECTION ( 'NONE',  ( -0.000000000000000000, 1.000000000000000000, -0.000000000000000000 ) ) ;
#20279 = VERTEX_POINT ( 'NONE', #24024 ) ;
#20280 = ORIENTED_EDGE ( 'NONE', *, *, #40138, .F. ) ;
#20281 = CARTESIAN_POINT ( 'NONE',  ( 12.94999999999989981, 2.500000000000000000, -2.265063509461101798 ) ) ;
#20282 = EDGE_CURVE ( 'NONE', #102223, #128465, #23990, .T. ) ;
#20283 = DIRECTION ( 'NONE',  ( 0.000000000000000000, 1.000000000000000000, 0.000000000000000000 ) ) ;
#20284 = FACE_BOUND ( 'NONE', #56062, .T. ) ;
#20285 = EDGE_CURVE ( 'NONE', #111104, #63288, #34504, .T. ) ;
#20286 = DIRECTION ( 'NONE',  ( 0.000000000000000000, 1.000000000000000000, 0.000000000000000000 ) ) ;
#20287 = DIRECTION ( 'NONE',  ( 0.000000000000000000, 0.000000000000000000, 1.000000000000000000 ) ) ;
#20288 = EDGE_CURVE ( 'NONE', #66014, #115619, #75053, .T. ) ;
#20289 = EDGE_CURVE ( 'NONE', #31251, #63386, #55100, .T. ) ;
#20290 = VERTEX_POINT ( 'NONE', #104502 ) ;
#20291 = DIRECTION ( 'NONE',  ( -0.000000000000000000, -1.000000000000000000, -0.000000000000000000 ) ) ;
#20292 = ADVANCED_FACE ( 'NONE', ( #86131 ), #71827, .T. ) ;
#20293 = ADVANCED_FACE ( 'NONE', ( #36436 ), #106439, .T. ) ;
#20294 = CARTESIAN_POINT ( 'NONE',  ( 184.7500000000000000, 9.429780353434619030E-16, -7.700000000000000178 ) ) ;
#20295 = CIRCLE ( 'NONE', #53649, 0.09999999999999982514 ) ;
#20296 = ADVANCED_FACE ( 'NONE', ( #115599 ), #92757, .T. ) ;
#20297 = AXIS2_PLACEMENT_3D ( 'NONE', #61547, #22908, #83120 ) ;
#20298 = EDGE_LOOP ( 'NONE', ( #119954, #12001, #108596, #49931 ) ) ;
#20299 = DIRECTION ( 'NONE',  ( 0.000000000000000000, 0.000000000000000000, -1.000000000000000000 ) ) ;
#20300 = AXIS2_PLACEMENT_3D ( 'NONE', #81969, #102892, #91799 ) ;
#20301 = DIRECTION ( 'NONE',  ( 0.000000000000000000, 0.000000000000000000, 1.000000000000000000 ) ) ;
#20302 = CARTESIAN_POINT ( 'NONE',  ( -4.150000000000024336, 2.500000000000000000, -2.757883832488654097 ) ) ;
#20304 = EDGE_CURVE ( 'NONE', #43675, #112383, #30072, .T. ) ;
#20303 = DIRECTION ( 'NONE',  ( 0.000000000000000000, -0.000000000000000000, 1.000000000000000000 ) ) ;
#20305 = CIRCLE ( 'NONE', #110196, 0.06509327318403745899 ) ;
#20306 = CONICAL_SURFACE ( 'NONE', #9836, 0.1000000000000002554, 0.003490658503988666988 ) ;
#20307 = ADVANCED_FACE ( 'NONE', ( #124800 ), #82294, .T. ) ;
#20308 = VERTEX_POINT ( 'NONE', #56673 ) ;
#20309 = AXIS2_PLACEMENT_3D ( 'NONE', #117947, #28296, #87198 ) ;
#20310 = DIRECTION ( 'NONE',  ( 0.000000000000000000, 0.000000000000000000, -1.000000000000000000 ) ) ;
#20311 = DIRECTION ( 'NONE',  ( 0.000000000000000000, 1.000000000000000000, 0.000000000000000000 ) ) ;
#20312 = DIRECTION ( 'NONE',  ( 0.000000000000000000, 0.000000000000000000, 1.000000000000000000 ) ) ;
#20313 = CARTESIAN_POINT ( 'NONE',  ( 8.749999999999957367, 2.500000000000000000, -6.395190528383301931 ) ) ;
#20314 = ORIENTED_EDGE ( 'NONE', *, *, #129182, .T. ) ;
#20315 = ORIENTED_EDGE ( 'NONE', *, *, #61461, .T. ) ;
#20316 = CIRCLE ( 'NONE', #93480, 0.06509327318403745899 ) ;
#20317 = CARTESIAN_POINT ( 'NONE',  ( 5.399999999999934630, 2.500000000000000000, -0.6928203230275542523 ) ) ;
#20318 = CIRCLE ( 'NONE', #122531, 0.06509327318403745899 ) ;
#20319 = ORIENTED_EDGE ( 'NONE', *, *, #60685, .F. ) ;
#20320 = DIRECTION ( 'NONE',  ( 0.000000000000000000, 1.000000000000000000, 0.000000000000000000 ) ) ;
#20321 = DIRECTION ( 'NONE',  ( -0.000000000000000000, -1.000000000000000000, -0.000000000000000000 ) ) ;
#20323 = AXIS2_PLACEMENT_3D ( 'NONE', #102566, #122232, #22753 ) ;
#20322 = CIRCLE ( 'NONE', #35014, 0.09999999999999982514 ) ;
#20324 = DIRECTION ( 'NONE',  ( -0.000000000000000000, -1.000000000000000000, -0.000000000000000000 ) ) ;
#20325 = ORIENTED_EDGE ( 'NONE', *, *, #112312, .F. ) ;
#20326 = LINE ( 'NONE', #97588, #55804 ) ;
#20327 = DIRECTION ( 'NONE',  ( -0.000000000000000000, 1.000000000000000000, -0.000000000000000000 ) ) ;
#20328 = CARTESIAN_POINT ( 'NONE',  ( -10.00000000000000533, 2.500000000000000000, -5.122947341949750211 ) ) ;
#20329 = DIRECTION ( 'NONE',  ( -4.274815082592931898E-19, -0.9999939076577903929, -0.003490651415223739937 ) ) ;
#20330 = CARTESIAN_POINT ( 'NONE',  ( 11.24999999999991118, 2.500000000000000000, -2.757883832488654097 ) ) ;
#20331 = DIRECTION ( 'NONE',  ( 0.000000000000000000, 1.000000000000000000, 0.000000000000000000 ) ) ;
#20332 = ORIENTED_EDGE ( 'NONE', *, *, #91826, .F. ) ;
#20333 = VERTEX_POINT ( 'NONE', #126733 ) ;
#20334 = DIRECTION ( 'NONE',  ( 0.000000000000000000, 1.000000000000000000, 0.000000000000000000 ) ) ;
#20335 = EDGE_LOOP ( 'NONE', ( #116614, #108653 ) ) ;
#20336 = FACE_OUTER_BOUND ( 'NONE', #54629, .T. ) ;
#20338 = ORIENTED_EDGE ( 'NONE', *, *, #37525, .T. ) ;
#20337 = ORIENTED_EDGE ( 'NONE', *, *, #52347, .T. ) ;
#20339 = VERTEX_POINT ( 'NONE', #87435 ) ;
#20340 = EDGE_CURVE ( 'NONE', #115126, #71852, #109470, .T. ) ;
#20341 = AXIS2_PLACEMENT_3D ( 'NONE', #8647, #47315, #48603 ) ;
#20342 = CARTESIAN_POINT ( 'NONE',  ( 87.50000000000001421, -3.413194297214860118, -6.711110875543777610 ) ) ;
#20343 = ADVANCED_FACE ( 'NONE', ( #95979 ), #6920, .T. ) ;
#20344 = DIRECTION ( 'NONE',  ( -0.000000000000000000, 1.000000000000000000, -0.000000000000000000 ) ) ;
#20345 = DIRECTION ( 'NONE',  ( -0.000000000000000000, -1.000000000000000000, -0.000000000000000000 ) ) ;
#20346 = EDGE_CURVE ( 'NONE', #32403, #27815, #103211, .T. ) ;
#20347 = DIRECTION ( 'NONE',  ( 0.000000000000000000, 0.000000000000000000, 1.000000000000000000 ) ) ;
#20348 = CARTESIAN_POINT ( 'NONE',  ( -5.850000000000018296, 12.50000000000000000, 1.472243186433545459 ) ) ;
#20349 = CARTESIAN_POINT ( 'NONE',  ( -15.19999999999998330, 2.500000000000000000, 0.3464101615137758494 ) ) ;
#20350 = LINE ( 'NONE', #100201, #47091 ) ;
#20351 = CARTESIAN_POINT ( 'NONE',  ( -5.650000000000023448, 2.500000000000000000, -2.511473670974877948 ) ) ;
#20352 = EDGE_CURVE ( 'NONE', #86066, #75789, #86796, .T. ) ;
#20353 = CARTESIAN_POINT ( 'NONE',  ( 13.54999999999989946, 12.50000000000000000, 2.511473670974873507 ) ) ;
#20354 = EDGE_CURVE ( 'NONE', #47249, #9122, #97264, .T. ) ;
#20355 = ORIENTED_EDGE ( 'NONE', *, *, #117958, .F. ) ;
#20356 = VECTOR ( 'NONE', #15886, 1000.000000000000000 ) ;
#20357 = EDGE_CURVE ( 'NONE', #28403, #42353, #17517, .T. ) ;
#20358 = LINE ( 'NONE', #2625, #113408 ) ;
#20359 = ORIENTED_EDGE ( 'NONE', *, *, #42994, .T. ) ;
#20360 = ORIENTED_EDGE ( 'NONE', *, *, #67693, .F. ) ;
#20361 = CARTESIAN_POINT ( 'NONE',  ( 4.149999999999938183, 12.50000000000000000, 7.188010851410848723 ) ) ;
#20362 = CARTESIAN_POINT ( 'NONE',  ( -1.450000000000036371, 12.50000000000000000, 6.841600689897072485 ) ) ;
#20363 = EDGE_CURVE ( 'NONE', #4736, #5250, #94681, .T. ) ;
#20365 = CIRCLE ( 'NONE', #122770, 0.06509327318403745899 ) ;
#20364 = AXIS2_PLACEMENT_3D ( 'NONE', #108466, #90103, #48926 ) ;
#20366 = CYLINDRICAL_SURFACE ( 'NONE', #98432, 2.000000000000000000 ) ;
#20367 = AXIS2_PLACEMENT_3D ( 'NONE', #100990, #51273, #42753 ) ;
#20368 = DIRECTION ( 'NONE',  ( 0.000000000000000000, 1.000000000000000000, 0.000000000000000000 ) ) ;
#20369 = CARTESIAN_POINT ( 'NONE',  ( -10.60000000000000142, 12.50000000000000000, 0.4115034346978110880 ) ) ;
#20370 = FACE_OUTER_BOUND ( 'NONE', #110545, .T. ) ;
#20371 = ORIENTED_EDGE ( 'NONE', *, *, #89059, .T. ) ;
#20373 = CONICAL_SURFACE ( 'NONE', #116500, 0.1000000000000002554, 0.003490658503988666988 ) ;
#20372 = AXIS2_PLACEMENT_3D ( 'NONE', #67049, #48091, #96514 ) ;
#20374 = ORIENTED_EDGE ( 'NONE', *, *, #127743, .T. ) ;
#20375 = DIRECTION ( 'NONE',  ( -0.000000000000000000, 1.000000000000000000, -0.000000000000000000 ) ) ;
#20376 = AXIS2_PLACEMENT_3D ( 'NONE', #15782, #123798, #73417 ) ;
#20377 = EDGE_LOOP ( 'NONE', ( #104530, #14664, #654, #79397 ) ) ;
#20378 = CARTESIAN_POINT ( 'NONE',  ( 186.4166666666666856, 6.668395609140176816, 3.850000000000000977 ) ) ;
#20379 = EDGE_LOOP ( 'NONE', ( #30717, #10619, #122244, #60600 ) ) ;
#20380 = ADVANCED_FACE ( 'NONE', ( #7585 ), #90691, .T. ) ;
#20381 = ORIENTED_EDGE ( 'NONE', *, *, #123733, .T. ) ;
#20382 = CARTESIAN_POINT ( 'NONE',  ( 4.399999999999939071, 12.50000000000000000, 0.3464101615137736845 ) ) ;
#20383 = DIRECTION ( 'NONE',  ( 0.000000000000000000, -0.9999939076577903929, 0.003490651415223739937 ) ) ;
#20384 = VECTOR ( 'NONE', #30474, 1000.000000000000000 ) ;
#20385 = CARTESIAN_POINT ( 'NONE',  ( -13.09999999999999076, 2.500000000000000000, 4.576537180435972019 ) ) ;
#20386 = CARTESIAN_POINT ( 'NONE',  ( -2.050000000000032685, 2.500000000000000000, -6.395190528383301931 ) ) ;
#20387 = AXIS2_PLACEMENT_3D ( 'NONE', #41601, #2950, #12108 ) ;
#20388 = CARTESIAN_POINT ( 'NONE',  ( 87.50000000000001421, 1.433398978532515633, 7.395196794792773254 ) ) ;
#20389 = ORIENTED_EDGE ( 'NONE', *, *, #36423, .F. ) ;
#20390 = CARTESIAN_POINT ( 'NONE',  ( -1.050000000000038680, 2.500000000000000000, 2.411473670974873862 ) ) ;
#20391 = CARTESIAN_POINT ( 'NONE',  ( 11.24999999999990941, 2.500000000000000000, -1.472243186433550122 ) ) ;
#20392 = DIRECTION ( 'NONE',  ( 0.000000000000000000, -0.000000000000000000, 1.000000000000000000 ) ) ;
#20393 = CARTESIAN_POINT ( 'NONE',  ( 6.899999999999928413, 12.50000000000000000, -3.983716857408426293 ) ) ;
#20394 = AXIS2_PLACEMENT_3D ( 'NONE', #64435, #71853, #60739 ) ;
#20395 = VECTOR ( 'NONE', #121734, 1000.000000000000000 ) ;
#20396 = CARTESIAN_POINT ( 'NONE',  ( -10.65000000000000391, 12.50000000000000000, -6.841600689897075149 ) ) ;
#20397 = VERTEX_POINT ( 'NONE', #46229 ) ;
#20398 = AXIS2_PLACEMENT_3D ( 'NONE', #4271, #35068, #94598 ) ;
#20399 = ADVANCED_FACE ( 'NONE', ( #85512 ), #57246, .T. ) ;
#20400 = EDGE_LOOP ( 'NONE', ( #86900, #35127 ) ) ;
#20401 = DIRECTION ( 'NONE',  ( 0.000000000000000000, -0.9999939076577903929, 0.003490651415223739937 ) ) ;
#20402 = AXIS2_PLACEMENT_3D ( 'NONE', #44135, #72959, #83430 ) ;
#20403 = ORIENTED_EDGE ( 'NONE', *, *, #1919, .T. ) ;
#20404 = CARTESIAN_POINT ( 'NONE',  ( 3.299999999999942979, 2.500000000000000000, 4.330127018922196314 ) ) ;
#20405 = CARTESIAN_POINT ( 'NONE',  ( -14.14999999999998614, 12.50000000000000000, -2.857883832488651521 ) ) ;
#20406 = VECTOR ( 'NONE', #5862, 1000.000000000000000 ) ;
#20407 = VECTOR ( 'NONE', #42650, 1000.000000000000000 ) ;
#20408 = ORIENTED_EDGE ( 'NONE', *, *, #65946, .F. ) ;
#20409 = DIRECTION ( 'NONE',  ( 0.000000000000000000, 0.000000000000000000, 1.000000000000000000 ) ) ;
#20411 = VECTOR ( 'NONE', #83619, 1000.000000000000000 ) ;
#20410 = DIRECTION ( 'NONE',  ( -0.000000000000000000, 1.000000000000000000, -0.000000000000000000 ) ) ;
#20412 = ADVANCED_FACE ( 'NONE', ( #6282 ), #126197, .T. ) ;
#20413 = CARTESIAN_POINT ( 'NONE',  ( -0.8500000000000390576, 2.500000000000000000, -6.595190528383302109 ) ) ;
#20414 = LINE ( 'NONE', #19088, #56025 ) ;
#20416 = CONICAL_SURFACE ( 'NONE', #37150, 0.09999999999999982514, 0.003490658503988666988 ) ;
#20415 = CIRCLE ( 'NONE', #122919, 0.09999999999999982514 ) ;
#20417 = PLANE ( 'NONE',  #54030 ) ;
#20418 = ORIENTED_EDGE ( 'NONE', *, *, #161, .T. ) ;
#20419 = CARTESIAN_POINT ( 'NONE',  ( 26.76313892655710447, 1.072173145595670452, -4.440523166430129010 ) ) ;
#20420 = CARTESIAN_POINT ( 'NONE',  ( 6.899999999999928413, 2.500000000000000000, 3.983716857408420964 ) ) ;
#20421 = PLANE ( 'NONE',  #67873 ) ;
#20422 = DIRECTION ( 'NONE',  ( -0.000000000000000000, 1.000000000000000000, -0.000000000000000000 ) ) ;
#20423 = ORIENTED_EDGE ( 'NONE', *, *, #53522, .F. ) ;
#20424 = VERTEX_POINT ( 'NONE', #107733 ) ;
#20425 = DIRECTION ( 'NONE',  ( -0.000000000000000000, -1.000000000000000000, -0.000000000000000000 ) ) ;
#20426 = CARTESIAN_POINT ( 'NONE',  ( -5.800000000000018474, 12.50000000000000000, 4.330127018922196314 ) ) ;
#20427 = AXIS2_PLACEMENT_3D ( 'NONE', #47685, #69232, #97413 ) ;
#20428 = DIRECTION ( 'NONE',  ( 0.000000000000000000, 1.000000000000000000, 0.000000000000000000 ) ) ;
#20429 = EDGE_LOOP ( 'NONE', ( #117416, #18691 ) ) ;
#20430 = DIRECTION ( 'NONE',  ( 0.000000000000000000, -0.9999939076577903929, 0.003490651415223739937 ) ) ;
#20431 = EDGE_CURVE ( 'NONE', #71600, #112569, #76022, .T. ) ;
#20432 = CARTESIAN_POINT ( 'NONE',  ( -12.69999999999999218, 12.50000000000000000, 4.611443907251934426 ) ) ;
#20433 = EDGE_LOOP ( 'NONE', ( #119095, #127340 ) ) ;
#20434 = DIRECTION ( 'NONE',  ( 0.000000000000000000, 0.000000000000000000, -1.000000000000000000 ) ) ;
#20435 = ORIENTED_EDGE ( 'NONE', *, *, #115865, .T. ) ;
#20436 = DIRECTION ( 'NONE',  ( 0.000000000000000000, 0.000000000000000000, 1.000000000000000000 ) ) ;
#20437 = EDGE_CURVE ( 'NONE', #33882, #111424, #19592, .T. ) ;
#20438 = CONICAL_SURFACE ( 'NONE', #110233, 0.1000000000000002554, 0.003490658503988666988 ) ;
#20439 = CIRCLE ( 'NONE', #22614, 0.06509327318403745899 ) ;
#20440 = ORIENTED_EDGE ( 'NONE', *, *, #43289, .T. ) ;
#20441 = CARTESIAN_POINT ( 'NONE',  ( 9.549999999999918998, 2.500000000000000000, -6.495190528383302464 ) ) ;
#20442 = CARTESIAN_POINT ( 'NONE',  ( 15.83209681635555022, 2.500000000000000000, -5.404881881984143099 ) ) ;
#20443 = EDGE_CURVE ( 'NONE', #52720, #39660, #99004, .T. ) ;
#20444 = VERTEX_POINT ( 'NONE', #59952 ) ;
#20445 = EDGE_CURVE ( 'NONE', #60383, #16549, #61468, .T. ) ;
#20446 = ORIENTED_EDGE ( 'NONE', *, *, #68139, .F. ) ;
#20447 = EDGE_CURVE ( 'NONE', #46996, #17873, #76945, .T. ) ;
#20448 = EDGE_CURVE ( 'NONE', #1478, #37337, #34278, .T. ) ;
#20449 = CARTESIAN_POINT ( 'NONE',  ( 10.79999999999991012, 2.500000000000000000, -4.330127018922201643 ) ) ;
#20450 = DIRECTION ( 'NONE',  ( 0.000000000000000000, 0.000000000000000000, 1.000000000000000000 ) ) ;
#20451 = ORIENTED_EDGE ( 'NONE', *, *, #67621, .T. ) ;
#20452 = VECTOR ( 'NONE', #41945, 1000.000000000000000 ) ;
#20453 = DIRECTION ( 'NONE',  ( 0.000000000000000000, 1.000000000000000000, 0.000000000000000000 ) ) ;
#20454 = CARTESIAN_POINT ( 'NONE',  ( -11.84999999999999787, 2.500000000000000000, -1.918653347947322008 ) ) ;
#20455 = CIRCLE ( 'NONE', #37193, 0.06509327318403745899 ) ;
#20456 = EDGE_CURVE ( 'NONE', #5343, #57940, #109673, .T. ) ;
#20457 = DIRECTION ( 'NONE',  ( -0.000000000000000000, -1.000000000000000000, -0.000000000000000000 ) ) ;
#20458 = ADVANCED_FACE ( 'NONE', ( #48827 ), #40545, .T. ) ;
#20459 = CARTESIAN_POINT ( 'NONE',  ( 104.6937551430669089, 7.847315309856959686, 3.764367982486338526 ) ) ;
#20460 = DIRECTION ( 'NONE',  ( 0.000000000000000000, 1.000000000000000000, 0.000000000000000000 ) ) ;
#20461 = CARTESIAN_POINT ( 'NONE',  ( 12.04999999999990834, 2.500000000000000000, 6.495190528383297135 ) ) ;
#20462 = CARTESIAN_POINT ( 'NONE',  ( 10.44999999999991047, 12.50000000000000000, -6.495190528383302464 ) ) ;
#20463 = ADVANCED_FACE ( 'NONE', ( #48170 ), #124134, .T. ) ;
#20464 = EDGE_CURVE ( 'NONE', #112146, #58918, #113682, .T. ) ;
#20465 = AXIS2_PLACEMENT_3D ( 'NONE', #40623, #110614, #60873 ) ;
#20466 = ADVANCED_FACE ( 'NONE', ( #50122 ), #90008, .T. ) ;
#20467 = EDGE_LOOP ( 'NONE', ( #125083, #56515 ) ) ;
#20468 = ORIENTED_EDGE ( 'NONE', *, *, #77017, .F. ) ;
#20469 = ORIENTED_EDGE ( 'NONE', *, *, #79962, .T. ) ;
#20470 = DIRECTION ( 'NONE',  ( -0.000000000000000000, -1.000000000000000000, -0.000000000000000000 ) ) ;
#20471 = DIRECTION ( 'NONE',  ( 0.000000000000000000, 1.000000000000000000, 0.000000000000000000 ) ) ;
#20472 = VECTOR ( 'NONE', #10690, 1000.000000000000000 ) ;
#20473 = CARTESIAN_POINT ( 'NONE',  ( 4.549999999999935874, 2.500000000000000000, 6.495190528383297135 ) ) ;
#20475 = EDGE_LOOP ( 'NONE', ( #63156, #66902, #60846, #66480 ) ) ;
#20474 = VERTEX_POINT ( 'NONE', #40292 ) ;
#20476 = FACE_BOUND ( 'NONE', #77775, .T. ) ;
#20477 = ORIENTED_EDGE ( 'NONE', *, *, #34492, .T. ) ;
#20478 = EDGE_CURVE ( 'NONE', #49092, #81291, #9124, .T. ) ;
#20479 = CARTESIAN_POINT ( 'NONE',  ( 12.89999999999990266, 2.500000000000000000, 5.122947341949749323 ) ) ;
#20480 = DIRECTION ( 'NONE',  ( 0.000000000000000000, 0.000000000000000000, 1.000000000000000000 ) ) ;
#20481 = DIRECTION ( 'NONE',  ( 0.000000000000000000, 0.000000000000000000, -1.000000000000000000 ) ) ;
#20482 = AXIS2_PLACEMENT_3D ( 'NONE', #47008, #65330, #86911 ) ;
#20483 = DIRECTION ( 'NONE',  ( -4.274815082592931898E-19, -0.9999939076577903929, -0.003490651415223739937 ) ) ;
#20484 = DIRECTION ( 'NONE',  ( 0.000000000000000000, 0.000000000000000000, 1.000000000000000000 ) ) ;
#20485 = DIRECTION ( 'NONE',  ( -0.000000000000000000, 1.000000000000000000, -0.000000000000000000 ) ) ;
#20486 = AXIS2_PLACEMENT_3D ( 'NONE', #49982, #107590, #38884 ) ;
#20487 = DIRECTION ( 'NONE',  ( 0.000000000000000000, -0.000000000000000000, 1.000000000000000000 ) ) ;
#20488 = CARTESIAN_POINT ( 'NONE',  ( 15.59999999999988951, 12.50000000000000000, -0.2813168883297409439 ) ) ;
#20489 = DIRECTION ( 'NONE',  ( 0.000000000000000000, 1.000000000000000000, 0.000000000000000000 ) ) ;
#20490 = AXIS2_PLACEMENT_3D ( 'NONE', #21634, #122419, #12438 ) ;
#20491 = DIRECTION ( 'NONE',  ( -0.000000000000000000, 1.000000000000000000, -0.000000000000000000 ) ) ;
#20492 = EDGE_LOOP ( 'NONE', ( #58523, #75477 ) ) ;
#20494 = ORIENTED_EDGE ( 'NONE', *, *, #29650, .F. ) ;
#20493 = CIRCLE ( 'NONE', #64391, 0.1000000000000002554 ) ;
#20495 = EDGE_LOOP ( 'NONE', ( #64592, #43412, #30172, #2556 ) ) ;
#20496 = ORIENTED_EDGE ( 'NONE', *, *, #128983, .F. ) ;
#20497 = DIRECTION ( 'NONE',  ( -0.000000000000000000, 1.000000000000000000, -0.000000000000000000 ) ) ;
#20498 = PLANE ( 'NONE',  #111277 ) ;
#20500 = ORIENTED_EDGE ( 'NONE', *, *, #121700, .F. ) ;
#20499 = VERTEX_POINT ( 'NONE', #78292 ) ;
#20502 = VERTEX_POINT ( 'NONE', #78935 ) ;
#20501 = AXIS2_PLACEMENT_3D ( 'NONE', #23701, #64260, #41428 ) ;
#20504 = AXIS2_PLACEMENT_3D ( 'NONE', #25135, #54584, #105645 ) ;
#20503 = CARTESIAN_POINT ( 'NONE',  ( -14.59999999999998366, 2.500000000000000000, -0.6928203230275520319 ) ) ;
#20505 = CIRCLE ( 'NONE', #10034, 0.06509327318403741736 ) ;
#20506 = DIRECTION ( 'NONE',  ( 0.000000000000000000, 1.000000000000000000, 0.000000000000000000 ) ) ;
#20507 = DIRECTION ( 'NONE',  ( 0.000000000000000000, 0.000000000000000000, 1.000000000000000000 ) ) ;
#20508 = CARTESIAN_POINT ( 'NONE',  ( -8.950000000000004619, 2.500000000000000000, 6.248780366869521430 ) ) ;
#20509 = FACE_OUTER_BOUND ( 'NONE', #54767, .T. ) ;
#20510 = DIRECTION ( 'NONE',  ( -4.274815082592931898E-19, -0.9999939076577903929, -0.003490651415223739937 ) ) ;
#20511 = CARTESIAN_POINT ( 'NONE',  ( 9.149999999999920419, 12.50000000000000000, -5.802370205355749988 ) ) ;
#20512 = AXIS2_PLACEMENT_3D ( 'NONE', #104533, #53513, #86157 ) ;
#20513 = ORIENTED_EDGE ( 'NONE', *, *, #8051, .T. ) ;
#20514 = FACE_OUTER_BOUND ( 'NONE', #111969, .T. ) ;
#20515 = EDGE_LOOP ( 'NONE', ( #48007, #33381 ) ) ;
#20516 = EDGE_CURVE ( 'NONE', #111617, #7920, #84432, .T. ) ;
#20517 = CIRCLE ( 'NONE', #116638, 0.1000000000000000056 ) ;
#20518 = ORIENTED_EDGE ( 'NONE', *, *, #124061, .F. ) ;
#20519 = EDGE_LOOP ( 'NONE', ( #5342, #49334, #94913, #3877 ) ) ;
#20520 = ADVANCED_FACE ( 'NONE', ( #88737 ), #29721, .T. ) ;
#20521 = CARTESIAN_POINT ( 'NONE',  ( 187.5000000000000000, 9.429780353434619030E-16, -7.700000000000000178 ) ) ;
#20522 = ORIENTED_EDGE ( 'NONE', *, *, #88298, .F. ) ;
#20523 = ORIENTED_EDGE ( 'NONE', *, *, #33352, .F. ) ;
#20524 = DIRECTION ( 'NONE',  ( 0.000000000000000000, 1.000000000000000000, 0.000000000000000000 ) ) ;
#20525 = ADVANCED_FACE ( 'NONE', ( #36846, #87211 ), #17152, .T. ) ;
#20526 = DIRECTION ( 'NONE',  ( -0.000000000000000000, 1.000000000000000000, -0.000000000000000000 ) ) ;
#20527 = CARTESIAN_POINT ( 'NONE',  ( -2.900000000000029221, 2.500000000000000000, -0.5928203230275541635 ) ) ;
#20528 = DIRECTION ( 'NONE',  ( -4.274815082592931898E-19, -0.9999939076577903929, -0.003490651415223739937 ) ) ;
#20529 = LINE ( 'NONE', #70269, #103436 ) ;
#20530 = CARTESIAN_POINT ( 'NONE',  ( -3.950000000000026379, 2.500000000000000000, 2.511473670974873507 ) ) ;
#20531 = DIRECTION ( 'NONE',  ( -4.274815082592931898E-19, -0.9999939076577903929, -0.003490651415223739937 ) ) ;
#20532 = ORIENTED_EDGE ( 'NONE', *, *, #77601, .F. ) ;
#20533 = DIRECTION ( 'NONE',  ( -0.000000000000000000, 1.000000000000000000, -0.000000000000000000 ) ) ;
#20534 = ORIENTED_EDGE ( 'NONE', *, *, #102598, .T. ) ;
#20535 = CARTESIAN_POINT ( 'NONE',  ( 112.4783714810219806, 8.410376606499987417, -2.247359121523905490 ) ) ;
#20536 = DIRECTION ( 'NONE',  ( -4.274815082592931898E-19, -0.9999939076577903929, -0.003490651415223739937 ) ) ;
#20537 = AXIS2_PLACEMENT_3D ( 'NONE', #123654, #32741, #92941 ) ;
#20538 = AXIS2_PLACEMENT_3D ( 'NONE', #8415, #47720, #100039 ) ;
#20539 = EDGE_LOOP ( 'NONE', ( #22348, #121340 ) ) ;
#20541 = AXIS2_PLACEMENT_3D ( 'NONE', #101294, #81005, #120923 ) ;
#20540 = DIRECTION ( 'NONE',  ( 0.000000000000000000, -0.9999939076577903929, 0.003490651415223739937 ) ) ;
#20542 = CARTESIAN_POINT ( 'NONE',  ( 6.449999999999933564, 2.500000000000000000, -6.841600689897078702 ) ) ;
#20543 = EDGE_LOOP ( 'NONE', ( #113646, #64467, #9979, #123617 ) ) ;
#20544 = CARTESIAN_POINT ( 'NONE',  ( 6.649999999999931966, 2.500000000000000000, -5.802370205355749988 ) ) ;
#20545 = ORIENTED_EDGE ( 'NONE', *, *, #75242, .F. ) ;
#20546 = ORIENTED_EDGE ( 'NONE', *, *, #124426, .F. ) ;
#20547 = CARTESIAN_POINT ( 'NONE',  ( 9.799999999999915445, 2.500000000000000000, 3.983716857408420964 ) ) ;
#20548 = DIRECTION ( 'NONE',  ( 1.000000000000000000, 0.000000000000000000, 0.000000000000000000 ) ) ;
#20549 = LINE ( 'NONE', #38928, #77301 ) ;
#20550 = DIRECTION ( 'NONE',  ( 0.000000000000000000, 1.000000000000000000, 0.000000000000000000 ) ) ;
#20551 = AXIS2_PLACEMENT_3D ( 'NONE', #58111, #79046, #69187 ) ;
#20552 = DIRECTION ( 'NONE',  ( 0.000000000000000000, 1.000000000000000000, 0.000000000000000000 ) ) ;
#20553 = VECTOR ( 'NONE', #121038, 1000.000000000000000 ) ;
#20554 = VERTEX_POINT ( 'NONE', #67562 ) ;
#20555 = FACE_OUTER_BOUND ( 'NONE', #114658, .T. ) ;
#20556 = ORIENTED_EDGE ( 'NONE', *, *, #100842, .F. ) ;
#20557 = CARTESIAN_POINT ( 'NONE',  ( 12.89999999999990088, 12.50000000000000000, 4.330127018922196314 ) ) ;
#20559 = AXIS2_PLACEMENT_3D ( 'NONE', #95491, #5800, #75838 ) ;
#20558 = CARTESIAN_POINT ( 'NONE',  ( 9.349999999999916156, 2.500000000000000000, 6.048780366869520364 ) ) ;
#20560 = EDGE_CURVE ( 'NONE', #65002, #65711, #47951, .T. ) ;
#20561 = EDGE_CURVE ( 'NONE', #113501, #104378, #44386, .T. ) ;
#20562 = AXIS2_PLACEMENT_3D ( 'NONE', #25685, #55799, #83342 ) ;
#20563 = CARTESIAN_POINT ( 'NONE',  ( 186.2968750003414584, 8.734944146203032389, 5.348610694689227483E-16 ) ) ;
#20564 = CARTESIAN_POINT ( 'NONE',  ( 0.8499999999999553468, 2.500000000000000000, 1.472243186433545459 ) ) ;
#20565 = DIRECTION ( 'NONE',  ( 0.000000000000000000, 0.000000000000000000, 1.000000000000000000 ) ) ;
#20566 = EDGE_CURVE ( 'NONE', #85870, #101480, #61115, .T. ) ;
#20567 = DIRECTION ( 'NONE',  ( -0.000000000000000000, -1.000000000000000000, -0.000000000000000000 ) ) ;
#20568 = CARTESIAN_POINT ( 'NONE',  ( -1.900000000000034106, 12.50000000000000000, -3.983716857408426293 ) ) ;
#20569 = VERTEX_POINT ( 'NONE', #5427 ) ;
#20570 = CIRCLE ( 'NONE', #104186, 0.06509327318403745899 ) ;
#20571 = CARTESIAN_POINT ( 'NONE',  ( 6.249999999999967137, 12.50000000000000000, -2.165063509461101710 ) ) ;
#20572 = CARTESIAN_POINT ( 'NONE',  ( -2.700000000000029932, 2.500000000000000000, -4.676537180435977881 ) ) ;
#20573 = DIRECTION ( 'NONE',  ( 0.000000000000000000, 0.000000000000000000, 1.000000000000000000 ) ) ;
#20574 =( GEOMETRIC_REPRESENTATION_CONTEXT ( 3 ) GLOBAL_UNCERTAINTY_ASSIGNED_CONTEXT ( ( #89864 ) ) GLOBAL_UNIT_ASSIGNED_CONTEXT ( ( #26307, #29522, #69430 ) ) REPRESENTATION_CONTEXT ( 'NONE', 'WORKASPACE' ) );
#20575 = ADVANCED_FACE ( 'NONE', ( #26379 ), #2509, .T. ) ;
#20576 = ORIENTED_EDGE ( 'NONE', *, *, #88592, .T. ) ;
#20577 = CIRCLE ( 'NONE', #31060, 0.06509327318403745899 ) ;
#20578 = CARTESIAN_POINT ( 'NONE',  ( -9.150000000000009237, 12.50000000000000000, -7.188010851410848723 ) ) ;
#20579 = VECTOR ( 'NONE', #49891, 1000.000000000000000 ) ;
#20580 = ORIENTED_EDGE ( 'NONE', *, *, #103912, .T. ) ;
#20581 = ORIENTED_EDGE ( 'NONE', *, *, #47067, .F. ) ;
#20582 = FACE_OUTER_BOUND ( 'NONE', #88489, .T. ) ;
#20583 = EDGE_LOOP ( 'NONE', ( #21812, #16321 ) ) ;
#20584 = AXIS2_PLACEMENT_3D ( 'NONE', #114014, #91789, #43349 ) ;
#20585 = DIRECTION ( 'NONE',  ( 0.000000000000000000, 0.000000000000000000, 1.000000000000000000 ) ) ;
#20586 = DIRECTION ( 'NONE',  ( 0.000000000000000000, 0.000000000000000000, 1.000000000000000000 ) ) ;
#20587 = ORIENTED_EDGE ( 'NONE', *, *, #9466, .T. ) ;
#20588 = FACE_OUTER_BOUND ( 'NONE', #67524, .T. ) ;
#20589 = ADVANCED_FACE ( 'NONE', ( #86567 ), #57111, .T. ) ;
#20590 = CARTESIAN_POINT ( 'NONE',  ( -5.400000000000024336, 12.50000000000000000, -3.702399969078687292 ) ) ;
#20591 = FACE_OUTER_BOUND ( 'NONE', #66634, .T. ) ;
#20592 = AXIS2_PLACEMENT_3D ( 'NONE', #38507, #9009, #36572 ) ;
#20593 = ORIENTED_EDGE ( 'NONE', *, *, #117412, .T. ) ;
#20594 = EDGE_CURVE ( 'NONE', #82955, #9027, #104911, .T. ) ;
#20596 = CIRCLE ( 'NONE', #81240, 0.06509327318403745899 ) ;
#20595 = CONICAL_SURFACE ( 'NONE', #110472, 0.1000000000000002554, 0.003490658503988666988 ) ;
#20597 = VERTEX_POINT ( 'NONE', #97043 ) ;
#20598 = EDGE_LOOP ( 'NONE', ( #96980, #107622, #105929, #25230 ) ) ;
#20599 = CARTESIAN_POINT ( 'NONE',  ( 1.449999999999949551, 12.50000000000000000, 6.841600689897072485 ) ) ;
#20600 = CARTESIAN_POINT ( 'NONE',  ( -3.950000000000026379, 12.50000000000000000, 6.906693963081109722 ) ) ;
#20601 = CARTESIAN_POINT ( 'NONE',  ( 17.50000000000000000, -2.500000000000000000, -3.999999999999998224 ) ) ;
#20602 = EDGE_CURVE ( 'NONE', #93533, #100605, #86127, .T. ) ;
#20603 = EDGE_CURVE ( 'NONE', #18475, #76431, #31787, .T. ) ;
#20604 = FACE_BOUND ( 'NONE', #35246, .T. ) ;
#20605 = ORIENTED_EDGE ( 'NONE', *, *, #13034, .F. ) ;
#20606 = ADVANCED_FACE ( 'NONE', ( #37494 ), #96379, .T. ) ;
#20607 = ADVANCED_FACE ( 'NONE', ( #117287 ), #121654, .T. ) ;
#20608 = DIRECTION ( 'NONE',  ( -0.000000000000000000, 1.000000000000000000, -0.000000000000000000 ) ) ;
#20609 = PLANE ( 'NONE',  #27202 ) ;
#20610 = ORIENTED_EDGE ( 'NONE', *, *, #122019, .F. ) ;
#20611 = DIRECTION ( 'NONE',  ( 0.000000000000000000, 1.000000000000000000, 0.000000000000000000 ) ) ;
#20612 = CARTESIAN_POINT ( 'NONE',  ( 17.02136413300363316, 1.939324994459781903, 5.540650668389440980 ) ) ;
#20613 = EDGE_CURVE ( 'NONE', #53623, #66905, #6694, .T. ) ;
#20614 = LINE ( 'NONE', #80174, #96687 ) ;
#20615 = DIRECTION ( 'NONE',  ( 0.000000000000000000, 1.000000000000000000, 0.000000000000000000 ) ) ;
#20616 = AXIS2_PLACEMENT_3D ( 'NONE', #100923, #80006, #91119 ) ;
#20617 = DIRECTION ( 'NONE',  ( 0.000000000000000000, 0.000000000000000000, -1.000000000000000000 ) ) ;
#20618 = EDGE_CURVE ( 'NONE', #41193, #49661, #65204, .T. ) ;
#20619 = FACE_OUTER_BOUND ( 'NONE', #120932, .T. ) ;
#20620 = DIRECTION ( 'NONE',  ( -0.000000000000000000, 1.000000000000000000, -0.000000000000000000 ) ) ;
#20621 = EDGE_CURVE ( 'NONE', #104101, #114153, #15023, .T. ) ;
#20622 = VECTOR ( 'NONE', #59701, 1000.000000000000000 ) ;
#20623 = ADVANCED_FACE ( 'NONE', ( #15892 ), #68215, .T. ) ;
#20624 = ORIENTED_EDGE ( 'NONE', *, *, #102174, .F. ) ;
#20625 = ORIENTED_EDGE ( 'NONE', *, *, #20448, .F. ) ;
#20626 = AXIS2_PLACEMENT_3D ( 'NONE', #22142, #20834, #122902 ) ;
#20627 = VERTEX_POINT ( 'NONE', #35558 ) ;
#20628 = VERTEX_POINT ( 'NONE', #75459 ) ;
#20629 = FACE_OUTER_BOUND ( 'NONE', #18352, .T. ) ;
#20630 = CARTESIAN_POINT ( 'NONE',  ( -14.59999999999998366, 12.50000000000000000, 0.6928203230275518099 ) ) ;
#20631 = EDGE_LOOP ( 'NONE', ( #31312, #81571 ) ) ;
#20632 = EDGE_CURVE ( 'NONE', #105063, #34708, #85913, .T. ) ;
#20633 = FACE_BOUND ( 'NONE', #21271, .T. ) ;
#20634 = EDGE_CURVE ( 'NONE', #64406, #55074, #90339, .T. ) ;
#20635 = LINE ( 'NONE', #10769, #87566 ) ;
#20636 = CONICAL_SURFACE ( 'NONE', #93790, 0.1000000000000002554, 0.003490658503988666988 ) ;
#20637 = CARTESIAN_POINT ( 'NONE',  ( 16.55874544816223448, 0.4845305829267578801, 6.091953208799004926 ) ) ;
#20638 = CONICAL_SURFACE ( 'NONE', #22799, 0.09999999999999982514, 0.003490658503988666988 ) ;
#20639 = AXIS2_PLACEMENT_3D ( 'NONE', #1470, #23058, #91155 ) ;
#20640 = CARTESIAN_POINT ( 'NONE',  ( -2.300000000000032685, 2.500000000000000000, -0.3464101615137783474 ) ) ;
#20641 = DIRECTION ( 'NONE',  ( 0.000000000000000000, 0.000000000000000000, 1.000000000000000000 ) ) ;
#20642 = CARTESIAN_POINT ( 'NONE',  ( -11.44999999999999929, 12.50000000000000000, -1.818653347947322141 ) ) ;
#20643 = CARTESIAN_POINT ( 'NONE',  ( -4.600000000000024514, 2.500000000000000000, 4.922947341949748257 ) ) ;
#20644 = CARTESIAN_POINT ( 'NONE',  ( -5.200000000000022382, 12.50000000000000000, 4.611443907251934426 ) ) ;
#20645 = DIRECTION ( 'NONE',  ( 0.000000000000000000, 0.000000000000000000, 1.000000000000000000 ) ) ;
#20646 = EDGE_LOOP ( 'NONE', ( #65292, #31151, #63012, #73116 ) ) ;
#20647 = CIRCLE ( 'NONE', #1844, 0.06509327318403745899 ) ;
#20648 = ORIENTED_EDGE ( 'NONE', *, *, #18720, .T. ) ;
#20649 = AXIS2_PLACEMENT_3D ( 'NONE', #92996, #43260, #21016 ) ;
#20650 = ORIENTED_EDGE ( 'NONE', *, *, #1246, .T. ) ;
#20651 = ORIENTED_EDGE ( 'NONE', *, *, #127596, .T. ) ;
#20652 = EDGE_LOOP ( 'NONE', ( #40408, #82359, #17756, #17668 ) ) ;
#20653 = EDGE_LOOP ( 'NONE', ( #25752, #79476, #100638, #68023 ) ) ;
#20654 = CARTESIAN_POINT ( 'NONE',  ( 3.949999999999941558, 2.500000000000000000, -6.148780366869526226 ) ) ;
#20655 = ORIENTED_EDGE ( 'NONE', *, *, #32292, .F. ) ;
#20656 = AXIS2_PLACEMENT_3D ( 'NONE', #34997, #85357, #15306 ) ;
#20657 = CARTESIAN_POINT ( 'NONE',  ( 10.84999999999990905, 12.50000000000000000, 2.099970236277060032 ) ) ;
#20658 = CARTESIAN_POINT ( 'NONE',  ( 184.3593750003413732, 0.000000000000000000, 7.564683531250000925 ) ) ;
#20659 = LINE ( 'NONE', #61223, #91771 ) ;
#20660 = CARTESIAN_POINT ( 'NONE',  ( 1.249999999999988898, 2.500000000000000000, -6.595190528383302109 ) ) ;
#20661 = AXIS2_PLACEMENT_3D ( 'NONE', #80603, #50486, #100241 ) ;
#20662 = ORIENTED_EDGE ( 'NONE', *, *, #85436, .T. ) ;
#20663 = CARTESIAN_POINT ( 'NONE',  ( -8.150000000000012790, 12.50000000000000000, 1.818653347947321475 ) ) ;
#20664 = VERTEX_POINT ( 'NONE', #30899 ) ;
#20665 = EDGE_CURVE ( 'NONE', #96497, #24701, #8772, .T. ) ;
#20666 = VERTEX_POINT ( 'NONE', #765 ) ;
#20667 = CONICAL_SURFACE ( 'NONE', #68768, 0.1000000000000002554, 0.003490658503988666988 ) ;
#20668 = CARTESIAN_POINT ( 'NONE',  ( -7.499999999999976907, 2.500000000000000000, 4.330127018922196314 ) ) ;
#20669 = EDGE_CURVE ( 'NONE', #92919, #117157, #1408, .T. ) ;
#20670 = FACE_OUTER_BOUND ( 'NONE', #129, .T. ) ;
#20671 = CARTESIAN_POINT ( 'NONE',  ( 10.39999999999990976, 12.50000000000000000, 4.330127018922196314 ) ) ;
#20672 = ORIENTED_EDGE ( 'NONE', *, *, #71394, .T. ) ;
#20673 = VECTOR ( 'NONE', #67669, 1000.000000000000000 ) ;
#20674 = VERTEX_POINT ( 'NONE', #59057 ) ;
#20675 = DIRECTION ( 'NONE',  ( 0.000000000000000000, 1.000000000000000000, 0.000000000000000000 ) ) ;
#20676 = AXIS2_PLACEMENT_3D ( 'NONE', #15729, #15061, #25542 ) ;
#20677 = LINE ( 'NONE', #109025, #95542 ) ;
#20678 = DIRECTION ( 'NONE',  ( 0.000000000000000000, 1.000000000000000000, 0.000000000000000000 ) ) ;
#20679 = LINE ( 'NONE', #22626, #35709 ) ;
#20680 = VERTEX_POINT ( 'NONE', #40059 ) ;
#20681 = CARTESIAN_POINT ( 'NONE',  ( 0.5999999999999612310, 2.500000000000000000, -0.2464101615137760659 ) ) ;
#20682 = AXIS2_PLACEMENT_3D ( 'NONE', #85368, #125297, #35635 ) ;
#20683 = ORIENTED_EDGE ( 'NONE', *, *, #43832, .F. ) ;
#20684 = CARTESIAN_POINT ( 'NONE',  ( 10.84999999999991260, 2.500000000000000000, 5.802370205355744659 ) ) ;
#20685 = ORIENTED_EDGE ( 'NONE', *, *, #65368, .T. ) ;
#20686 = DIRECTION ( 'NONE',  ( 0.000000000000000000, 0.000000000000000000, -1.000000000000000000 ) ) ;
#20687 = AXIS2_PLACEMENT_3D ( 'NONE', #50488, #39412, #19755 ) ;
#20688 = CARTESIAN_POINT ( 'NONE',  ( -11.44999999999999751, 12.50000000000000000, -2.511473670974873951 ) ) ;
#20689 = CARTESIAN_POINT ( 'NONE',  ( 130.5000000000000000, 0.5000000000000000000, 7.499999999999998224 ) ) ;
#20690 = AXIS2_PLACEMENT_3D ( 'NONE', #51541, #101919, #79691 ) ;
#20691 = CARTESIAN_POINT ( 'NONE',  ( 12.94999999999989981, 12.50000000000000000, -2.165063509461101710 ) ) ;
#20692 = VERTEX_POINT ( 'NONE', #81274 ) ;
#20693 = CARTESIAN_POINT ( 'NONE',  ( 6.649999999999930189, 2.500000000000000000, -1.472243186433550122 ) ) ;
#20695 = VECTOR ( 'NONE', #49566, 1000.000000000000000 ) ;
#20694 = AXIS2_PLACEMENT_3D ( 'NONE', #22164, #52250, #92159 ) ;
#20696 = DIRECTION ( 'NONE',  ( 0.000000000000000000, 0.000000000000000000, 1.000000000000000000 ) ) ;
#20697 = VERTEX_POINT ( 'NONE', #58423 ) ;
#20698 = ORIENTED_EDGE ( 'NONE', *, *, #55096, .T. ) ;
#20699 = VERTEX_POINT ( 'NONE', #98975 ) ;
#20700 = CARTESIAN_POINT ( 'NONE',  ( -1.050000000000037348, 2.500000000000000000, -6.941600689897078347 ) ) ;
#20701 = DIRECTION ( 'NONE',  ( 0.000000000000000000, 0.000000000000000000, 1.000000000000000000 ) ) ;
#20702 = FACE_OUTER_BOUND ( 'NONE', #60303, .T. ) ;
#20703 = CARTESIAN_POINT ( 'NONE',  ( 4.399999999999939071, 2.500000000000000000, -0.4464101615137782142 ) ) ;
#20704 = CARTESIAN_POINT ( 'NONE',  ( -7.100000000000018296, 2.500000000000000000, -2.385244779468109755E-15 ) ) ;
#20705 = ADVANCED_FACE ( 'NONE', ( #28960 ), #25502, .T. ) ;
#20706 = DIRECTION ( 'NONE',  ( 0.000000000000000000, 0.000000000000000000, -1.000000000000000000 ) ) ;
#20707 = CARTESIAN_POINT ( 'NONE',  ( 0.8499999999999557909, 12.50000000000000000, -6.495190528383302464 ) ) ;
#20708 = DIRECTION ( 'NONE',  ( 0.000000000000000000, -0.000000000000000000, 1.000000000000000000 ) ) ;
#20709 = CIRCLE ( 'NONE', #123109, 0.06509327318403745899 ) ;
#20710 = AXIS2_PLACEMENT_3D ( 'NONE', #18928, #49717, #40546 ) ;
#20711 = CIRCLE ( 'NONE', #37448, 0.06509327318403745899 ) ;
#20712 = EDGE_LOOP ( 'NONE', ( #72475, #110483, #14939, #58853 ) ) ;
#20713 = CARTESIAN_POINT ( 'NONE',  ( -7.900000000000014566, 2.500000000000000000, 0.6928203230275494784 ) ) ;
#20714 = ADVANCED_FACE ( 'NONE', ( #69498 ), #18476, .T. ) ;
#20716 = ADVANCED_FACE ( 'NONE', ( #108143 ), #8635, .T. ) ;
#20715 = DIRECTION ( 'NONE',  ( -4.274815082592931898E-19, -0.9999939076577903929, -0.003490651415223739937 ) ) ;
#20717 = DIRECTION ( 'NONE',  ( 0.000000000000000000, -0.9999939076577903929, 0.003490651415223739937 ) ) ;
#20718 = DIRECTION ( 'NONE',  ( 0.000000000000000000, -0.000000000000000000, 1.000000000000000000 ) ) ;
#20719 = AXIS2_PLACEMENT_3D ( 'NONE', #26509, #87334, #97172 ) ;
#20720 = ORIENTED_EDGE ( 'NONE', *, *, #29630, .F. ) ;
#20721 = AXIS2_PLACEMENT_3D ( 'NONE', #59507, #19546, #31324 ) ;
#20722 = CARTESIAN_POINT ( 'NONE',  ( -3.150000000000029221, 2.500000000000000000, -1.818653347947326138 ) ) ;
#20723 = VECTOR ( 'NONE', #119824, 1000.000000000000000 ) ;
#20724 = CARTESIAN_POINT ( 'NONE',  ( -5.400000000000024336, 12.50000000000000000, -3.637306695894650055 ) ) ;
#20726 = EDGE_LOOP ( 'NONE', ( #125158, #99235, #85175, #44838 ) ) ;
#20725 = DIRECTION ( 'NONE',  ( 0.000000000000000000, 0.000000000000000000, 1.000000000000000000 ) ) ;
#20727 = ADVANCED_FACE ( 'NONE', ( #11224 ), #55914, .T. ) ;
#20728 = AXIS2_PLACEMENT_3D ( 'NONE', #14615, #53294, #84668 ) ;
#20729 = ORIENTED_EDGE ( 'NONE', *, *, #72016, .T. ) ;
#20730 = DIRECTION ( 'NONE',  ( 0.000000000000000000, -0.9999939076577903929, 0.003490651415223739937 ) ) ;
#20731 = AXIS2_PLACEMENT_3D ( 'NONE', #72561, #92175, #31350 ) ;
#20732 = ORIENTED_EDGE ( 'NONE', *, *, #117314, .F. ) ;
#20733 = ORIENTED_EDGE ( 'NONE', *, *, #80608, .F. ) ;
#20734 = FACE_OUTER_BOUND ( 'NONE', #118773, .T. ) ;
#20735 = CARTESIAN_POINT ( 'NONE',  ( 21.15177371151439090, 2.593223176056364210, -4.151029080743463773 ) ) ;
#20736 = CARTESIAN_POINT ( 'NONE',  ( -7.950000000000012612, 12.50000000000000000, -2.230156782645139391 ) ) ;
#20737 = FACE_OUTER_BOUND ( 'NONE', #24058, .T. ) ;
#20738 = EDGE_LOOP ( 'NONE', ( #89083, #125224, #110788, #58151 ) ) ;
#20739 = DIRECTION ( 'NONE',  ( -0.000000000000000000, -1.000000000000000000, -0.000000000000000000 ) ) ;
#20740 = ORIENTED_EDGE ( 'NONE', *, *, #88120, .T. ) ;
#20741 = VECTOR ( 'NONE', #120206, 1000.000000000000000 ) ;
#20742 = LINE ( 'NONE', #30582, #95577 ) ;
#20743 = CYLINDRICAL_SURFACE ( 'NONE', #81993, 5.000000000000004441 ) ;
#20744 = CARTESIAN_POINT ( 'NONE',  ( 16.80072262464533139, -1.717570462274074838, 5.816823748342618394 ) ) ;
#20745 = ORIENTED_EDGE ( 'NONE', *, *, #46690, .T. ) ;
#20746 = EDGE_CURVE ( 'NONE', #17252, #95053, #39348, .T. ) ;
#20747 = ORIENTED_EDGE ( 'NONE', *, *, #87828, .F. ) ;
#20748 = ORIENTED_EDGE ( 'NONE', *, *, #121508, .F. ) ;
#20749 = ORIENTED_EDGE ( 'NONE', *, *, #2884, .T. ) ;
#20750 = FACE_OUTER_BOUND ( 'NONE', #104807, .T. ) ;
#20751 = CARTESIAN_POINT ( 'NONE',  ( 16.04744069018201458, 1.499999999999809042, 6.586254744912538150 ) ) ;
#20752 = CARTESIAN_POINT ( 'NONE',  ( -11.24999999999996270, 12.50000000000000000, 6.430097255199259010 ) ) ;
#20753 = EDGE_CURVE ( 'NONE', #106287, #18828, #81936, .T. ) ;
#20754 = FACE_BOUND ( 'NONE', #86902, .T. ) ;
#20755 = CARTESIAN_POINT ( 'NONE',  ( 7.499999999999927169, 2.500000000000000000, -5.122947341949753763 ) ) ;
#20756 = FACE_OUTER_BOUND ( 'NONE', #10595, .T. ) ;
#20757 = AXIS2_PLACEMENT_3D ( 'NONE', #60468, #80084, #118713 ) ;
#20758 = EDGE_CURVE ( 'NONE', #63832, #87480, #98875, .T. ) ;
#20759 = LINE ( 'NONE', #12213, #101257 ) ;
#20760 = DIRECTION ( 'NONE',  ( 0.000000000000000000, 0.000000000000000000, -1.000000000000000000 ) ) ;
#20761 = EDGE_CURVE ( 'NONE', #68129, #119603, #59631, .T. ) ;
#20762 = DIRECTION ( 'NONE',  ( 0.000000000000000000, 1.000000000000000000, 0.000000000000000000 ) ) ;
#20763 = EDGE_CURVE ( 'NONE', #101014, #51535, #48494, .T. ) ;
#20764 = CARTESIAN_POINT ( 'NONE',  ( -11.44999999999999751, 12.50000000000000000, 6.148780366869520897 ) ) ;
#20765 = AXIS2_PLACEMENT_3D ( 'NONE', #16611, #106926, #57857 ) ;
#20766 = EDGE_CURVE ( 'NONE', #112120, #114810, #42253, .T. ) ;
#20767 = DIRECTION ( 'NONE',  ( -0.000000000000000000, 1.000000000000000000, -0.000000000000000000 ) ) ;
#20768 = EDGE_CURVE ( 'NONE', #42757, #103996, #58975, .T. ) ;
#20769 = DIRECTION ( 'NONE',  ( 0.000000000000000000, 1.000000000000000000, 0.000000000000000000 ) ) ;
#20772 = EDGE_CURVE ( 'NONE', #32556, #108826, #119165, .T. ) ;
#20771 = AXIS2_PLACEMENT_3D ( 'NONE', #107196, #77725, #16221 ) ;
#20770 = AXIS2_PLACEMENT_3D ( 'NONE', #405, #12802, #39738 ) ;
#20773 = VERTEX_POINT ( 'NONE', #29504 ) ;
#20774 = ORIENTED_EDGE ( 'NONE', *, *, #83446, .F. ) ;
#20775 = EDGE_LOOP ( 'NONE', ( #75398, #35275 ) ) ;
#20776 = EDGE_LOOP ( 'NONE', ( #54107, #91308 ) ) ;
#20777 = DIRECTION ( 'NONE',  ( 0.000000000000000000, 1.000000000000000000, 0.000000000000000000 ) ) ;
#20778 = AXIS2_PLACEMENT_3D ( 'NONE', #66490, #16725, #56658 ) ;
#20779 = CARTESIAN_POINT ( 'NONE',  ( -5.800000000000022027, 12.50000000000000000, -4.330127018922201643 ) ) ;
#20780 = VERTEX_POINT ( 'NONE', #69410 ) ;
#20781 = FACE_BOUND ( 'NONE', #116104, .T. ) ;
#20782 = EDGE_CURVE ( 'NONE', #16737, #11179, #38130, .T. ) ;
#20783 = FACE_OUTER_BOUND ( 'NONE', #13952, .T. ) ;
#20785 = CIRCLE ( 'NONE', #64595, 0.1000000000000000472 ) ;
#20784 = AXIS2_PLACEMENT_3D ( 'NONE', #47587, #78343, #46951 ) ;
#20786 = EDGE_LOOP ( 'NONE', ( #1151, #6783, #114498, #42864 ) ) ;
#20787 = FACE_OUTER_BOUND ( 'NONE', #110259, .T. ) ;
#20788 = CARTESIAN_POINT ( 'NONE',  ( 4.549999999999939426, 2.500000000000000000, -6.595190528383302109 ) ) ;
#20789 = LINE ( 'NONE', #49619, #124219 ) ;
#20790 = FACE_OUTER_BOUND ( 'NONE', #49300, .T. ) ;
#20791 = ORIENTED_EDGE ( 'NONE', *, *, #17921, .F. ) ;
#20792 = DIRECTION ( 'NONE',  ( 0.000000000000000000, 0.000000000000000000, 1.000000000000000000 ) ) ;
#20793 = EDGE_LOOP ( 'NONE', ( #66660, #14510 ) ) ;
#20794 = EDGE_LOOP ( 'NONE', ( #38465, #44854 ) ) ;
#20795 = CONICAL_SURFACE ( 'NONE', #129487, 0.1000000000000002554, 0.003490658503988666988 ) ;
#20796 = DIRECTION ( 'NONE',  ( 0.000000000000000000, 0.000000000000000000, -1.000000000000000000 ) ) ;
#20797 = CARTESIAN_POINT ( 'NONE',  ( 14.39999999999989555, 2.500000000000000000, 0.4464101615137736623 ) ) ;
#20798 = VERTEX_POINT ( 'NONE', #9862 ) ;
#20799 = CARTESIAN_POINT ( 'NONE',  ( 9.349999999999919709, 2.500000000000000000, -6.941600689897078347 ) ) ;
#20800 = AXIS2_PLACEMENT_3D ( 'NONE', #66595, #44380, #126166 ) ;
#20801 = DIRECTION ( 'NONE',  ( -0.000000000000000000, -1.000000000000000000, -0.000000000000000000 ) ) ;
#20802 = AXIS2_PLACEMENT_3D ( 'NONE', #25349, #65927, #45666 ) ;
#20803 = DIRECTION ( 'NONE',  ( 0.000000000000000000, 0.000000000000000000, 1.000000000000000000 ) ) ;
#20804 = DIRECTION ( 'NONE',  ( 0.000000000000000000, 0.000000000000000000, 1.000000000000000000 ) ) ;
#20805 = ORIENTED_EDGE ( 'NONE', *, *, #2418, .T. ) ;
#20806 = DIRECTION ( 'NONE',  ( 0.000000000000000000, 0.000000000000000000, 1.000000000000000000 ) ) ;
#20808 = ORIENTED_EDGE ( 'NONE', *, *, #111801, .F. ) ;
#20807 = AXIS2_PLACEMENT_3D ( 'NONE', #46622, #47286, #105556 ) ;
#20809 = CARTESIAN_POINT ( 'NONE',  ( -3.300000000000027800, 2.500000000000000000, -2.276824562219559311E-15 ) ) ;
#20810 = AXIS2_PLACEMENT_3D ( 'NONE', #110975, #50791, #52088 ) ;
#20811 = CIRCLE ( 'NONE', #81453, 0.1000000000000002554 ) ;
#20812 = ORIENTED_EDGE ( 'NONE', *, *, #67084, .F. ) ;
#20813 = ADVANCED_FACE ( 'NONE', ( #49802 ), #52704, .T. ) ;
#20814 = CARTESIAN_POINT ( 'NONE',  ( 162.5000000000000000, -0.5000000000000000000, 7.499999999999994671 ) ) ;
#20815 = ORIENTED_EDGE ( 'NONE', *, *, #1538, .F. ) ;
#20816 = CARTESIAN_POINT ( 'NONE',  ( -10.60000000000000142, 2.500000000000000000, -0.3464101615137782364 ) ) ;
#20817 = LINE ( 'NONE', #30000, #6887 ) ;
#20818 = DIRECTION ( 'NONE',  ( 0.000000000000000000, 0.000000000000000000, 1.000000000000000000 ) ) ;
#20819 = DIRECTION ( 'NONE',  ( 0.000000000000000000, -0.000000000000000000, 1.000000000000000000 ) ) ;
#20820 = LINE ( 'NONE', #30005, #55843 ) ;
#20821 = AXIS2_PLACEMENT_3D ( 'NONE', #1437, #41389, #60390 ) ;
#20822 = ORIENTED_EDGE ( 'NONE', *, *, #67670, .F. ) ;
#20823 = ORIENTED_EDGE ( 'NONE', *, *, #114450, .F. ) ;
#20824 = ADVANCED_FACE ( 'NONE', ( #79885 ), #125851, .T. ) ;
#20826 = ORIENTED_EDGE ( 'NONE', *, *, #114042, .F. ) ;
#20825 = CONICAL_SURFACE ( 'NONE', #85568, 0.1000000000000002554, 0.003490658503988666988 ) ;
#20827 = LINE ( 'NONE', #3122, #103941 ) ;
#20828 = AXIS2_PLACEMENT_3D ( 'NONE', #98983, #76772, #107517 ) ;
#20829 = DIRECTION ( 'NONE',  ( 0.000000000000000000, 0.000000000000000000, -1.000000000000000000 ) ) ;
#20830 = DIRECTION ( 'NONE',  ( -0.000000000000000000, -1.000000000000000000, -0.000000000000000000 ) ) ;
#20832 = EDGE_LOOP ( 'NONE', ( #64360, #95852, #4525, #13737 ) ) ;
#20831 = ORIENTED_EDGE ( 'NONE', *, *, #31680, .T. ) ;
#20833 = ORIENTED_EDGE ( 'NONE', *, *, #117567, .T. ) ;
#20834 = DIRECTION ( 'NONE',  ( 0.000000000000000000, 1.000000000000000000, 0.000000000000000000 ) ) ;
#20835 = ORIENTED_EDGE ( 'NONE', *, *, #51487, .T. ) ;
#20836 = DIRECTION ( 'NONE',  ( -0.000000000000000000, -1.000000000000000000, -0.000000000000000000 ) ) ;
#20837 = DIRECTION ( 'NONE',  ( -0.000000000000000000, -1.000000000000000000, -0.000000000000000000 ) ) ;
#20838 = DIRECTION ( 'NONE',  ( 0.000000000000000000, 0.000000000000000000, 1.000000000000000000 ) ) ;
#20839 = DIRECTION ( 'NONE',  ( 0.000000000000000000, 0.000000000000000000, 1.000000000000000000 ) ) ;
#20840 = CARTESIAN_POINT ( 'NONE',  ( 1.249999999999952038, 2.500000000000000000, 5.702370205355745014 ) ) ;
#20841 = CIRCLE ( 'NONE', #125388, 0.09999999999999999167 ) ;
#20842 = CARTESIAN_POINT ( 'NONE',  ( -13.54999999999999005, 2.500000000000000000, 2.611473670974877148 ) ) ;
#20843 = CARTESIAN_POINT ( 'NONE',  ( -1.850000000000033840, 12.50000000000000000, 2.511473670974873507 ) ) ;
#20844 = VERTEX_POINT ( 'NONE', #50422 ) ;
#20845 = ORIENTED_EDGE ( 'NONE', *, *, #112935, .F. ) ;
#20846 = DIRECTION ( 'NONE',  ( 0.000000000000000000, 1.000000000000000000, 0.000000000000000000 ) ) ;
#20847 = DIRECTION ( 'NONE',  ( 0.000000000000000000, 0.000000000000000000, -1.000000000000000000 ) ) ;
#20848 = ORIENTED_EDGE ( 'NONE', *, *, #100827, .F. ) ;
#20849 = EDGE_LOOP ( 'NONE', ( #121215, #123301, #12505, #36728, #102631, #23065, #104870, #2466, #116863, #78782, #21989, #11648, #39065 ) ) ;
#20850 = DIRECTION ( 'NONE',  ( -0.000000000000000000, 1.000000000000000000, -0.000000000000000000 ) ) ;
#20851 = DIRECTION ( 'NONE',  ( -0.000000000000000000, -1.000000000000000000, -0.000000000000000000 ) ) ;
#20852 = DIRECTION ( 'NONE',  ( 0.000000000000000000, -0.9999939076577903929, 0.003490651415223739937 ) ) ;
#20853 = DIRECTION ( 'NONE',  ( 0.000000000000000000, 0.000000000000000000, 1.000000000000000000 ) ) ;
#20854 = ADVANCED_FACE ( 'NONE', ( #68122 ), #128013, .T. ) ;
#20855 = CARTESIAN_POINT ( 'NONE',  ( -1.900000000000034106, 2.500000000000000000, 0.4464101615137735513 ) ) ;
#20856 = DIRECTION ( 'NONE',  ( 0.000000000000000000, 0.000000000000000000, 1.000000000000000000 ) ) ;
#20857 = DIRECTION ( 'NONE',  ( 0.000000000000000000, 0.000000000000000000, 1.000000000000000000 ) ) ;
#20858 = VECTOR ( 'NONE', #30015, 1000.000000000000000 ) ;
#20859 = FACE_OUTER_BOUND ( 'NONE', #2781, .T. ) ;
#20860 = EDGE_CURVE ( 'NONE', #36385, #26275, #450, .T. ) ;
#20861 = ORIENTED_EDGE ( 'NONE', *, *, #111016, .F. ) ;
#20862 = EDGE_LOOP ( 'NONE', ( #5491, #70455, #15556, #115935 ) ) ;
#20864 = AXIS2_PLACEMENT_3D ( 'NONE', #105766, #106399, #27191 ) ;
#20863 = AXIS2_PLACEMENT_3D ( 'NONE', #97823, #76903, #46807 ) ;
#20865 = EDGE_LOOP ( 'NONE', ( #51869, #53400 ) ) ;
#20866 = AXIS2_PLACEMENT_3D ( 'NONE', #108195, #6123, #86626 ) ;
#20867 = EDGE_CURVE ( 'NONE', #107780, #7939, #115464, .T. ) ;
#20868 = EDGE_LOOP ( 'NONE', ( #31081, #95699 ) ) ;
#20869 = ORIENTED_EDGE ( 'NONE', *, *, #88633, .F. ) ;
#20870 = EDGE_CURVE ( 'NONE', #4913, #47413, #70710, .T. ) ;
#20871 = CARTESIAN_POINT ( 'NONE',  ( 8.349999999999919709, 12.50000000000000000, -2.792790559304616504 ) ) ;
#20872 = DIRECTION ( 'NONE',  ( 0.000000000000000000, 0.000000000000000000, 1.000000000000000000 ) ) ;
#20875 = EDGE_LOOP ( 'NONE', ( #53444, #64861 ) ) ;
#20874 = CONICAL_SURFACE ( 'NONE', #24982, 0.09999999999999982514, 0.003490658503988666988 ) ;
#20873 = VECTOR ( 'NONE', #27282, 1000.000000000000000 ) ;
#20876 = FACE_OUTER_BOUND ( 'NONE', #72331, .T. ) ;
#20877 = CARTESIAN_POINT ( 'NONE',  ( 186.2812500006828031, 0.000000000000000000, 7.700000000000000178 ) ) ;
#20878 = EDGE_CURVE ( 'NONE', #25375, #107896, #51090, .T. ) ;
#20879 = DIRECTION ( 'NONE',  ( 0.000000000000000000, 0.000000000000000000, 1.000000000000000000 ) ) ;
#20881 = EDGE_LOOP ( 'NONE', ( #103033, #86786, #2097, #114002 ) ) ;
#20880 = DIRECTION ( 'NONE',  ( 0.000000000000000000, 1.000000000000000000, 0.000000000000000000 ) ) ;
#20882 = EDGE_CURVE ( 'NONE', #107817, #79702, #41272, .T. ) ;
#20883 = CARTESIAN_POINT ( 'NONE',  ( -7.900000000000011013, 12.50000000000000000, 5.022947341949748790 ) ) ;
#20884 = CARTESIAN_POINT ( 'NONE',  ( -15.39999999999997904, 12.50000000000000000, -0.7579135962115893799 ) ) ;
#20885 = ORIENTED_EDGE ( 'NONE', *, *, #22412, .T. ) ;
#20886 = EDGE_LOOP ( 'NONE', ( #4899, #82580, #60703, #21145 ) ) ;
#20887 = EDGE_LOOP ( 'NONE', ( #62568, #9907, #34876, #27049, #46775, #88866, #993, #62239 ) ) ;
#20888 = VERTEX_POINT ( 'NONE', #123655 ) ;
#20889 = DIRECTION ( 'NONE',  ( 0.000000000000000000, 0.000000000000000000, 1.000000000000000000 ) ) ;
#20890 = FACE_OUTER_BOUND ( 'NONE', #18574, .T. ) ;
#20891 = CARTESIAN_POINT ( 'NONE',  ( -0.8500000000000386136, 2.500000000000000000, 1.572243186433545548 ) ) ;
#20892 = AXIS2_PLACEMENT_3D ( 'NONE', #14592, #2197, #72892 ) ;
#20893 = VECTOR ( 'NONE', #5485, 1000.000000000000000 ) ;
#20894 = DIRECTION ( 'NONE',  ( 0.000000000000000000, -0.9999939076577903929, 0.003490651415223739937 ) ) ;
#20895 = VERTEX_POINT ( 'NONE', #1954 ) ;
#20896 = CARTESIAN_POINT ( 'NONE',  ( -3.100000000000028511, 2.500000000000000000, -3.983716857408426293 ) ) ;
#20897 = CARTESIAN_POINT ( 'NONE',  ( -12.89999999999999147, 2.500000000000000000, 3.737306695894644371 ) ) ;
#20898 = LINE ( 'NONE', #42488, #31699 ) ;
#20899 = DIRECTION ( 'NONE',  ( 0.000000000000000000, -0.000000000000000000, 1.000000000000000000 ) ) ;
#20900 = CIRCLE ( 'NONE', #66860, 0.1000000000000002554 ) ;
#20901 = ORIENTED_EDGE ( 'NONE', *, *, #104937, .F. ) ;
#20902 = ORIENTED_EDGE ( 'NONE', *, *, #42664, .F. ) ;
#20903 = ORIENTED_EDGE ( 'NONE', *, *, #127473, .T. ) ;
#20904 = CARTESIAN_POINT ( 'NONE',  ( -0.8500000000000382805, 12.50000000000000000, -2.857883832488653741 ) ) ;
#20905 = CARTESIAN_POINT ( 'NONE',  ( -7.950000000000016165, 2.500000000000000000, -6.495190528383297135 ) ) ;
#20906 = FACE_BOUND ( 'NONE', #4883, .T. ) ;
#20907 = AXIS2_PLACEMENT_3D ( 'NONE', #22394, #93060, #74053 ) ;
#20908 = DIRECTION ( 'NONE',  ( -0.000000000000000000, -1.000000000000000000, -0.000000000000000000 ) ) ;
#20909 = DIRECTION ( 'NONE',  ( 0.000000000000000000, 1.000000000000000000, 0.000000000000000000 ) ) ;
#20910 = EDGE_CURVE ( 'NONE', #28738, #64836, #107162, .T. ) ;
#20911 = CARTESIAN_POINT ( 'NONE',  ( 3.949999999999941558, 2.500000000000000000, -1.918653347947326004 ) ) ;
#20912 = AXIS2_PLACEMENT_3D ( 'NONE', #30887, #108765, #1395 ) ;
#20913 = AXIS2_PLACEMENT_3D ( 'NONE', #35408, #94303, #93675 ) ;
#20914 = EDGE_CURVE ( 'NONE', #94964, #4541, #44477, .T. ) ;
#20915 = EDGE_CURVE ( 'NONE', #98238, #63941, #56981, .T. ) ;
#20916 = DIRECTION ( 'NONE',  ( -0.000000000000000000, -1.000000000000000000, -0.000000000000000000 ) ) ;
#20917 = AXIS2_PLACEMENT_3D ( 'NONE', #126414, #117862, #79257 ) ;
#20918 = DIRECTION ( 'NONE',  ( 0.000000000000000000, -0.000000000000000000, 1.000000000000000000 ) ) ;
#20919 = EDGE_CURVE ( 'NONE', #30265, #119631, #123889, .T. ) ;
#20920 = CARTESIAN_POINT ( 'NONE',  ( -14.14999999999998792, 2.500000000000000000, -1.472243186433547901 ) ) ;
#20921 = EDGE_LOOP ( 'NONE', ( #54843, #44426 ) ) ;
#20923 = ADVANCED_FACE ( 'NONE', ( #104042 ), #61213, .T. ) ;
#20922 = AXIS2_PLACEMENT_3D ( 'NONE', #125684, #76604, #36038 ) ;
#20924 = LINE ( 'NONE', #92223, #38674 ) ;
#20925 = DIRECTION ( 'NONE',  ( 0.000000000000000000, -0.000000000000000000, 1.000000000000000000 ) ) ;
#20926 = EDGE_CURVE ( 'NONE', #110378, #15661, #123042, .T. ) ;
#20927 = AXIS2_PLACEMENT_3D ( 'NONE', #82448, #80508, #61516 ) ;
#20928 = EDGE_LOOP ( 'NONE', ( #90225, #73477 ) ) ;
#20929 = ORIENTED_EDGE ( 'NONE', *, *, #43334, .T. ) ;
#20930 = DIRECTION ( 'NONE',  ( 0.000000000000000000, -0.000000000000000000, 1.000000000000000000 ) ) ;
#20931 = DIRECTION ( 'NONE',  ( 0.000000000000000000, 1.000000000000000000, 0.000000000000000000 ) ) ;
#20932 = FACE_BOUND ( 'NONE', #13961, .T. ) ;
#20933 = CARTESIAN_POINT ( 'NONE',  ( -9.999999999999969802, 12.50000000000000000, 4.330127018922196314 ) ) ;
#20934 = EDGE_CURVE ( 'NONE', #8949, #15822, #94215, .T. ) ;
#20935 = ADVANCED_FACE ( 'NONE', ( #13708 ), #27748, .T. ) ;
#20936 = DIRECTION ( 'NONE',  ( 0.000000000000000000, 0.000000000000000000, 1.000000000000000000 ) ) ;
#20937 = ORIENTED_EDGE ( 'NONE', *, *, #37308, .T. ) ;
#20938 = CARTESIAN_POINT ( 'NONE',  ( 9.149999999999920419, 2.500000000000000000, -5.702370205355749455 ) ) ;
#20939 = CARTESIAN_POINT ( 'NONE',  ( 185.4166666666666856, 6.668395609140176816, 3.850000000000000977 ) ) ;
#20940 = ORIENTED_EDGE ( 'NONE', *, *, #34948, .T. ) ;
#20941 = CARTESIAN_POINT ( 'NONE',  ( -4.350000000000023626, 2.500000000000000000, 6.741600689897071952 ) ) ;
#20942 = DIRECTION ( 'NONE',  ( 0.000000000000000000, 0.000000000000000000, 1.000000000000000000 ) ) ;
#20943 = AXIS2_PLACEMENT_3D ( 'NONE', #52077, #41627, #80248 ) ;
#20944 = CARTESIAN_POINT ( 'NONE',  ( -2.499999999999996003, 2.500000000000000000, -0.1000000000000022815 ) ) ;
#20945 = CIRCLE ( 'NONE', #62811, 0.06509327318403745899 ) ;
#20946 = DIRECTION ( 'NONE',  ( -0.000000000000000000, 1.000000000000000000, -0.000000000000000000 ) ) ;
#20947 = EDGE_CURVE ( 'NONE', #40320, #86459, #111354, .T. ) ;
#20948 = EDGE_LOOP ( 'NONE', ( #22990, #24224, #98646, #53921 ) ) ;
#20949 = CARTESIAN_POINT ( 'NONE',  ( 8.549999999999922551, 2.500000000000000000, -6.148780366869526226 ) ) ;
#20951 = AXIS2_PLACEMENT_3D ( 'NONE', #103017, #102391, #103684 ) ;
#20950 = VECTOR ( 'NONE', #22517, 1000.000000000000000 ) ;
#20952 = LINE ( 'NONE', #62183, #62241 ) ;
#20953 = FACE_OUTER_BOUND ( 'NONE', #11613, .T. ) ;
#20954 = EDGE_LOOP ( 'NONE', ( #80150, #43283 ) ) ;
#20955 = ORIENTED_EDGE ( 'NONE', *, *, #34648, .T. ) ;
#20956 = DIRECTION ( 'NONE',  ( 0.000000000000000000, 0.000000000000000000, 1.000000000000000000 ) ) ;
#20957 = EDGE_LOOP ( 'NONE', ( #46445, #100482 ) ) ;
#20958 = LINE ( 'NONE', #42556, #28418 ) ;
#20960 = CARTESIAN_POINT ( 'NONE',  ( -10.00000000000000711, 12.50000000000000000, -3.702399969078682851 ) ) ;
#20959 = CIRCLE ( 'NONE', #117087, 0.1000000000000002554 ) ;
#20961 = DIRECTION ( 'NONE',  ( 0.000000000000000000, 0.000000000000000000, 1.000000000000000000 ) ) ;
#20962 = VERTEX_POINT ( 'NONE', #14350 ) ;
#20963 = FACE_OUTER_BOUND ( 'NONE', #106378, .T. ) ;
#20964 = DIRECTION ( 'NONE',  ( 0.000000000000000000, 0.000000000000000000, 1.000000000000000000 ) ) ;
#20965 = DIRECTION ( 'NONE',  ( 0.000000000000000000, 1.000000000000000000, 0.000000000000000000 ) ) ;
#20966 = PLANE ( 'NONE',  #87275 ) ;
#20967 = CARTESIAN_POINT ( 'NONE',  ( -0.8000000000000376810, 12.50000000000000000, -4.330127018922201643 ) ) ;
#20968 = FACE_OUTER_BOUND ( 'NONE', #9038, .T. ) ;
#20969 = ORIENTED_EDGE ( 'NONE', *, *, #123836, .T. ) ;
#20970 = EDGE_CURVE ( 'NONE', #72461, #92222, #13060, .T. ) ;
#20971 = ORIENTED_EDGE ( 'NONE', *, *, #26086, .F. ) ;
#20972 = DIRECTION ( 'NONE',  ( 0.000000000000000000, 0.000000000000000000, -1.000000000000000000 ) ) ;
#20973 = ORIENTED_EDGE ( 'NONE', *, *, #53627, .T. ) ;
#20974 = CARTESIAN_POINT ( 'NONE',  ( -0.6500000000000398792, 12.50000000000000000, -2.446380397790840266 ) ) ;
#20976 = ORIENTED_EDGE ( 'NONE', *, *, #58616, .F. ) ;
#20975 = ORIENTED_EDGE ( 'NONE', *, *, #41783, .F. ) ;
#20977 = ORIENTED_EDGE ( 'NONE', *, *, #11829, .F. ) ;
#20978 = CARTESIAN_POINT ( 'NONE',  ( 17.50000000000000000, -2.500000000000000000, -3.999999999999998224 ) ) ;
#20979 = CONICAL_SURFACE ( 'NONE', #94136, 0.1000000000000000472, 0.003490658503988666988 ) ;
#20980 = CARTESIAN_POINT ( 'NONE',  ( 2.699999999999947331, 12.50000000000000000, -0.3464101615137783474 ) ) ;
#20981 = AXIS2_PLACEMENT_3D ( 'NONE', #69271, #29381, #31319 ) ;
#20982 = DIRECTION ( 'NONE',  ( 0.000000000000000000, 1.000000000000000000, 0.000000000000000000 ) ) ;
#20983 = SHAPE_REPRESENTATION_RELATIONSHIP ( 'NONE' , 'NONE' ,  #120523, #2393 ) ;
#20984 = DIRECTION ( 'NONE',  ( 0.000000000000000000, 0.000000000000000000, 1.000000000000000000 ) ) ;
#20985 = CARTESIAN_POINT ( 'NONE',  ( -1.900000000000034106, 12.50000000000000000, 0.3464101615137735735 ) ) ;
#20986 = CARTESIAN_POINT ( 'NONE',  ( 195.5000000000000000, 0.000000000000000000, 0.000000000000000000 ) ) ;
#20987 = DIRECTION ( 'NONE',  ( -0.000000000000000000, -1.000000000000000000, -0.000000000000000000 ) ) ;
#20988 = CARTESIAN_POINT ( 'NONE',  ( -10.45000000000000107, 2.500000000000000000, 2.165063509461097713 ) ) ;
#20990 = VECTOR ( 'NONE', #20894, 1000.000000000000000 ) ;
#20989 = FACE_OUTER_BOUND ( 'NONE', #58232, .T. ) ;
#20991 = EDGE_LOOP ( 'NONE', ( #114354, #124895, #103496, #2214 ) ) ;
#20992 = CARTESIAN_POINT ( 'NONE',  ( -10.45000000000000107, 12.50000000000000000, 6.560283801567334372 ) ) ;
#20993 = ORIENTED_EDGE ( 'NONE', *, *, #30138, .T. ) ;
#20994 = ORIENTED_EDGE ( 'NONE', *, *, #126123, .T. ) ;
#20995 = LINE ( 'NONE', #58368, #41975 ) ;
#20996 = CARTESIAN_POINT ( 'NONE',  ( 6.899999999999928413, 2.500000000000000000, 4.776537180435972196 ) ) ;
#20997 = CIRCLE ( 'NONE', #66948, 0.09999999999999982514 ) ;
#20998 = DIRECTION ( 'NONE',  ( 0.000000000000000000, 0.000000000000000000, -1.000000000000000000 ) ) ;
#20999 = VECTOR ( 'NONE', #52301, 1000.000000000000000 ) ;
#21000 = DIRECTION ( 'NONE',  ( 0.000000000000000000, 0.000000000000000000, 1.000000000000000000 ) ) ;
#21001 = DIRECTION ( 'NONE',  ( -0.000000000000000000, 1.000000000000000000, -0.000000000000000000 ) ) ;
#21002 = DIRECTION ( 'NONE',  ( 0.000000000000000000, 0.000000000000000000, 1.000000000000000000 ) ) ;
#21003 = ORIENTED_EDGE ( 'NONE', *, *, #103168, .F. ) ;
#21004 = AXIS2_PLACEMENT_3D ( 'NONE', #91581, #112520, #21553 ) ;
#21005 = VERTEX_POINT ( 'NONE', #73281 ) ;
#21006 = DIRECTION ( 'NONE',  ( 0.000000000000000000, 0.000000000000000000, 1.000000000000000000 ) ) ;
#21007 = ADVANCED_FACE ( 'NONE', ( #112581 ), #25589, .T. ) ;
#21008 = VERTEX_POINT ( 'NONE', #102729 ) ;
#21009 = LINE ( 'NONE', #53549, #46255 ) ;
#21010 = AXIS2_PLACEMENT_3D ( 'NONE', #124765, #95946, #27849 ) ;
#21011 = VERTEX_POINT ( 'NONE', #22910 ) ;
#21012 = EDGE_CURVE ( 'NONE', #91607, #71034, #86227, .T. ) ;
#21013 = ORIENTED_EDGE ( 'NONE', *, *, #76937, .T. ) ;
#21014 = EDGE_CURVE ( 'NONE', #87232, #5884, #121097, .T. ) ;
#21015 = CARTESIAN_POINT ( 'NONE',  ( -0.4000000000000396572, 2.500000000000000000, 4.230127018922196669 ) ) ;
#21016 = DIRECTION ( 'NONE',  ( 0.000000000000000000, 0.000000000000000000, 1.000000000000000000 ) ) ;
#21017 = DIRECTION ( 'NONE',  ( 0.000000000000000000, 0.000000000000000000, -1.000000000000000000 ) ) ;
#21018 = DIRECTION ( 'NONE',  ( 0.000000000000000000, 1.000000000000000000, 0.000000000000000000 ) ) ;
#21019 = EDGE_CURVE ( 'NONE', #122356, #108389, #8862, .T. ) ;
#21020 = CARTESIAN_POINT ( 'NONE',  ( 87.50000000000001421, -3.974992050023846257, 6.359987280038160939 ) ) ;
#21022 = VERTEX_POINT ( 'NONE', #53647 ) ;
#21021 = ADVANCED_FACE ( 'NONE', ( #113199 ), #31981, .T. ) ;
#21023 = CARTESIAN_POINT ( 'NONE',  ( -0.8500000000000390576, 2.500000000000000000, -2.065063509461102065 ) ) ;
#21024 = CARTESIAN_POINT ( 'NONE',  ( 8.549999999999924327, 12.50000000000000000, 1.753560074763284016 ) ) ;
#21025 = EDGE_CURVE ( 'NONE', #73329, #97417, #59063, .T. ) ;
#21026 = DIRECTION ( 'NONE',  ( 0.000000000000000000, 0.000000000000000000, 1.000000000000000000 ) ) ;
#21027 = ADVANCED_FACE ( 'NONE', ( #83754 ), #125943, .T. ) ;
#21028 = EDGE_CURVE ( 'NONE', #67896, #36385, #79981, .T. ) ;
#21029 = CARTESIAN_POINT ( 'NONE',  ( -3.950000000000028155, 12.50000000000000000, -6.841600689897077814 ) ) ;
#21030 = CARTESIAN_POINT ( 'NONE',  ( 5.849999999999931255, 12.50000000000000000, 2.922977105672686982 ) ) ;
#21031 = ORIENTED_EDGE ( 'NONE', *, *, #29296, .T. ) ;
#21032 = VERTEX_POINT ( 'NONE', #34677 ) ;
#21033 = ORIENTED_EDGE ( 'NONE', *, *, #56808, .T. ) ;
#21034 = CONICAL_SURFACE ( 'NONE', #119318, 0.1000000000000000472, 0.003490658503988666988 ) ;
#21035 = CARTESIAN_POINT ( 'NONE',  ( -1.450000000000035039, 2.500000000000000000, -2.511473670974877948 ) ) ;
#21036 = CIRCLE ( 'NONE', #60756, 0.09999999999999982514 ) ;
#21037 = EDGE_CURVE ( 'NONE', #48425, #585, #4749, .T. ) ;
#21038 = ORIENTED_EDGE ( 'NONE', *, *, #31419, .F. ) ;
#21039 = CARTESIAN_POINT ( 'NONE',  ( 17.50000000000000000, -2.481874935395255832, 3.264429721014085573 ) ) ;
#21040 = DIRECTION ( 'NONE',  ( 0.000000000000000000, 0.000000000000000000, -1.000000000000000000 ) ) ;
#21041 = EDGE_LOOP ( 'NONE', ( #125393, #78779 ) ) ;
#21042 = DIRECTION ( 'NONE',  ( 0.000000000000000000, 0.000000000000000000, 1.000000000000000000 ) ) ;
#21043 = DIRECTION ( 'NONE',  ( 0.000000000000000000, 1.000000000000000000, 0.000000000000000000 ) ) ;
#21044 = CARTESIAN_POINT ( 'NONE',  ( -9.350000000000006750, 12.50000000000000000, -2.576566944158915184 ) ) ;
#21045 = DIRECTION ( 'NONE',  ( 0.000000000000000000, 1.000000000000000000, 0.000000000000000000 ) ) ;
#21046 = DIRECTION ( 'NONE',  ( -0.000000000000000000, -1.000000000000000000, -0.000000000000000000 ) ) ;
#21047 = ORIENTED_EDGE ( 'NONE', *, *, #38361, .T. ) ;
#21048 = DIRECTION ( 'NONE',  ( -4.274815082592931898E-19, -0.9999939076577903929, -0.003490651415223739937 ) ) ;
#21049 = CARTESIAN_POINT ( 'NONE',  ( 4.549999999999937650, 12.50000000000000000, 2.099970236277060032 ) ) ;
#21050 = DIRECTION ( 'NONE',  ( 0.000000000000000000, 1.000000000000000000, 0.000000000000000000 ) ) ;
#21051 = CARTESIAN_POINT ( 'NONE',  ( -9.400000000000007461, 2.500000000000000000, 4.083716857408420609 ) ) ;
#21052 = VERTEX_POINT ( 'NONE', #116418 ) ;
#21053 = VERTEX_POINT ( 'NONE', #35311 ) ;
#21054 = EDGE_CURVE ( 'NONE', #118622, #71534, #26129, .T. ) ;
#21055 = PLANE ( 'NONE',  #119115 ) ;
#21056 = FACE_OUTER_BOUND ( 'NONE', #67370, .T. ) ;
#21057 = DIRECTION ( 'NONE',  ( 0.000000000000000000, 0.000000000000000000, 1.000000000000000000 ) ) ;
#21058 = EDGE_CURVE ( 'NONE', #2492, #58787, #109220, .T. ) ;
#21059 = ORIENTED_EDGE ( 'NONE', *, *, #55612, .F. ) ;
#21060 = VECTOR ( 'NONE', #85729, 1000.000000000000000 ) ;
#21061 = CARTESIAN_POINT ( 'NONE',  ( -3.350000000000028955, 2.500000000000000000, 7.188010851410848723 ) ) ;
#21062 = AXIS2_PLACEMENT_3D ( 'NONE', #118881, #31163, #59990 ) ;
#21063 = ADVANCED_FACE ( 'NONE', ( #115115 ), #100897, .T. ) ;
#21064 = CARTESIAN_POINT ( 'NONE',  ( -11.44999999999999751, 12.50000000000000000, 2.511473670974873507 ) ) ;
#21065 = ORIENTED_EDGE ( 'NONE', *, *, #53088, .F. ) ;
#21066 = LINE ( 'NONE', #100913, #126389 ) ;
#21067 = ADVANCED_FACE ( 'NONE', ( #66675 ), #19332, .T. ) ;
#21068 = ORIENTED_EDGE ( 'NONE', *, *, #96438, .F. ) ;
#21069 = CIRCLE ( 'NONE', #6376, 0.1000000000000002554 ) ;
#21070 = CARTESIAN_POINT ( 'NONE',  ( 11.69999999999990870, 12.50000000000000000, -4.330127018922201643 ) ) ;
#21071 = EDGE_CURVE ( 'NONE', #49367, #114625, #106605, .T. ) ;
#21072 = AXIS2_PLACEMENT_3D ( 'NONE', #41310, #111293, #121137 ) ;
#21073 = EDGE_CURVE ( 'NONE', #83615, #89926, #52792, .T. ) ;
#21074 = ADVANCED_FACE ( 'NONE', ( #45774 ), #54925, .T. ) ;
#21075 = ORIENTED_EDGE ( 'NONE', *, *, #45619, .F. ) ;
#21076 = DIRECTION ( 'NONE',  ( 0.000000000000000000, 1.000000000000000000, 0.000000000000000000 ) ) ;
#21077 = FACE_OUTER_BOUND ( 'NONE', #112767, .T. ) ;
#21078 = ORIENTED_EDGE ( 'NONE', *, *, #100341, .T. ) ;
#21079 = EDGE_LOOP ( 'NONE', ( #105650, #86901, #51284, #9718, #111532, #35065, #25327 ) ) ;
#21080 = DIRECTION ( 'NONE',  ( 0.000000000000000000, 0.000000000000000000, -1.000000000000000000 ) ) ;
#21081 = DIRECTION ( 'NONE',  ( 0.000000000000000000, 1.000000000000000000, 0.000000000000000000 ) ) ;
#21082 = ORIENTED_EDGE ( 'NONE', *, *, #40699, .F. ) ;
#21083 = ADVANCED_FACE ( 'NONE', ( #107254 ), #57524, .T. ) ;
#21085 = CARTESIAN_POINT ( 'NONE',  ( -4.251297162942325111E-14, 2.500000000000000000, -3.737306695894649700 ) ) ;
#21084 = CIRCLE ( 'NONE', #110956, 0.06509327318403745899 ) ;
#21086 = CARTESIAN_POINT ( 'NONE',  ( 186.1510416670080588, 4.367472073101518859, -7.564683531249999149 ) ) ;
#21087 = VECTOR ( 'NONE', #20109, 1000.000000000000000 ) ;
#21088 = CARTESIAN_POINT ( 'NONE',  ( 11.89999999999990798, 2.500000000000000000, -3.883716857408426648 ) ) ;
#21089 = CARTESIAN_POINT ( 'NONE',  ( 9.799999999999917222, 2.500000000000000000, 0.2464101615137735679 ) ) ;
#21090 = DIRECTION ( 'NONE',  ( 0.000000000000000000, 0.000000000000000000, 1.000000000000000000 ) ) ;
#21091 = PLANE ( 'NONE',  #24325 ) ;
#21092 = DIRECTION ( 'NONE',  ( 0.000000000000000000, 1.000000000000000000, 0.000000000000000000 ) ) ;
#21093 = CIRCLE ( 'NONE', #46140, 0.06509327318403745899 ) ;
#21094 = EDGE_LOOP ( 'NONE', ( #110494, #12121, #112401, #25392 ) ) ;
#21095 = ORIENTED_EDGE ( 'NONE', *, *, #116890, .F. ) ;
#21096 = CARTESIAN_POINT ( 'NONE',  ( 3.949999999999941558, 12.50000000000000000, -1.818653347947326138 ) ) ;
#21097 = EDGE_LOOP ( 'NONE', ( #95419, #33687, #122643, #2681 ) ) ;
#21098 = AXIS2_PLACEMENT_3D ( 'NONE', #61185, #81473, #33658 ) ;
#21099 = CARTESIAN_POINT ( 'NONE',  ( 0.6499999999999543920, 2.500000000000000000, 6.841600689897072485 ) ) ;
#21100 = FACE_OUTER_BOUND ( 'NONE', #76360, .T. ) ;
#21101 = DIRECTION ( 'NONE',  ( 0.000000000000000000, 0.000000000000000000, -1.000000000000000000 ) ) ;
#21103 = ORIENTED_EDGE ( 'NONE', *, *, #83127, .F. ) ;
#21102 = ORIENTED_EDGE ( 'NONE', *, *, #71190, .F. ) ;
#21104 = FACE_BOUND ( 'NONE', #82961, .T. ) ;
#21105 = ORIENTED_EDGE ( 'NONE', *, *, #91309, .T. ) ;
#21106 = ADVANCED_FACE ( 'NONE', ( #46391 ), #71673, .T. ) ;
#21107 = DIRECTION ( 'NONE',  ( 0.000000000000000000, 0.000000000000000000, 1.000000000000000000 ) ) ;
#21108 = LINE ( 'NONE', #61034, #58439 ) ;
#21109 = CARTESIAN_POINT ( 'NONE',  ( 1.899999999999951283, 2.500000000000000000, -3.883716857408426648 ) ) ;
#21110 = CARTESIAN_POINT ( 'NONE',  ( -1.850000000000033396, 12.50000000000000000, -1.818653347947325916 ) ) ;
#21111 = FACE_OUTER_BOUND ( 'NONE', #105457, .T. ) ;
#21112 = CARTESIAN_POINT ( 'NONE',  ( 14.99999999999992895, 2.500000000000000000, 0.09999999999999772959 ) ) ;
#21113 = DIRECTION ( 'NONE',  ( -0.000000000000000000, 1.000000000000000000, -0.000000000000000000 ) ) ;
#21114 = LINE ( 'NONE', #834, #83338 ) ;
#21115 = DIRECTION ( 'NONE',  ( 0.000000000000000000, 1.000000000000000000, 0.000000000000000000 ) ) ;
#21116 = CARTESIAN_POINT ( 'NONE',  ( -4.150000000000028777, 2.500000000000000000, -5.702370205355749455 ) ) ;
#21117 = DIRECTION ( 'NONE',  ( 0.000000000000000000, -0.9999939076577903929, 0.003490651415223739937 ) ) ;
#21118 = ORIENTED_EDGE ( 'NONE', *, *, #26445, .F. ) ;
#21119 = EDGE_LOOP ( 'NONE', ( #94408, #27801, #79848, #41177 ) ) ;
#21120 = ADVANCED_FACE ( 'NONE', ( #105969 ), #15307, .T. ) ;
#21121 = ORIENTED_EDGE ( 'NONE', *, *, #99642, .T. ) ;
#21122 = ORIENTED_EDGE ( 'NONE', *, *, #110702, .T. ) ;
#21123 = DIRECTION ( 'NONE',  ( -0.000000000000000000, -1.000000000000000000, -0.000000000000000000 ) ) ;
#21124 = AXIS2_PLACEMENT_3D ( 'NONE', #29241, #77666, #37756 ) ;
#21125 = CARTESIAN_POINT ( 'NONE',  ( 6.249999999999932498, 2.500000000000000000, 5.802370205355744659 ) ) ;
#21126 = VECTOR ( 'NONE', #91204, 1000.000000000000000 ) ;
#21127 = VECTOR ( 'NONE', #68321, 1000.000000000000000 ) ;
#21129 = ORIENTED_EDGE ( 'NONE', *, *, #39254, .T. ) ;
#21128 = ORIENTED_EDGE ( 'NONE', *, *, #13931, .T. ) ;
#21130 = ORIENTED_EDGE ( 'NONE', *, *, #79562, .F. ) ;
#21131 = DIRECTION ( 'NONE',  ( 0.000000000000000000, 0.000000000000000000, -1.000000000000000000 ) ) ;
#21132 = CIRCLE ( 'NONE', #37852, 0.1000000000000002554 ) ;
#21133 = DIRECTION ( 'NONE',  ( 0.000000000000000000, 1.000000000000000000, 0.000000000000000000 ) ) ;
#21134 = FILL_AREA_STYLE_COLOUR ( '', #104099 ) ;
#21135 = DIRECTION ( 'NONE',  ( 0.000000000000000000, 0.000000000000000000, 1.000000000000000000 ) ) ;
#21136 = LINE ( 'NONE', #11960, #105691 ) ;
#21137 = FACE_OUTER_BOUND ( 'NONE', #70487, .T. ) ;
#21138 = AXIS2_PLACEMENT_3D ( 'NONE', #10200, #40317, #80235 ) ;
#21139 = CARTESIAN_POINT ( 'NONE',  ( 6.899999999999928413, 12.50000000000000000, -4.676537180435977881 ) ) ;
#21140 = EDGE_CURVE ( 'NONE', #86566, #7480, #5175, .T. ) ;
#21141 = EDGE_LOOP ( 'NONE', ( #107816, #10787, #91477, #13781 ) ) ;
#21142 = LINE ( 'NONE', #123224, #91447 ) ;
#21143 = VERTEX_POINT ( 'NONE', #25454 ) ;
#21144 = ORIENTED_EDGE ( 'NONE', *, *, #101586, .T. ) ;
#21145 = ORIENTED_EDGE ( 'NONE', *, *, #117072, .F. ) ;
#21146 = CARTESIAN_POINT ( 'NONE',  ( 10.79999999999991012, 2.500000000000000000, 4.230127018922196669 ) ) ;
#21147 = VERTEX_POINT ( 'NONE', #117053 ) ;
#21148 = ORIENTED_EDGE ( 'NONE', *, *, #5521, .T. ) ;
#21149 = ORIENTED_EDGE ( 'NONE', *, *, #112109, .T. ) ;
#21150 = DIRECTION ( 'NONE',  ( 0.000000000000000000, 0.000000000000000000, 1.000000000000000000 ) ) ;
#21151 = CIRCLE ( 'NONE', #96355, 7.700000000000000178 ) ;
#21152 = DIRECTION ( 'NONE',  ( 0.000000000000000000, 0.000000000000000000, -1.000000000000000000 ) ) ;
#21153 = PLANE ( 'NONE',  #14384 ) ;
#21154 = CARTESIAN_POINT ( 'NONE',  ( 15.19999999999989093, 2.500000000000000000, 0.3464101615137735735 ) ) ;
#21155 = CARTESIAN_POINT ( 'NONE',  ( 9.349999999999919709, 12.50000000000000000, 2.446380397790835826 ) ) ;
#21156 = DIRECTION ( 'NONE',  ( 0.000000000000000000, 0.000000000000000000, 1.000000000000000000 ) ) ;
#21157 = FACE_OUTER_BOUND ( 'NONE', #60080, .T. ) ;
#21158 = AXIS2_PLACEMENT_3D ( 'NONE', #25513, #83801, #85089 ) ;
#21159 = CONICAL_SURFACE ( 'NONE', #77505, 0.1000000000000002554, 0.003490658503988666988 ) ;
#21160 = ORIENTED_EDGE ( 'NONE', *, *, #126738, .T. ) ;
#21161 = DIRECTION ( 'NONE',  ( -0.000000000000000000, 1.000000000000000000, -0.000000000000000000 ) ) ;
#21162 = EDGE_CURVE ( 'NONE', #79172, #108104, #645, .T. ) ;
#21163 = VERTEX_POINT ( 'NONE', #105330 ) ;
#21164 = DIRECTION ( 'NONE',  ( -0.000000000000000000, 1.000000000000000000, -0.000000000000000000 ) ) ;
#21165 = PLANE ( 'NONE',  #37767 ) ;
#21166 = ORIENTED_EDGE ( 'NONE', *, *, #116959, .F. ) ;
#21167 = LINE ( 'NONE', #10682, #2870 ) ;
#21168 = DIRECTION ( 'NONE',  ( -0.000000000000000000, 1.000000000000000000, -0.000000000000000000 ) ) ;
#21169 = ORIENTED_EDGE ( 'NONE', *, *, #111178, .T. ) ;
#21170 = VECTOR ( 'NONE', #75938, 1000.000000000000000 ) ;
#21171 = EDGE_CURVE ( 'NONE', #1500, #112120, #27386, .T. ) ;
#21172 = AXIS2_PLACEMENT_3D ( 'NONE', #121770, #32137, #53688 ) ;
#21173 = CARTESIAN_POINT ( 'NONE',  ( 0.4499999999999552136, 12.50000000000000000, 6.495190528383297135 ) ) ;
#21174 = ORIENTED_EDGE ( 'NONE', *, *, #16821, .T. ) ;
#21175 = ADVANCED_FACE ( 'NONE', ( #6440 ), #63364, .T. ) ;
#21177 = VERTEX_POINT ( 'NONE', #78468 ) ;
#21176 = EDGE_CURVE ( 'NONE', #44930, #81872, #73815, .T. ) ;
#21178 = DIRECTION ( 'NONE',  ( -4.274815082592931898E-19, -0.9999939076577903929, -0.003490651415223739937 ) ) ;
#21179 = DIRECTION ( 'NONE',  ( -0.000000000000000000, 1.000000000000000000, -0.000000000000000000 ) ) ;
#21180 = EDGE_CURVE ( 'NONE', #15629, #109700, #20817, .T. ) ;
#21181 = LINE ( 'NONE', #61109, #23019 ) ;
#21182 = EDGE_CURVE ( 'NONE', #7665, #12607, #88232, .T. ) ;
#21183 = CARTESIAN_POINT ( 'NONE',  ( 7.499999999999927169, 12.50000000000000000, 3.702399969078682407 ) ) ;
#21184 = AXIS2_PLACEMENT_3D ( 'NONE', #100443, #99805, #12055 ) ;
#21185 = CARTESIAN_POINT ( 'NONE',  ( -13.74999999999998757, 12.50000000000000000, -2.857883832488651521 ) ) ;
#21186 = ORIENTED_EDGE ( 'NONE', *, *, #92232, .T. ) ;
#21187 = CARTESIAN_POINT ( 'NONE',  ( 11.84999999999990372, 2.500000000000000000, 1.818653347947321475 ) ) ;
#21188 = ADVANCED_FACE ( 'NONE', ( #98078 ), #27841, .T. ) ;
#21189 = AXIS2_PLACEMENT_3D ( 'NONE', #13492, #53448, #81599 ) ;
#21190 = ORIENTED_EDGE ( 'NONE', *, *, #113301, .T. ) ;
#21191 = EDGE_CURVE ( 'NONE', #6403, #74808, #65399, .T. ) ;
#21192 = PLANE ( 'NONE',  #121789 ) ;
#21193 = LINE ( 'NONE', #60500, #104438 ) ;
#21194 = EDGE_CURVE ( 'NONE', #93259, #26633, #39192, .T. ) ;
#21195 = CONICAL_SURFACE ( 'NONE', #50524, 0.1000000000000002554, 0.003490658503988666988 ) ;
#21196 = CIRCLE ( 'NONE', #50443, 0.1000000000000002554 ) ;
#21197 = ADVANCED_BREP_SHAPE_REPRESENTATION ( '', ( #100344, #108296 ), #1678 ) ;
#21198 = CARTESIAN_POINT ( 'NONE',  ( 0.1999999999999567124, 2.500000000000000000, -3.983716857408426293 ) ) ;
#21199 = DIRECTION ( 'NONE',  ( -0.000000000000000000, -1.000000000000000000, -0.000000000000000000 ) ) ;
#21200 = DIRECTION ( 'NONE',  ( 0.000000000000000000, 1.000000000000000000, 0.000000000000000000 ) ) ;
#21201 = FACE_OUTER_BOUND ( 'NONE', #18361, .T. ) ;
#21202 = DIRECTION ( 'NONE',  ( 0.000000000000000000, 0.000000000000000000, 1.000000000000000000 ) ) ;
#21203 = VERTEX_POINT ( 'NONE', #119012 ) ;
#21204 = DIRECTION ( 'NONE',  ( 0.000000000000000000, 0.000000000000000000, 1.000000000000000000 ) ) ;
#21205 = CARTESIAN_POINT ( 'NONE',  ( 8.149999999999923972, 2.500000000000000000, 1.818653347947321475 ) ) ;
#21206 = CARTESIAN_POINT ( 'NONE',  ( 2.499999999999983569, 2.500000000000000000, 0.09999999999999772959 ) ) ;
#21207 = VERTEX_POINT ( 'NONE', #120308 ) ;
#21208 = DIRECTION ( 'NONE',  ( 0.000000000000000000, 0.000000000000000000, -1.000000000000000000 ) ) ;
#21209 = ORIENTED_EDGE ( 'NONE', *, *, #40731, .T. ) ;
#21210 = ORIENTED_EDGE ( 'NONE', *, *, #55909, .T. ) ;
#21211 = DIRECTION ( 'NONE',  ( 0.000000000000000000, 0.000000000000000000, 1.000000000000000000 ) ) ;
#21212 = CONICAL_SURFACE ( 'NONE', #115182, 0.1000000000000002554, 0.003490658503988666988 ) ;
#21213 = CIRCLE ( 'NONE', #71290, 0.1000000000000002554 ) ;
#21214 = CIRCLE ( 'NONE', #44291, 0.06509327318403745899 ) ;
#21215 = ORIENTED_EDGE ( 'NONE', *, *, #84329, .F. ) ;
#21216 = LINE ( 'NONE', #42831, #60228 ) ;
#21217 = DIRECTION ( 'NONE',  ( 0.000000000000000000, 0.000000000000000000, -1.000000000000000000 ) ) ;
#21218 = CARTESIAN_POINT ( 'NONE',  ( 3.549999999999943867, 2.500000000000000000, -6.048780366869526581 ) ) ;
#21219 = ORIENTED_EDGE ( 'NONE', *, *, #31131, .F. ) ;
#21221 = CARTESIAN_POINT ( 'NONE',  ( -11.05000000000000071, 12.50000000000000000, 2.511473670974873507 ) ) ;
#21220 = VECTOR ( 'NONE', #73860, 1000.000000000000000 ) ;
#21222 = AXIS2_PLACEMENT_3D ( 'NONE', #20809, #60737, #120933 ) ;
#21223 = CARTESIAN_POINT ( 'NONE',  ( -5.600000000000020073, 12.50000000000000000, 4.676537180435972552 ) ) ;
#21224 = CARTESIAN_POINT ( 'NONE',  ( 11.84999999999990727, 2.500000000000000000, -1.718653347947326049 ) ) ;
#21225 = EDGE_CURVE ( 'NONE', #124539, #105724, #29360, .T. ) ;
#21226 = ORIENTED_EDGE ( 'NONE', *, *, #51644, .T. ) ;
#21227 = EDGE_CURVE ( 'NONE', #83483, #111264, #94745, .T. ) ;
#21228 = ORIENTED_EDGE ( 'NONE', *, *, #100647, .T. ) ;
#21229 = EDGE_CURVE ( 'NONE', #73117, #123848, #38549, .T. ) ;
#21230 = ORIENTED_EDGE ( 'NONE', *, *, #25929, .F. ) ;
#21231 = FACE_OUTER_BOUND ( 'NONE', #81791, .T. ) ;
#21232 = DIRECTION ( 'NONE',  ( 0.000000000000000000, 0.000000000000000000, -1.000000000000000000 ) ) ;
#21233 = DIRECTION ( 'NONE',  ( -4.274815082592931898E-19, -0.9999939076577903929, -0.003490651415223739937 ) ) ;
#21234 = FACE_BOUND ( 'NONE', #16402, .T. ) ;
#21235 = EDGE_LOOP ( 'NONE', ( #57356, #45730, #57579, #42063 ) ) ;
#21236 = DIRECTION ( 'NONE',  ( -0.000000000000000000, 1.000000000000000000, -0.000000000000000000 ) ) ;
#21237 = FACE_OUTER_BOUND ( 'NONE', #5532, .T. ) ;
#21238 = ORIENTED_EDGE ( 'NONE', *, *, #124652, .F. ) ;
#21239 = ADVANCED_FACE ( 'NONE', ( #98710 ), #48789, .T. ) ;
#21240 = DIRECTION ( 'NONE',  ( 0.000000000000000000, 0.000000000000000000, -1.000000000000000000 ) ) ;
#21241 = CARTESIAN_POINT ( 'NONE',  ( 4.399999999999940847, 2.500000000000000000, -4.083716857408426826 ) ) ;
#21242 = CARTESIAN_POINT ( 'NONE',  ( 7.099999999999925926, 2.500000000000000000, 0.5928203230275495006 ) ) ;
#21243 = FACE_OUTER_BOUND ( 'NONE', #50703, .T. ) ;
#21244 = CARTESIAN_POINT ( 'NONE',  ( 133.2169897921533845, 2.500000000000000000, -2.337293474289257933 ) ) ;
#21245 = DIRECTION ( 'NONE',  ( 0.000000000000000000, 0.000000000000000000, -1.000000000000000000 ) ) ;
#21246 = DIRECTION ( 'NONE',  ( -0.000000000000000000, 1.000000000000000000, -0.000000000000000000 ) ) ;
#21247 = CIRCLE ( 'NONE', #42191, 0.06509327318403745899 ) ;
#21248 = CIRCLE ( 'NONE', #6543, 0.06509327318403743123 ) ;
#21249 = EDGE_LOOP ( 'NONE', ( #25721, #96469, #19698, #27920 ) ) ;
#21250 = VERTEX_POINT ( 'NONE', #109174 ) ;
#21251 = ORIENTED_EDGE ( 'NONE', *, *, #60918, .T. ) ;
#21252 = ORIENTED_EDGE ( 'NONE', *, *, #26654, .F. ) ;
#21253 = DIRECTION ( 'NONE',  ( 0.000000000000000000, -0.9999939076577903929, 0.003490651415223739937 ) ) ;
#21254 = CARTESIAN_POINT ( 'NONE',  ( 11.44999999999990692, 2.500000000000000000, -6.941600689897078347 ) ) ;
#21255 = EDGE_LOOP ( 'NONE', ( #114836, #129556 ) ) ;
#21256 = FACE_BOUND ( 'NONE', #58576, .T. ) ;
#21257 = EDGE_CURVE ( 'NONE', #14153, #63242, #113529, .T. ) ;
#21258 = CONICAL_SURFACE ( 'NONE', #29580, 0.09999999999999999167, 0.003490658503988666988 ) ;
#21259 = CARTESIAN_POINT ( 'NONE',  ( 1.699999999999951994, 12.50000000000000000, -2.276824562219559311E-15 ) ) ;
#21260 = CONICAL_SURFACE ( 'NONE', #46296, 0.1000000000000000056, 0.003490658503988666988 ) ;
#21261 = DIRECTION ( 'NONE',  ( 0.000000000000000000, -0.9999939076577903929, 0.003490651415223739937 ) ) ;
#21262 = CIRCLE ( 'NONE', #77687, 0.06509327318403745899 ) ;
#21263 = DIRECTION ( 'NONE',  ( -4.274815082592931898E-19, -0.9999939076577903929, -0.003490651415223739937 ) ) ;
#21264 = DIRECTION ( 'NONE',  ( 0.000000000000000000, 0.000000000000000000, 1.000000000000000000 ) ) ;
#21265 = DIRECTION ( 'NONE',  ( -0.000000000000000000, -1.000000000000000000, -0.000000000000000000 ) ) ;
#21266 = CARTESIAN_POINT ( 'NONE',  ( 6.049999999999934097, 2.500000000000000000, -6.048780366869526581 ) ) ;
#21267 = DIRECTION ( 'NONE',  ( 0.000000000000000000, 1.000000000000000000, 0.000000000000000000 ) ) ;
#21268 = CARTESIAN_POINT ( 'NONE',  ( -3.100000000000028955, 12.50000000000000000, 3.983716857408420964 ) ) ;
#21269 = ORIENTED_EDGE ( 'NONE', *, *, #16029, .T. ) ;
#21270 = CIRCLE ( 'NONE', #60980, 0.1000000000000002554 ) ;
#21271 = EDGE_LOOP ( 'NONE', ( #86031, #70242 ) ) ;
#21272 = PRODUCT_DEFINITION_FORMATION_WITH_SPECIFIED_SOURCE ( 'ANY', '', #72268, .NOT_KNOWN. ) ;
#21273 = CONICAL_SURFACE ( 'NONE', #35948, 0.1000000000000000472, 0.003490658503988666988 ) ;
#21274 = VERTEX_POINT ( 'NONE', #79105 ) ;
#21275 = EDGE_LOOP ( 'NONE', ( #71038, #99531 ) ) ;
#21276 = EDGE_CURVE ( 'NONE', #101165, #72896, #57088, .T. ) ;
#21277 = ORIENTED_EDGE ( 'NONE', *, *, #114808, .T. ) ;
#21278 = EDGE_LOOP ( 'NONE', ( #95580, #91044, #118137, #24867 ) ) ;
#21279 = AXIS2_PLACEMENT_3D ( 'NONE', #88140, #90086, #47613 ) ;
#21280 = CONICAL_SURFACE ( 'NONE', #75643, 0.1000000000000002554, 0.003490658503988666988 ) ;
#21281 = CARTESIAN_POINT ( 'NONE',  ( -3.950000000000028155, 2.500000000000000000, -6.841600689897077814 ) ) ;
#21282 = VERTEX_POINT ( 'NONE', #9045 ) ;
#21283 = CONICAL_SURFACE ( 'NONE', #38007, 0.09999999999999982514, 0.003490658503988666988 ) ;
#21284 = CARTESIAN_POINT ( 'NONE',  ( 17.37282530749033427, 0.4689596142739222984, 5.357821376857530460 ) ) ;
#21285 = AXIS2_PLACEMENT_3D ( 'NONE', #115919, #36734, #24962 ) ;
#21286 = CARTESIAN_POINT ( 'NONE',  ( 16.56576425164984201, -2.499999999999999556, 6.084390597446047266 ) ) ;
#21287 = FACE_OUTER_BOUND ( 'NONE', #115482, .T. ) ;
#21288 = DIRECTION ( 'NONE',  ( 0.000000000000000000, 0.000000000000000000, 1.000000000000000000 ) ) ;
#21289 = ADVANCED_FACE ( 'NONE', ( #58180 ), #52901, .T. ) ;
#21290 = ORIENTED_EDGE ( 'NONE', *, *, #30432, .T. ) ;
#21291 = DIRECTION ( 'NONE',  ( -1.000000000000000000, -0.000000000000000000, -0.000000000000000000 ) ) ;
#21292 = ORIENTED_EDGE ( 'NONE', *, *, #14346, .T. ) ;
#21293 = ORIENTED_EDGE ( 'NONE', *, *, #46314, .F. ) ;
#21294 = LINE ( 'NONE', #71692, #119981 ) ;
#21295 = FACE_OUTER_BOUND ( 'NONE', #101056, .T. ) ;
#21297 = ADVANCED_FACE ( 'NONE', ( #48339 ), #2697, .T. ) ;
#21296 = DIRECTION ( 'NONE',  ( -0.000000000000000000, -1.000000000000000000, -0.000000000000000000 ) ) ;
#21298 = ORIENTED_EDGE ( 'NONE', *, *, #113743, .T. ) ;
#21299 = ORIENTED_EDGE ( 'NONE', *, *, #25060, .F. ) ;
#21300 = DIRECTION ( 'NONE',  ( 0.000000000000000000, 1.000000000000000000, 0.000000000000000000 ) ) ;
#21301 = CARTESIAN_POINT ( 'NONE',  ( 4.149999999999938183, 12.50000000000000000, 2.165063509461097713 ) ) ;
#21302 = DIRECTION ( 'NONE',  ( -0.000000000000000000, -1.000000000000000000, -0.000000000000000000 ) ) ;
#21304 = FACE_OUTER_BOUND ( 'NONE', #46068, .T. ) ;
#21303 = AXIS2_PLACEMENT_3D ( 'NONE', #110581, #20916, #51039 ) ;
#21305 = VERTEX_POINT ( 'NONE', #89550 ) ;
#21306 = AXIS2_PLACEMENT_3D ( 'NONE', #120012, #40829, #31012 ) ;
#21307 = CARTESIAN_POINT ( 'NONE',  ( -13.14999999999999147, 2.500000000000000000, -2.611473670974875372 ) ) ;
#21308 = VERTEX_POINT ( 'NONE', #99384 ) ;
#21309 = CARTESIAN_POINT ( 'NONE',  ( 8.299999999999922551, 2.500000000000000000, -4.430127018922202176 ) ) ;
#21310 = VERTEX_POINT ( 'NONE', #9706 ) ;
#21311 = DIRECTION ( 'NONE',  ( 0.000000000000000000, 0.000000000000000000, -1.000000000000000000 ) ) ;
#21313 = EDGE_CURVE ( 'NONE', #62304, #127558, #8960, .T. ) ;
#21312 = AXIS2_PLACEMENT_3D ( 'NONE', #107430, #112904, #86494 ) ;
#21314 = CARTESIAN_POINT ( 'NONE',  ( 21.23528140090950345, -2.699413673072312392, 2.293764360948889802 ) ) ;
#21315 = CARTESIAN_POINT ( 'NONE',  ( -10.65000000000000391, 2.500000000000000000, -1.918653347947322230 ) ) ;
#21316 = AXIS2_PLACEMENT_3D ( 'NONE', #107732, #72970, #71674 ) ;
#21317 = CIRCLE ( 'NONE', #79812, 0.06509327318403745899 ) ;
#21318 = DIRECTION ( 'NONE',  ( 0.000000000000000000, 0.000000000000000000, 1.000000000000000000 ) ) ;
#21319 = ORIENTED_EDGE ( 'NONE', *, *, #58873, .T. ) ;
#21320 = VECTOR ( 'NONE', #14155, 1000.000000000000000 ) ;
#21321 = ADVANCED_FACE ( 'NONE', ( #20168 ), #60116, .T. ) ;
#21322 = DIRECTION ( 'NONE',  ( 0.000000000000000000, -0.9999939076577903929, 0.003490651415223739937 ) ) ;
#21323 = FACE_OUTER_BOUND ( 'NONE', #80641, .T. ) ;
#21324 = VERTEX_POINT ( 'NONE', #80390 ) ;
#21325 = VERTEX_POINT ( 'NONE', #30649 ) ;
#21326 = EDGE_CURVE ( 'NONE', #123620, #65442, #4849, .T. ) ;
#21328 = EDGE_LOOP ( 'NONE', ( #84882, #5881, #83242, #7708 ) ) ;
#21327 = EDGE_CURVE ( 'NONE', #32461, #45043, #90540, .T. ) ;
#21329 = DIRECTION ( 'NONE',  ( -4.274815082592931898E-19, -0.9999939076577903929, -0.003490651415223739937 ) ) ;
#21330 = DIRECTION ( 'NONE',  ( 0.000000000000000000, 0.000000000000000000, -1.000000000000000000 ) ) ;
#21331 = DIRECTION ( 'NONE',  ( 0.000000000000000000, 1.000000000000000000, 0.000000000000000000 ) ) ;
#21332 = EDGE_CURVE ( 'NONE', #70125, #92609, #92605, .T. ) ;
#21333 = CARTESIAN_POINT ( 'NONE',  ( -9.550000000000006040, 12.50000000000000000, 2.099970236277060032 ) ) ;
#21334 = ADVANCED_FACE ( 'NONE', ( #63311 ), #67536, .T. ) ;
#21335 = DIRECTION ( 'NONE',  ( 0.000000000000000000, 1.000000000000000000, 0.000000000000000000 ) ) ;
#21336 = CARTESIAN_POINT ( 'NONE',  ( -1.850000000000033396, 2.500000000000000000, -2.411473670974877859 ) ) ;
#21337 = DIRECTION ( 'NONE',  ( -0.000000000000000000, 1.000000000000000000, -0.000000000000000000 ) ) ;
#21338 = CARTESIAN_POINT ( 'NONE',  ( 11.64999999999990798, 2.500000000000000000, -2.957883832488653830 ) ) ;
#21339 = LINE ( 'NONE', #34414, #77726 ) ;
#21340 = ADVANCED_FACE ( 'NONE', ( #62685 ), #117707, .T. ) ;
#21341 = EDGE_CURVE ( 'NONE', #44142, #107907, #59169, .T. ) ;
#21342 = EDGE_CURVE ( 'NONE', #118459, #116018, #128209, .T. ) ;
#21344 = EDGE_CURVE ( 'NONE', #114635, #80732, #78023, .T. ) ;
#21343 = AXIS2_PLACEMENT_3D ( 'NONE', #75413, #6022, #6639 ) ;
#21345 = ADVANCED_FACE ( 'NONE', ( #33849 ), #42445, .T. ) ;
#21346 = EDGE_LOOP ( 'NONE', ( #125766, #25994 ) ) ;
#21347 = DIRECTION ( 'NONE',  ( 0.000000000000000000, 1.000000000000000000, 0.000000000000000000 ) ) ;
#21348 = ADVANCED_FACE ( 'NONE', ( #42396 ), #93422, .T. ) ;
#21349 = DIRECTION ( 'NONE',  ( 1.000000000000000000, 0.000000000000000000, 8.881784197001235560E-16 ) ) ;
#21350 = DIRECTION ( 'NONE',  ( -4.274815082592931898E-19, -0.9999939076577903929, -0.003490651415223739937 ) ) ;
#21351 = DIRECTION ( 'NONE',  ( 0.000000000000000000, 0.000000000000000000, -1.000000000000000000 ) ) ;
#21353 = EDGE_CURVE ( 'NONE', #115594, #10073, #13153, .T. ) ;
#21352 = CIRCLE ( 'NONE', #71527, 0.1000000000000002554 ) ;
#21354 = AXIS2_PLACEMENT_3D ( 'NONE', #123372, #53998, #113556 ) ;
#21355 = ORIENTED_EDGE ( 'NONE', *, *, #81486, .F. ) ;
#21356 = LINE ( 'NONE', #31200, #109426 ) ;
#21357 = VECTOR ( 'NONE', #55794, 1000.000000000000000 ) ;
#21358 = CONICAL_SURFACE ( 'NONE', #23406, 0.1000000000000002554, 0.003490658503988666988 ) ;
#21359 = CARTESIAN_POINT ( 'NONE',  ( 1.249999999999953815, 12.50000000000000000, 1.472243186433545459 ) ) ;
#21361 = ORIENTED_EDGE ( 'NONE', *, *, #66682, .F. ) ;
#21360 = LINE ( 'NONE', #41675, #25374 ) ;
#21362 = CONICAL_SURFACE ( 'NONE', #52751, 0.1000000000000000472, 0.003490658503988666988 ) ;
#21363 = ORIENTED_EDGE ( 'NONE', *, *, #60829, .F. ) ;
#21365 = CIRCLE ( 'NONE', #42306, 0.06509327318403745899 ) ;
#21364 = DIRECTION ( 'NONE',  ( 0.000000000000000000, 1.000000000000000000, 0.000000000000000000 ) ) ;
#21366 = EDGE_LOOP ( 'NONE', ( #21082, #31921, #123930, #10180 ) ) ;
#21367 = VECTOR ( 'NONE', #46051, 1000.000000000000000 ) ;
#21369 = ORIENTED_EDGE ( 'NONE', *, *, #31185, .F. ) ;
#21368 = AXIS2_PLACEMENT_3D ( 'NONE', #106787, #127099, #17093 ) ;
#21370 = AXIS2_PLACEMENT_3D ( 'NONE', #108702, #50424, #8547 ) ;
#21371 = DIRECTION ( 'NONE',  ( 0.000000000000000000, -0.9999939076577903929, 0.003490651415223739937 ) ) ;
#21372 = CARTESIAN_POINT ( 'NONE',  ( -9.600000000000006750, 12.50000000000000000, -0.6928203230275542523 ) ) ;
#21373 = DIRECTION ( 'NONE',  ( 0.000000000000000000, 1.000000000000000000, 0.000000000000000000 ) ) ;
#21374 = CARTESIAN_POINT ( 'NONE',  ( 17.49862860983167323, 2.500000000000000000, -4.081131818001370704 ) ) ;
#21375 = ORIENTED_EDGE ( 'NONE', *, *, #26333, .F. ) ;
#21376 = CIRCLE ( 'NONE', #71555, 0.09999999999999982514 ) ;
#21377 = CARTESIAN_POINT ( 'NONE',  ( -9.999999999999969802, 2.500000000000000000, 4.330127018922196314 ) ) ;
#21378 = ORIENTED_EDGE ( 'NONE', *, *, #128425, .F. ) ;
#21379 = DIRECTION ( 'NONE',  ( 0.000000000000000000, 0.000000000000000000, -1.000000000000000000 ) ) ;
#21380 = DIRECTION ( 'NONE',  ( 0.000000000000000000, 0.000000000000000000, 1.000000000000000000 ) ) ;
#21381 = ORIENTED_EDGE ( 'NONE', *, *, #50221, .F. ) ;
#21382 = EDGE_CURVE ( 'NONE', #53076, #53205, #103061, .T. ) ;
#21383 = VERTEX_POINT ( 'NONE', #92117 ) ;
#21385 = ORIENTED_EDGE ( 'NONE', *, *, #15977, .T. ) ;
#21384 = EDGE_CURVE ( 'NONE', #107586, #11222, #2811, .T. ) ;
#21386 = EDGE_LOOP ( 'NONE', ( #52495, #36854 ) ) ;
#21387 = CARTESIAN_POINT ( 'NONE',  ( -0.4000000000000396572, 12.50000000000000000, 4.330127018922196314 ) ) ;
#21388 = CARTESIAN_POINT ( 'NONE',  ( 7.314170287673980475, 2.499999999999874323, 9.688393442490522034 ) ) ;
#21389 = CARTESIAN_POINT ( 'NONE',  ( 0.5999999999999560130, 2.500000000000000000, -3.983716857408426293 ) ) ;
#21390 = FACE_BOUND ( 'NONE', #38573, .T. ) ;
#21391 = DIRECTION ( 'NONE',  ( -0.000000000000000000, 1.000000000000000000, -0.000000000000000000 ) ) ;
#21392 = CARTESIAN_POINT ( 'NONE',  ( 184.8645833340161175, -6.668395609140180369, 3.849999999999994760 ) ) ;
#21393 = CARTESIAN_POINT ( 'NONE',  ( -10.60000000000000320, 12.50000000000000000, -3.983716857408421852 ) ) ;
#21394 = PLANE ( 'NONE',  #85605 ) ;
#21395 = EDGE_CURVE ( 'NONE', #83416, #93002, #122038, .T. ) ;
#21396 = AXIS2_PLACEMENT_3D ( 'NONE', #122830, #124108, #54089 ) ;
#21397 = VECTOR ( 'NONE', #108054, 1000.000000000000000 ) ;
#21399 = CIRCLE ( 'NONE', #52705, 0.06509327318403745899 ) ;
#21398 = CARTESIAN_POINT ( 'NONE',  ( 5.849999999999935696, 12.50000000000000000, -7.188010851410854052 ) ) ;
#21400 = DIRECTION ( 'NONE',  ( 0.000000000000000000, 1.000000000000000000, 0.000000000000000000 ) ) ;
#21401 = CARTESIAN_POINT ( 'NONE',  ( -11.44999999999999751, 12.50000000000000000, 6.776507416713035248 ) ) ;
#21402 = CIRCLE ( 'NONE', #111269, 0.1000000000000000472 ) ;
#21404 = CARTESIAN_POINT ( 'NONE',  ( 11.89999999999990798, 2.500000000000000000, 3.983716857408420964 ) ) ;
#21403 = CIRCLE ( 'NONE', #102973, 0.09999999999999982514 ) ;
#21405 = VECTOR ( 'NONE', #30828, 1000.000000000000000 ) ;
#21406 = ORIENTED_EDGE ( 'NONE', *, *, #112521, .F. ) ;
#21407 = VERTEX_POINT ( 'NONE', #51575 ) ;
#21408 = ORIENTED_EDGE ( 'NONE', *, *, #50741, .T. ) ;
#21409 = ORIENTED_EDGE ( 'NONE', *, *, #117527, .T. ) ;
#21411 = ORIENTED_EDGE ( 'NONE', *, *, #26814, .F. ) ;
#21410 = CIRCLE ( 'NONE', #38141, 0.1000000000000002554 ) ;
#21412 = DIRECTION ( 'NONE',  ( -1.000000000000000000, -0.000000000000000000, -0.000000000000000000 ) ) ;
#21413 = AXIS2_PLACEMENT_3D ( 'NONE', #107271, #57539, #44484 ) ;
#21414 = DIRECTION ( 'NONE',  ( 0.000000000000000000, -0.9999939076577903929, 0.003490651415223739937 ) ) ;
#21415 = EDGE_LOOP ( 'NONE', ( #23464, #92906, #42394, #10914 ) ) ;
#21416 = FACE_BOUND ( 'NONE', #9701, .T. ) ;
#21417 = CONICAL_SURFACE ( 'NONE', #25515, 0.1000000000000000472, 0.003490658503988666988 ) ;
#21418 = CARTESIAN_POINT ( 'NONE',  ( 3.949999999999938005, 2.500000000000000000, 6.941600689897073018 ) ) ;
#21419 = VERTEX_POINT ( 'NONE', #112426 ) ;
#21420 = CARTESIAN_POINT ( 'NONE',  ( 9.599999999999914380, 2.500000000000000000, 3.637306695894644726 ) ) ;
#21421 = FACE_OUTER_BOUND ( 'NONE', #71438, .T. ) ;
#21422 = FACE_OUTER_BOUND ( 'NONE', #37227, .T. ) ;
#21423 = LINE ( 'NONE', #3088, #5711 ) ;
#21424 = VERTEX_POINT ( 'NONE', #13556 ) ;
#21425 = CARTESIAN_POINT ( 'NONE',  ( 2.699999999999946443, 2.500000000000000000, -4.083716857408426826 ) ) ;
#21426 = AXIS2_PLACEMENT_3D ( 'NONE', #8962, #117607, #88822 ) ;
#21427 = EDGE_CURVE ( 'NONE', #107613, #119819, #9063, .T. ) ;
#21428 = VERTEX_POINT ( 'NONE', #111097 ) ;
#21429 = ORIENTED_EDGE ( 'NONE', *, *, #63752, .T. ) ;
#21430 = CARTESIAN_POINT ( 'NONE',  ( -10.40000000000000213, 2.500000000000000000, -5.122947341949750211 ) ) ;
#21431 = DIRECTION ( 'NONE',  ( 0.000000000000000000, 0.000000000000000000, -1.000000000000000000 ) ) ;
#21432 = ORIENTED_EDGE ( 'NONE', *, *, #19447, .T. ) ;
#21433 = DIRECTION ( 'NONE',  ( 0.000000000000000000, 0.000000000000000000, -1.000000000000000000 ) ) ;
#21434 = CONICAL_SURFACE ( 'NONE', #107103, 0.09999999999999982514, 0.003490658503988666988 ) ;
#21436 = FACE_OUTER_BOUND ( 'NONE', #17035, .T. ) ;
#21435 = VECTOR ( 'NONE', #33517, 1000.000000000000000 ) ;
#21437 = CARTESIAN_POINT ( 'NONE',  ( -6.650000000000014566, 2.500000000000000000, 6.495190528383297135 ) ) ;
#21438 = PLANE ( 'NONE',  #93364 ) ;
#21439 = CARTESIAN_POINT ( 'NONE',  ( 9.399999999999918643, 2.500000000000000000, -0.3464101615137782364 ) ) ;
#21440 = ORIENTED_EDGE ( 'NONE', *, *, #116804, .F. ) ;
#21441 = EDGE_CURVE ( 'NONE', #107306, #59034, #105306, .T. ) ;
#21442 = CARTESIAN_POINT ( 'NONE',  ( 9.599999999999914380, 12.50000000000000000, -5.022947341949754119 ) ) ;
#21443 = AXIS2_PLACEMENT_3D ( 'NONE', #8811, #128638, #38976 ) ;
#21444 = ORIENTED_EDGE ( 'NONE', *, *, #74519, .F. ) ;
#21445 = DIRECTION ( 'NONE',  ( 0.000000000000000000, 0.000000000000000000, -1.000000000000000000 ) ) ;
#21446 = AXIS2_PLACEMENT_3D ( 'NONE', #97141, #72206, #11974 ) ;
#21447 = CIRCLE ( 'NONE', #8914, 0.1000000000000002554 ) ;
#21448 = EDGE_LOOP ( 'NONE', ( #66724, #15600, #62941, #118164 ) ) ;
#21449 = AXIS2_PLACEMENT_3D ( 'NONE', #104269, #53882, #93810 ) ;
#21450 = DIRECTION ( 'NONE',  ( -0.000000000000000000, 1.000000000000000000, -0.000000000000000000 ) ) ;
#21451 = EDGE_LOOP ( 'NONE', ( #86390, #128742, #63266, #104940 ) ) ;
#21452 = CARTESIAN_POINT ( 'NONE',  ( 4.199999999999941558, 2.500000000000000000, -4.430127018922202176 ) ) ;
#21453 = DIRECTION ( 'NONE',  ( 0.000000000000000000, 0.000000000000000000, -1.000000000000000000 ) ) ;
#21454 = CARTESIAN_POINT ( 'NONE',  ( -7.500000000000013323, 2.500000000000000000, 5.022947341949748790 ) ) ;
#21456 = EDGE_CURVE ( 'NONE', #84082, #59400, #61408, .T. ) ;
#21455 = CARTESIAN_POINT ( 'NONE',  ( 5.199999999999937117, 2.500000000000000000, -4.676537180435978769 ) ) ;
#21457 = DIRECTION ( 'NONE',  ( -0.000000000000000000, 1.000000000000000000, -0.000000000000000000 ) ) ;
#21458 = VECTOR ( 'NONE', #58269, 1000.000000000000000 ) ;
#21459 = VERTEX_POINT ( 'NONE', #91482 ) ;
#21460 = ORIENTED_EDGE ( 'NONE', *, *, #35659, .F. ) ;
#21461 = CONICAL_SURFACE ( 'NONE', #94605, 0.1000000000000002554, 0.003490658503988666988 ) ;
#21462 = ORIENTED_EDGE ( 'NONE', *, *, #26484, .T. ) ;
#21463 = FACE_OUTER_BOUND ( 'NONE', #73460, .T. ) ;
#21465 = VECTOR ( 'NONE', #87627, 1000.000000000000000 ) ;
#21464 = CARTESIAN_POINT ( 'NONE',  ( 7.299999999999926104, 2.500000000000000000, 4.676537180435972552 ) ) ;
#21466 = AXIS2_PLACEMENT_3D ( 'NONE', #119201, #77984, #57714 ) ;
#21467 = CONICAL_SURFACE ( 'NONE', #523, 0.09999999999999982514, 0.003490658503988666988 ) ;
#21468 = DIRECTION ( 'NONE',  ( 0.000000000000000000, -0.000000000000000000, 1.000000000000000000 ) ) ;
#21470 = EDGE_LOOP ( 'NONE', ( #37722, #39244 ) ) ;
#21469 = ORIENTED_EDGE ( 'NONE', *, *, #95197, .T. ) ;
#21471 = ORIENTED_EDGE ( 'NONE', *, *, #11463, .F. ) ;
#21472 = CARTESIAN_POINT ( 'NONE',  ( -1.250000000000037970, 2.500000000000000000, 2.757883832488649656 ) ) ;
#21473 = VECTOR ( 'NONE', #55550, 1000.000000000000000 ) ;
#21474 = ORIENTED_EDGE ( 'NONE', *, *, #5384, .T. ) ;
#21475 = DIRECTION ( 'NONE',  ( 0.000000000000000000, -0.000000000000000000, 1.000000000000000000 ) ) ;
#21476 = DIRECTION ( 'NONE',  ( 0.000000000000000000, -0.000000000000000000, 1.000000000000000000 ) ) ;
#21477 = FACE_OUTER_BOUND ( 'NONE', #13006, .T. ) ;
#21478 = CARTESIAN_POINT ( 'NONE',  ( 12.89999999999989910, 2.500000000000000000, -0.5928203230275542746 ) ) ;
#21479 = LINE ( 'NONE', #63339, #75829 ) ;
#21480 = CARTESIAN_POINT ( 'NONE',  ( 13.34999999999989662, 12.50000000000000000, -1.537336459617587581 ) ) ;
#21481 = DIRECTION ( 'NONE',  ( -4.274815082592931898E-19, -0.9999939076577903929, -0.003490651415223739937 ) ) ;
#21482 = DIRECTION ( 'NONE',  ( -0.000000000000000000, -1.000000000000000000, -0.000000000000000000 ) ) ;
#21483 = ORIENTED_EDGE ( 'NONE', *, *, #128642, .T. ) ;
#21484 = ADVANCED_FACE ( 'NONE', ( #1801 ), #82234, .T. ) ;
#21485 = CARTESIAN_POINT ( 'NONE',  ( -13.29999999999999005, 2.500000000000000000, -4.230127018922199333 ) ) ;
#21486 = DIRECTION ( 'NONE',  ( -0.000000000000000000, -1.000000000000000000, -0.000000000000000000 ) ) ;
#21487 = ORIENTED_EDGE ( 'NONE', *, *, #71553, .T. ) ;
#21488 = ORIENTED_EDGE ( 'NONE', *, *, #121115, .F. ) ;
#21489 = CIRCLE ( 'NONE', #61204, 0.06509327318403745899 ) ;
#21490 = ADVANCED_FACE ( 'NONE', ( #25975 ), #6988, .T. ) ;
#21491 = CARTESIAN_POINT ( 'NONE',  ( 187.4218750003414016, 0.000000000000000000, 7.564683531250000925 ) ) ;
#21492 = DIRECTION ( 'NONE',  ( -1.000000000000000000, -0.000000000000000000, -0.000000000000000000 ) ) ;
#21493 = DIRECTION ( 'NONE',  ( 0.000000000000000000, 0.000000000000000000, 1.000000000000000000 ) ) ;
#21494 = ADVANCED_FACE ( 'NONE', ( #85531 ), #90631, .T. ) ;
#21495 = CARTESIAN_POINT ( 'NONE',  ( -12.69999999999999396, 12.50000000000000000, -3.983716857408423628 ) ) ;
#21496 = CARTESIAN_POINT ( 'NONE',  ( 13.74999999999993072, 2.500000000000000000, -2.165063509461101710 ) ) ;
#21497 = CARTESIAN_POINT ( 'NONE',  ( -13.74999999999995381, 12.50000000000000000, -2.230156782645137170 ) ) ;
#21498 = AXIS2_PLACEMENT_3D ( 'NONE', #1598, #18670, #71003 ) ;
#21499 = DIRECTION ( 'NONE',  ( -0.000000000000000000, -1.000000000000000000, -0.000000000000000000 ) ) ;
#21500 = DIRECTION ( 'NONE',  ( -4.274815082592931898E-19, -0.9999939076577903929, -0.003490651415223739937 ) ) ;
#21501 = AXIS2_PLACEMENT_3D ( 'NONE', #82480, #12422, #93578 ) ;
#21502 = ADVANCED_FACE ( 'NONE', ( #105164 ), #115668, .T. ) ;
#21503 = VECTOR ( 'NONE', #33111, 1000.000000000000000 ) ;
#21504 = EDGE_CURVE ( 'NONE', #49723, #58972, #42539, .T. ) ;
#21505 = ADVANCED_FACE ( 'NONE', ( #5020 ), #25792, .T. ) ;
#21506 = DIRECTION ( 'NONE',  ( 0.000000000000000000, 1.000000000000000000, 0.000000000000000000 ) ) ;
#21507 = ORIENTED_EDGE ( 'NONE', *, *, #116766, .T. ) ;
#21508 = CIRCLE ( 'NONE', #652, 0.06509327318403745899 ) ;
#21509 = VERTEX_POINT ( 'NONE', #125452 ) ;
#21510 = VECTOR ( 'NONE', #44868, 1000.000000000000000 ) ;
#21511 = ADVANCED_FACE ( 'NONE', ( #6298 ), #116269, .T. ) ;
#21512 = ORIENTED_EDGE ( 'NONE', *, *, #32590, .F. ) ;
#21513 = AXIS2_PLACEMENT_3D ( 'NONE', #37249, #82644, #105971 ) ;
#21514 = CIRCLE ( 'NONE', #121958, 0.09999999999999982514 ) ;
#21515 = ORIENTED_EDGE ( 'NONE', *, *, #13796, .F. ) ;
#21516 = CARTESIAN_POINT ( 'NONE',  ( -8.150000000000014566, 12.50000000000000000, -6.841600689897073373 ) ) ;
#21517 = CARTESIAN_POINT ( 'NONE',  ( 11.24999999999990941, 2.500000000000000000, 7.188010851410848723 ) ) ;
#21518 = ADVANCED_FACE ( 'NONE', ( #86815 ), #80173, .T. ) ;
#21519 = ORIENTED_EDGE ( 'NONE', *, *, #52733, .T. ) ;
#21520 = CARTESIAN_POINT ( 'NONE',  ( 12.69999999999990337, 2.500000000000000000, -4.576537180435978236 ) ) ;
#21521 = CARTESIAN_POINT ( 'NONE',  ( -7.900000000000014566, 12.50000000000000000, -0.6277270498435166823 ) ) ;
#21522 = LINE ( 'NONE', #10405, #49370 ) ;
#21524 = ORIENTED_EDGE ( 'NONE', *, *, #41000, .T. ) ;
#21523 = FACE_OUTER_BOUND ( 'NONE', #121290, .T. ) ;
#21525 = DIRECTION ( 'NONE',  ( 0.000000000000000000, 0.000000000000000000, 1.000000000000000000 ) ) ;
#21527 = CARTESIAN_POINT ( 'NONE',  ( 6.649999999999931077, 2.500000000000000000, -6.495190528383302464 ) ) ;
#21526 = CONICAL_SURFACE ( 'NONE', #19358, 0.1000000000000002554, 0.003490658503988666988 ) ;
#21528 = ORIENTED_EDGE ( 'NONE', *, *, #45848, .F. ) ;
#21529 = ORIENTED_EDGE ( 'NONE', *, *, #37666, .F. ) ;
#21530 = EDGE_LOOP ( 'NONE', ( #40027, #9508 ) ) ;
#21531 = ORIENTED_EDGE ( 'NONE', *, *, #22675, .T. ) ;
#21532 = CARTESIAN_POINT ( 'NONE',  ( -2.100000000000034284, 12.50000000000000000, -4.330127018922201643 ) ) ;
#21534 = AXIS2_PLACEMENT_3D ( 'NONE', #64347, #62434, #52592 ) ;
#21533 = CARTESIAN_POINT ( 'NONE',  ( -11.89999999999999680, 12.50000000000000000, -0.2813168883297367806 ) ) ;
#21535 = CARTESIAN_POINT ( 'NONE',  ( -14.99999999999994671, 2.500000000000000000, 0.1000000000000000056 ) ) ;
#21536 = VECTOR ( 'NONE', #99178, 1000.000000000000000 ) ;
#21537 = ORIENTED_EDGE ( 'NONE', *, *, #77501, .F. ) ;
#21538 = CARTESIAN_POINT ( 'NONE',  ( -1.050000000000038680, 2.500000000000000000, 6.841600689897072485 ) ) ;
#21539 = ORIENTED_EDGE ( 'NONE', *, *, #111762, .F. ) ;
#21540 = LINE ( 'NONE', #70637, #3538 ) ;
#21541 = DIRECTION ( 'NONE',  ( 0.000000000000000000, 1.000000000000000000, 0.000000000000000000 ) ) ;
#21542 = CARTESIAN_POINT ( 'NONE',  ( -5.650000000000023448, 2.500000000000000000, -6.148780366869526226 ) ) ;
#21543 = DIRECTION ( 'NONE',  ( 0.000000000000000000, -0.000000000000000000, 1.000000000000000000 ) ) ;
#21544 = CIRCLE ( 'NONE', #6840, 0.06509327318403745899 ) ;
#21545 = CONICAL_SURFACE ( 'NONE', #125986, 0.09999999999999982514, 0.003490658503988666988 ) ;
#21546 = AXIS2_PLACEMENT_3D ( 'NONE', #7256, #77305, #120452 ) ;
#21547 = ORIENTED_EDGE ( 'NONE', *, *, #2264, .T. ) ;
#21548 = VECTOR ( 'NONE', #115349, 1000.000000000000000 ) ;
#21549 = ADVANCED_FACE ( 'NONE', ( #86151 ), #54142, .T. ) ;
#21550 = VERTEX_POINT ( 'NONE', #5662 ) ;
#21551 = VERTEX_POINT ( 'NONE', #14826 ) ;
#21552 = CARTESIAN_POINT ( 'NONE',  ( -6.650000000000014566, 12.50000000000000000, 6.560283801567334372 ) ) ;
#21553 = DIRECTION ( 'NONE',  ( 0.000000000000000000, 0.000000000000000000, -1.000000000000000000 ) ) ;
#21554 = FACE_BOUND ( 'NONE', #102693, .T. ) ;
#21555 = DIRECTION ( 'NONE',  ( 0.000000000000000000, 0.000000000000000000, 1.000000000000000000 ) ) ;
#21557 = DIRECTION ( 'NONE',  ( -0.000000000000000000, 1.000000000000000000, -0.000000000000000000 ) ) ;
#21556 = CONICAL_SURFACE ( 'NONE', #94704, 0.09999999999999982514, 0.003490658503988666988 ) ;
#21558 = DIRECTION ( 'NONE',  ( 0.000000000000000000, 1.000000000000000000, 0.000000000000000000 ) ) ;
#21559 = ADVANCED_FACE ( 'NONE', ( #24684 ), #64599, .T. ) ;
#21560 = AXIS2_PLACEMENT_3D ( 'NONE', #12922, #101980, #31957 ) ;
#21561 = VECTOR ( 'NONE', #63188, 1000.000000000000000 ) ;
#21562 = AXIS2_PLACEMENT_3D ( 'NONE', #39193, #79734, #86972 ) ;
#21563 = DIRECTION ( 'NONE',  ( 0.000000000000000000, 1.000000000000000000, 0.000000000000000000 ) ) ;
#21564 = DIRECTION ( 'NONE',  ( 0.000000000000000000, 0.000000000000000000, 1.000000000000000000 ) ) ;
#21565 = VECTOR ( 'NONE', #43026, 1000.000000000000000 ) ;
#21566 = CARTESIAN_POINT ( 'NONE',  ( -9.150000000000009237, 12.50000000000000000, -1.472243186433550122 ) ) ;
#21567 = EDGE_LOOP ( 'NONE', ( #98839, #100226, #90229, #16865 ) ) ;
#21568 = DIRECTION ( 'NONE',  ( -0.000000000000000000, -1.000000000000000000, -0.000000000000000000 ) ) ;
#21569 = LINE ( 'NONE', #121690, #64279 ) ;
#21570 = CIRCLE ( 'NONE', #69390, 0.06509327318403745899 ) ;
#21571 = VERTEX_POINT ( 'NONE', #126091 ) ;
#21572 = ORIENTED_EDGE ( 'NONE', *, *, #77750, .T. ) ;
#21573 = CARTESIAN_POINT ( 'NONE',  ( -2.900000000000029221, 12.50000000000000000, -5.022947341949754119 ) ) ;
#21574 = DIRECTION ( 'NONE',  ( 0.000000000000000000, 1.000000000000000000, 0.000000000000000000 ) ) ;
#21575 = FACE_BOUND ( 'NONE', #59744, .T. ) ;
#21576 = CARTESIAN_POINT ( 'NONE',  ( 6.249999999999932498, 2.500000000000000000, -5.802370205355749988 ) ) ;
#21578 = EDGE_LOOP ( 'NONE', ( #59106, #67275 ) ) ;
#21577 = AXIS2_PLACEMENT_3D ( 'NONE', #80414, #29384, #90199 ) ;
#21580 = CIRCLE ( 'NONE', #73899, 0.1000000000000002554 ) ;
#21579 = CARTESIAN_POINT ( 'NONE',  ( 4.399999999999939071, 2.500000000000000000, -0.3464101615137782364 ) ) ;
#21581 = DIRECTION ( 'NONE',  ( -0.000000000000000000, -1.000000000000000000, -0.000000000000000000 ) ) ;
#21582 = EDGE_LOOP ( 'NONE', ( #69399, #18895, #2034, #56270 ) ) ;
#21583 = FACE_OUTER_BOUND ( 'NONE', #87543, .T. ) ;
#21584 = FACE_OUTER_BOUND ( 'NONE', #88625, .T. ) ;
#21585 = ADVANCED_FACE ( 'NONE', ( #56689 ), #30013, .T. ) ;
#21586 = VECTOR ( 'NONE', #67734, 1000.000000000000000 ) ;
#21587 = CONICAL_SURFACE ( 'NONE', #67534, 0.1000000000000002554, 0.003490658503988666988 ) ;
#21588 = AXIS2_PLACEMENT_3D ( 'NONE', #109841, #68614, #50278 ) ;
#21589 = AXIS2_PLACEMENT_3D ( 'NONE', #84768, #116147, #124697 ) ;
#21590 = DIRECTION ( 'NONE',  ( -4.274815082592931898E-19, -0.9999939076577903929, -0.003490651415223739937 ) ) ;
#21591 = DIRECTION ( 'NONE',  ( -0.000000000000000000, 1.000000000000000000, -0.000000000000000000 ) ) ;
#21592 = EDGE_CURVE ( 'NONE', #94263, #102067, #65884, .T. ) ;
#21593 = AXIS2_PLACEMENT_3D ( 'NONE', #104732, #75930, #115183 ) ;
#21595 = ORIENTED_EDGE ( 'NONE', *, *, #58363, .T. ) ;
#21594 = AXIS2_PLACEMENT_3D ( 'NONE', #48674, #10035, #855 ) ;
#21596 = DIRECTION ( 'NONE',  ( -0.000000000000000000, 1.000000000000000000, -0.000000000000000000 ) ) ;
#21597 = PLANE ( 'NONE',  #22540 ) ;
#21598 = CARTESIAN_POINT ( 'NONE',  ( -12.49999999999995914, 2.500000000000000000, 1.843143693225357538E-15 ) ) ;
#21599 = AXIS2_PLACEMENT_3D ( 'NONE', #81031, #61395, #11636 ) ;
#21601 = ORIENTED_EDGE ( 'NONE', *, *, #95960, .F. ) ;
#21600 = AXIS2_PLACEMENT_3D ( 'NONE', #94401, #113411, #45329 ) ;
#21602 = EDGE_CURVE ( 'NONE', #99945, #46684, #57188, .T. ) ;
#21603 = EDGE_LOOP ( 'NONE', ( #116989, #11284, #19680, #42295 ) ) ;
#21604 = EDGE_CURVE ( 'NONE', #49367, #21810, #96001, .T. ) ;
#21605 = CARTESIAN_POINT ( 'NONE',  ( -6.050000000000017586, 2.500000000000000000, 6.248780366869520542 ) ) ;
#21606 = CIRCLE ( 'NONE', #32087, 0.1000000000000002554 ) ;
#21607 = ORIENTED_EDGE ( 'NONE', *, *, #122559, .T. ) ;
#21608 = PLANE ( 'NONE',  #15674 ) ;
#21609 = CARTESIAN_POINT ( 'NONE',  ( 9.149999999999920419, 2.500000000000000000, 2.957883832488649389 ) ) ;
#21610 = DIRECTION ( 'NONE',  ( 0.000000000000000000, 0.000000000000000000, -1.000000000000000000 ) ) ;
#21611 = VERTEX_POINT ( 'NONE', #37088 ) ;
#21612 = ADVANCED_FACE ( 'NONE', ( #106458 ), #17461, .T. ) ;
#21613 = CARTESIAN_POINT ( 'NONE',  ( 2.899999999999944844, 2.500000000000000000, 5.022947341949748790 ) ) ;
#21614 = CARTESIAN_POINT ( 'NONE',  ( -5.850000000000021849, 12.50000000000000000, -2.857883832488653741 ) ) ;
#21615 = DIRECTION ( 'NONE',  ( 0.000000000000000000, 0.000000000000000000, 1.000000000000000000 ) ) ;
#21616 = LINE ( 'NONE', #81183, #108210 ) ;
#21617 = PLANE ( 'NONE',  #67399 ) ;
#21618 = EDGE_CURVE ( 'NONE', #78911, #48128, #126143, .T. ) ;
#21619 = DIRECTION ( 'NONE',  ( 0.000000000000000000, -0.000000000000000000, 1.000000000000000000 ) ) ;
#21620 = CIRCLE ( 'NONE', #78048, 0.06509327318403741736 ) ;
#21621 = ORIENTED_EDGE ( 'NONE', *, *, #97283, .T. ) ;
#21622 = EDGE_LOOP ( 'NONE', ( #120827, #34843, #108432, #4365 ) ) ;
#21623 = DIRECTION ( 'NONE',  ( -0.000000000000000000, 1.000000000000000000, -0.000000000000000000 ) ) ;
#21624 = EDGE_LOOP ( 'NONE', ( #9245, #12325 ) ) ;
#21625 = LINE ( 'NONE', #70083, #61918 ) ;
#21627 = EDGE_LOOP ( 'NONE', ( #116586, #98430, #58807, #87717 ) ) ;
#21626 = ORIENTED_EDGE ( 'NONE', *, *, #90922, .F. ) ;
#21628 = VERTEX_POINT ( 'NONE', #78953 ) ;
#21629 = CARTESIAN_POINT ( 'NONE',  ( -11.89999999999999680, 2.500000000000000000, -4.676537180435976104 ) ) ;
#21630 = CONICAL_SURFACE ( 'NONE', #17397, 0.09999999999999982514, 0.003490658503988666988 ) ;
#21631 = AXIS2_PLACEMENT_3D ( 'NONE', #44109, #84024, #55858 ) ;
#21632 = CARTESIAN_POINT ( 'NONE',  ( 4.349999999999938360, 2.500000000000000000, 1.818653347947321475 ) ) ;
#21633 = AXIS2_PLACEMENT_3D ( 'NONE', #118140, #129281, #28482 ) ;
#21634 = CARTESIAN_POINT ( 'NONE',  ( 5.599999999999933031, 2.500000000000000000, 0.3464101615137735735 ) ) ;
#21635 =( LENGTH_UNIT ( ) NAMED_UNIT ( * ) SI_UNIT ( .MILLI., .METRE. ) );
#21636 = DIRECTION ( 'NONE',  ( 0.000000000000000000, 1.000000000000000000, 0.000000000000000000 ) ) ;
#21637 = FACE_OUTER_BOUND ( 'NONE', #21255, .T. ) ;
#21638 = DIRECTION ( 'NONE',  ( 0.000000000000000000, -0.9999939076577903929, 0.003490651415223739937 ) ) ;
#21639 = DIRECTION ( 'NONE',  ( -4.274815082592931898E-19, -0.9999939076577903929, -0.003490651415223739937 ) ) ;
#21640 = FACE_OUTER_BOUND ( 'NONE', #24442, .T. ) ;
#21641 = CONICAL_SURFACE ( 'NONE', #115617, 0.1000000000000002554, 0.003490658503988666988 ) ;
#21642 = DIRECTION ( 'NONE',  ( 1.000000000000000000, 0.000000000000000000, 0.000000000000000000 ) ) ;
#21643 = VECTOR ( 'NONE', #54757, 1000.000000000000000 ) ;
#21644 = VERTEX_POINT ( 'NONE', #119494 ) ;
#21645 = AXIS2_PLACEMENT_3D ( 'NONE', #41979, #34093, #113938 ) ;
#21646 = EDGE_CURVE ( 'NONE', #51736, #111655, #4931, .T. ) ;
#21647 = DIRECTION ( 'NONE',  ( 0.000000000000000000, 1.000000000000000000, 0.000000000000000000 ) ) ;
#21648 = EDGE_LOOP ( 'NONE', ( #77586, #22706, #119675, #56170 ) ) ;
#21649 = EDGE_LOOP ( 'NONE', ( #59104, #357, #77097, #119739 ) ) ;
#21650 = DIRECTION ( 'NONE',  ( -0.000000000000000000, -1.000000000000000000, -0.000000000000000000 ) ) ;
#21652 = CIRCLE ( 'NONE', #107612, 0.1000000000000000472 ) ;
#21651 = DIRECTION ( 'NONE',  ( 0.000000000000000000, -0.9999939076577903929, 0.003490651415223739937 ) ) ;
#21653 = DIRECTION ( 'NONE',  ( 0.000000000000000000, 0.000000000000000000, 1.000000000000000000 ) ) ;
#21654 = EDGE_CURVE ( 'NONE', #108166, #82548, #71869, .T. ) ;
#21655 = DIRECTION ( 'NONE',  ( 0.000000000000000000, 0.000000000000000000, 1.000000000000000000 ) ) ;
#21656 = CARTESIAN_POINT ( 'NONE',  ( 15.39999999999989200, 2.500000000000000000, -0.5928203230275542746 ) ) ;
#21657 = AXIS2_PLACEMENT_3D ( 'NONE', #120105, #30453, #70352 ) ;
#21658 = DIRECTION ( 'NONE',  ( 0.000000000000000000, 0.000000000000000000, 1.000000000000000000 ) ) ;
#21659 = CONICAL_SURFACE ( 'NONE', #34188, 0.09999999999999982514, 0.003490658503988666988 ) ;
#21660 = AXIS2_PLACEMENT_3D ( 'NONE', #37089, #127399, #118214 ) ;
#21661 = LINE ( 'NONE', #89747, #42551 ) ;
#21662 = ORIENTED_EDGE ( 'NONE', *, *, #119862, .T. ) ;
#21663 = EDGE_CURVE ( 'NONE', #24371, #24257, #119883, .T. ) ;
#21664 = CIRCLE ( 'NONE', #73884, 0.1000000000000002554 ) ;
#21665 = EDGE_CURVE ( 'NONE', #113481, #90527, #15397, .T. ) ;
#21666 = EDGE_CURVE ( 'NONE', #67886, #14684, #124080, .T. ) ;
#21667 = AXIS2_PLACEMENT_3D ( 'NONE', #107539, #36874, #97710 ) ;
#21668 = ORIENTED_EDGE ( 'NONE', *, *, #29629, .T. ) ;
#21669 = ORIENTED_EDGE ( 'NONE', *, *, #14564, .T. ) ;
#21670 = ADVANCED_FACE ( 'NONE', ( #118856 ), #78129, .T. ) ;
#21671 = ORIENTED_EDGE ( 'NONE', *, *, #107475, .T. ) ;
#21672 = ORIENTED_EDGE ( 'NONE', *, *, #47397, .F. ) ;
#21673 = DIRECTION ( 'NONE',  ( -0.000000000000000000, -1.000000000000000000, -0.000000000000000000 ) ) ;
#21674 = FACE_OUTER_BOUND ( 'NONE', #52841, .T. ) ;
#21675 = ADVANCED_FACE ( 'NONE', ( #40315 ), #111562, .T. ) ;
#21676 = ADVANCED_FACE ( 'NONE', ( #90023 ), #40584, .T. ) ;
#21677 = LINE ( 'NONE', #20385, #111485 ) ;
#21678 = CARTESIAN_POINT ( 'NONE',  ( -0.6000000000000388356, 2.500000000000000000, 4.776537180435972196 ) ) ;
#21679 = DIRECTION ( 'NONE',  ( 0.000000000000000000, -0.000000000000000000, 1.000000000000000000 ) ) ;
#21680 = ORIENTED_EDGE ( 'NONE', *, *, #11314, .T. ) ;
#21681 = CARTESIAN_POINT ( 'NONE',  ( -14.39999999999998614, 2.500000000000000000, -0.3464101615137760715 ) ) ;
#21683 = AXIS2_PLACEMENT_3D ( 'NONE', #25330, #36479, #96637 ) ;
#21682 = DIRECTION ( 'NONE',  ( 0.000000000000000000, 0.000000000000000000, 1.000000000000000000 ) ) ;
#21684 = AXIS2_PLACEMENT_3D ( 'NONE', #63460, #103382, #75836 ) ;
#21685 = CARTESIAN_POINT ( 'NONE',  ( -5.850000000000022737, 2.500000000000000000, -2.165063509461101710 ) ) ;
#21686 = DIRECTION ( 'NONE',  ( 0.000000000000000000, 1.000000000000000000, 0.000000000000000000 ) ) ;
#21687 = DIRECTION ( 'NONE',  ( 0.000000000000000000, 0.000000000000000000, 1.000000000000000000 ) ) ;
#21688 = ORIENTED_EDGE ( 'NONE', *, *, #77901, .T. ) ;
#21689 = CONICAL_SURFACE ( 'NONE', #107350, 0.1000000000000002554, 0.003490658503988666988 ) ;
#21690 = CIRCLE ( 'NONE', #61405, 0.06509327318403745899 ) ;
#21691 = ORIENTED_EDGE ( 'NONE', *, *, #67572, .F. ) ;
#21692 = ORIENTED_EDGE ( 'NONE', *, *, #17914, .T. ) ;
#21693 = AXIS2_PLACEMENT_3D ( 'NONE', #34890, #96346, #13922 ) ;
#21694 = DIRECTION ( 'NONE',  ( 0.000000000000000000, 1.000000000000000000, 0.000000000000000000 ) ) ;
#21695 = ORIENTED_EDGE ( 'NONE', *, *, #24774, .T. ) ;
#21696 = CARTESIAN_POINT ( 'NONE',  ( 9.149999999999918643, 2.500000000000000000, -6.495190528383302464 ) ) ;
#21697 = DIRECTION ( 'NONE',  ( -0.000000000000000000, 1.000000000000000000, -0.000000000000000000 ) ) ;
#21698 = AXIS2_PLACEMENT_3D ( 'NONE', #34749, #36018, #95583 ) ;
#21699 = CONICAL_SURFACE ( 'NONE', #32078, 0.09999999999999982514, 0.003490658503988666988 ) ;
#21700 = VECTOR ( 'NONE', #127197, 1000.000000000000000 ) ;
#21701 = CIRCLE ( 'NONE', #94851, 0.06509327318403743123 ) ;
#21702 = EDGE_LOOP ( 'NONE', ( #583, #54217, #24754, #91011 ) ) ;
#21703 = CARTESIAN_POINT ( 'NONE',  ( -0.6500000000000389910, 12.50000000000000000, -1.818653347947326138 ) ) ;
#21704 = CARTESIAN_POINT ( 'NONE',  ( 7.499999999999927169, 12.50000000000000000, 3.637306695894644726 ) ) ;
#21705 = FACE_OUTER_BOUND ( 'NONE', #39190, .T. ) ;
#21706 = FACE_OUTER_BOUND ( 'NONE', #101436, .T. ) ;
#21707 = DIRECTION ( 'NONE',  ( 0.000000000000000000, 1.000000000000000000, 0.000000000000000000 ) ) ;
#21708 = VERTEX_POINT ( 'NONE', #109691 ) ;
#21709 = ORIENTED_EDGE ( 'NONE', *, *, #102018, .T. ) ;
#21710 = FACE_OUTER_BOUND ( 'NONE', #78756, .T. ) ;
#21711 = DIRECTION ( 'NONE',  ( 0.000000000000000000, 0.000000000000000000, 1.000000000000000000 ) ) ;
#21712 = DIRECTION ( 'NONE',  ( 0.000000000000000000, 0.000000000000000000, 1.000000000000000000 ) ) ;
#21713 = CARTESIAN_POINT ( 'NONE',  ( 0.4499999999999573785, 2.500000000000000000, -6.495190528383302464 ) ) ;
#21714 = EDGE_CURVE ( 'NONE', #113119, #90074, #69806, .T. ) ;
#21715 = EDGE_LOOP ( 'NONE', ( #124464, #29054, #56279, #47572 ) ) ;
#21716 = ORIENTED_EDGE ( 'NONE', *, *, #16450, .F. ) ;
#21717 = CARTESIAN_POINT ( 'NONE',  ( 11.44999999999990870, 2.500000000000000000, 6.841600689897072485 ) ) ;
#21718 = CARTESIAN_POINT ( 'NONE',  ( -11.69999999999999929, 2.500000000000000000, 1.734723475976807094E-15 ) ) ;
#21719 = CARTESIAN_POINT ( 'NONE',  ( 0.6499999999999566125, 12.50000000000000000, -6.148780366869526226 ) ) ;
#21720 = CIRCLE ( 'NONE', #88309, 0.06509327318403745899 ) ;
#21721 = CARTESIAN_POINT ( 'NONE',  ( 12.69999999999990159, 2.500000000000000000, -4.083716857408426826 ) ) ;
#21722 = ORIENTED_EDGE ( 'NONE', *, *, #41881, .F. ) ;
#21723 = CONICAL_SURFACE ( 'NONE', #109452, 0.09999999999999982514, 0.003490658503988666988 ) ;
#21724 = CONICAL_SURFACE ( 'NONE', #67774, 0.09999999999999982514, 0.003490658503988666988 ) ;
#21725 = FACE_OUTER_BOUND ( 'NONE', #11986, .T. ) ;
#21726 = CARTESIAN_POINT ( 'NONE',  ( 3.349999999999941913, 2.500000000000000000, 5.802370205355744659 ) ) ;
#21727 = ORIENTED_EDGE ( 'NONE', *, *, #70151, .T. ) ;
#21728 = CARTESIAN_POINT ( 'NONE',  ( 6.449999999999931788, 2.500000000000000000, -6.148780366869526226 ) ) ;
#21729 = AXIS2_PLACEMENT_3D ( 'NONE', #25406, #66629, #29304 ) ;
#21730 = ORIENTED_EDGE ( 'NONE', *, *, #66679, .T. ) ;
#21731 = VECTOR ( 'NONE', #10839, 1000.000000000000000 ) ;
#21732 = DIRECTION ( 'NONE',  ( 0.000000000000000000, 1.000000000000000000, 0.000000000000000000 ) ) ;
#21733 = CIRCLE ( 'NONE', #13305, 0.09999999999999982514 ) ;
#21734 = ORIENTED_EDGE ( 'NONE', *, *, #52932, .T. ) ;
#21735 = AXIS2_PLACEMENT_3D ( 'NONE', #42976, #25878, #53417 ) ;
#21736 = ORIENTED_EDGE ( 'NONE', *, *, #110052, .F. ) ;
#21737 = CARTESIAN_POINT ( 'NONE',  ( -10.00000000000000533, 2.500000000000000000, 0.6928203230275494784 ) ) ;
#21738 = DIRECTION ( 'NONE',  ( 0.000000000000000000, 1.000000000000000000, -0.000000000000000000 ) ) ;
#21739 = EDGE_LOOP ( 'NONE', ( #19311, #108600 ) ) ;
#21740 = ORIENTED_EDGE ( 'NONE', *, *, #9213, .F. ) ;
#21741 = AXIS2_PLACEMENT_3D ( 'NONE', #109002, #68440, #18049 ) ;
#21742 = DIRECTION ( 'NONE',  ( -4.274815082592931898E-19, -0.9999939076577903929, -0.003490651415223739937 ) ) ;
#21743 = DIRECTION ( 'NONE',  ( 0.000000000000000000, -0.000000000000000000, 1.000000000000000000 ) ) ;
#21744 = ORIENTED_EDGE ( 'NONE', *, *, #8200, .F. ) ;
#21745 = CARTESIAN_POINT ( 'NONE',  ( 1.249999999999952038, 12.50000000000000000, -1.407149913249512663 ) ) ;
#21746 = CARTESIAN_POINT ( 'NONE',  ( 186.2343750003414016, 8.734944146203032389, 5.348610694689227483E-16 ) ) ;
#21747 = CARTESIAN_POINT ( 'NONE',  ( 0.7999999999999548583, 2.500000000000000000, 4.430127018922196847 ) ) ;
#21748 = VECTOR ( 'NONE', #67583, 1000.000000000000000 ) ;
#21749 = CARTESIAN_POINT ( 'NONE',  ( -2.900000000000029221, 2.500000000000000000, -5.122947341949753763 ) ) ;
#21750 = FACE_OUTER_BOUND ( 'NONE', #95351, .T. ) ;
#21751 = CARTESIAN_POINT ( 'NONE',  ( 8.149999999999920419, 12.50000000000000000, 6.776507416713035248 ) ) ;
#21752 = CIRCLE ( 'NONE', #48949, 0.09999999999999982514 ) ;
#21753 = FACE_OUTER_BOUND ( 'NONE', #17128, .T. ) ;
#21754 = AXIS2_PLACEMENT_3D ( 'NONE', #69864, #89500, #109786 ) ;
#21755 = EDGE_CURVE ( 'NONE', #90522, #77475, #65675, .T. ) ;
#21756 = ORIENTED_EDGE ( 'NONE', *, *, #50319, .F. ) ;
#21757 = VERTEX_POINT ( 'NONE', #7607 ) ;
#21758 = CARTESIAN_POINT ( 'NONE',  ( -9.350000000000006750, 12.50000000000000000, -2.511473670974877948 ) ) ;
#21759 = ORIENTED_EDGE ( 'NONE', *, *, #47965, .F. ) ;
#21760 = CARTESIAN_POINT ( 'NONE',  ( 11.04999999999990656, 2.500000000000000000, -6.148780366869526226 ) ) ;
#21761 = FACE_OUTER_BOUND ( 'NONE', #114281, .T. ) ;
#21762 = DIRECTION ( 'NONE',  ( 0.000000000000000000, 0.000000000000000000, -1.000000000000000000 ) ) ;
#21764 = ORIENTED_EDGE ( 'NONE', *, *, #30403, .F. ) ;
#21763 = ORIENTED_EDGE ( 'NONE', *, *, #115422, .T. ) ;
#21765 = ADVANCED_FACE ( 'NONE', ( #99875 ), #353, .T. ) ;
#21766 = FACE_BOUND ( 'NONE', #39678, .T. ) ;
#21767 = ORIENTED_EDGE ( 'NONE', *, *, #38743, .F. ) ;
#21768 = ADVANCED_FACE ( 'NONE', ( #127398 ), #49499, .T. ) ;
#21769 = FACE_OUTER_BOUND ( 'NONE', #110643, .T. ) ;
#21770 = FACE_OUTER_BOUND ( 'NONE', #37755, .T. ) ;
#21771 = CARTESIAN_POINT ( 'NONE',  ( 8.949999999999919353, 2.500000000000000000, -6.248780366869526759 ) ) ;
#21772 = CARTESIAN_POINT ( 'NONE',  ( 195.5000000000000000, 0.000000000000000000, -3.500000000000000000 ) ) ;
#21773 = CARTESIAN_POINT ( 'NONE',  ( -5.850000000000018296, 2.500000000000000000, 5.702370205355745014 ) ) ;
#21774 = CARTESIAN_POINT ( 'NONE',  ( -10.65000000000000213, 2.500000000000000000, 6.841600689897072485 ) ) ;
#21775 = EDGE_CURVE ( 'NONE', #105608, #86126, #80233, .T. ) ;
#21776 = CONICAL_SURFACE ( 'NONE', #105387, 0.1000000000000002554, 0.003490658503988666988 ) ;
#21777 = DIRECTION ( 'NONE',  ( 0.000000000000000000, 0.000000000000000000, 1.000000000000000000 ) ) ;
#21778 = EDGE_CURVE ( 'NONE', #82940, #99080, #58018, .T. ) ;
#21779 = CARTESIAN_POINT ( 'NONE',  ( -2.900000000000030109, 12.50000000000000000, 0.6928203230275494784 ) ) ;
#21780 = CONICAL_SURFACE ( 'NONE', #109602, 0.1000000000000002554, 0.003490658503988666988 ) ;
#21781 = CONICAL_SURFACE ( 'NONE', #38512, 0.09999999999999982514, 0.003490658503988666988 ) ;
#21782 = DIRECTION ( 'NONE',  ( 0.000000000000000000, -0.9999939076577903929, 0.003490651415223739937 ) ) ;
#21783 = CARTESIAN_POINT ( 'NONE',  ( 4.399999999999939071, 12.50000000000000000, -0.2813168883297408329 ) ) ;
#21784 = EDGE_CURVE ( 'NONE', #103084, #47024, #5033, .T. ) ;
#21785 = LINE ( 'NONE', #62981, #116118 ) ;
#21786 = AXIS2_PLACEMENT_3D ( 'NONE', #72270, #64990, #104294 ) ;
#21788 = EDGE_LOOP ( 'NONE', ( #38789, #96304, #104229, #81836 ) ) ;
#21787 = CIRCLE ( 'NONE', #69801, 0.06509327318403745899 ) ;
#21789 = ORIENTED_EDGE ( 'NONE', *, *, #91262, .F. ) ;
#21790 = EDGE_LOOP ( 'NONE', ( #78838, #77133, #5114, #330 ) ) ;
#21791 = AXIS2_PLACEMENT_3D ( 'NONE', #69004, #39586, #48741 ) ;
#21792 = EDGE_LOOP ( 'NONE', ( #80445, #77387, #86813, #44809 ) ) ;
#21794 = AXIS2_PLACEMENT_3D ( 'NONE', #122730, #70407, #41611 ) ;
#21793 = CARTESIAN_POINT ( 'NONE',  ( -3.100000000000028955, 2.500000000000000000, 4.676537180435972552 ) ) ;
#21795 = DIRECTION ( 'NONE',  ( -0.000000000000000000, -1.000000000000000000, -0.000000000000000000 ) ) ;
#21797 = ORIENTED_EDGE ( 'NONE', *, *, #114001, .T. ) ;
#21796 = ORIENTED_EDGE ( 'NONE', *, *, #100693, .T. ) ;
#21798 = ORIENTED_EDGE ( 'NONE', *, *, #88887, .F. ) ;
#21799 = DIRECTION ( 'NONE',  ( 0.000000000000000000, 1.000000000000000000, 0.000000000000000000 ) ) ;
#21800 = AXIS2_PLACEMENT_3D ( 'NONE', #8469, #58881, #117771 ) ;
#21801 = CONICAL_SURFACE ( 'NONE', #48897, 0.1000000000000002554, 0.003490658503988666988 ) ;
#21802 = VECTOR ( 'NONE', #119781, 1000.000000000000000 ) ;
#21803 = DIRECTION ( 'NONE',  ( -0.000000000000000000, 1.000000000000000000, -0.000000000000000000 ) ) ;
#21804 = DIRECTION ( 'NONE',  ( 0.000000000000000000, 0.000000000000000000, 1.000000000000000000 ) ) ;
#21805 = CARTESIAN_POINT ( 'NONE',  ( 12.09999999999990550, 2.500000000000000000, 4.922947341949748257 ) ) ;
#21806 = CARTESIAN_POINT ( 'NONE',  ( -8.350000000000013856, 12.50000000000000000, 2.165063509461097713 ) ) ;
#21807 = DIRECTION ( 'NONE',  ( 0.000000000000000000, 1.000000000000000000, 0.000000000000000000 ) ) ;
#21808 = VERTEX_POINT ( 'NONE', #20025 ) ;
#21809 = CARTESIAN_POINT ( 'NONE',  ( 0.000000000000000000, 0.000000000000000000, 6.000000000000005329 ) ) ;
#21810 = VERTEX_POINT ( 'NONE', #107090 ) ;
#21811 = ORIENTED_EDGE ( 'NONE', *, *, #6821, .T. ) ;
#21812 = ORIENTED_EDGE ( 'NONE', *, *, #81163, .F. ) ;
#21813 = DIRECTION ( 'NONE',  ( -4.274815082592931898E-19, -0.9999939076577903929, -0.003490651415223739937 ) ) ;
#21814 = ADVANCED_FACE ( 'NONE', ( #8250 ), #128716, .T. ) ;
#21815 = VERTEX_POINT ( 'NONE', #38389 ) ;
#21816 = EDGE_LOOP ( 'NONE', ( #32836, #124643 ) ) ;
#21817 = ORIENTED_EDGE ( 'NONE', *, *, #120813, .T. ) ;
#21818 = AXIS2_PLACEMENT_3D ( 'NONE', #7859, #74679, #114590 ) ;
#21819 = SURFACE_STYLE_USAGE ( .BOTH. , #12613 ) ;
#21820 = DIRECTION ( 'NONE',  ( 0.000000000000000000, -0.9999939076577903929, 0.003490651415223739937 ) ) ;
#21821 = LINE ( 'NONE', #73470, #108585 ) ;
#21822 = FACE_OUTER_BOUND ( 'NONE', #53129, .T. ) ;
#21823 = CARTESIAN_POINT ( 'NONE',  ( 0.3999999999999568345, 2.500000000000000000, -4.922947341949753586 ) ) ;
#21824 = ADVANCED_FACE ( 'NONE', ( #121426 ), #115759, .T. ) ;
#21825 = FACE_OUTER_BOUND ( 'NONE', #122654, .T. ) ;
#21826 = ADVANCED_FACE ( 'NONE', ( #81520 ), #82435, .T. ) ;
#21827 = ADVANCED_FACE ( 'NONE', ( #61892 ), #90688, .T. ) ;
#21828 = DIRECTION ( 'NONE',  ( -0.000000000000000000, 1.000000000000000000, -0.000000000000000000 ) ) ;
#21829 = AXIS2_PLACEMENT_3D ( 'NONE', #114621, #34146, #105463 ) ;
#21830 = CIRCLE ( 'NONE', #86653, 0.06509327318403745899 ) ;
#21831 = EDGE_LOOP ( 'NONE', ( #101457, #42612 ) ) ;
#21832 = DIRECTION ( 'NONE',  ( 0.000000000000000000, 0.000000000000000000, 1.000000000000000000 ) ) ;
#21833 = ORIENTED_EDGE ( 'NONE', *, *, #21896, .T. ) ;
#21834 = CARTESIAN_POINT ( 'NONE',  ( 4.799999999999935874, 2.500000000000000000, 0.3464101615137735735 ) ) ;
#21836 = VERTEX_POINT ( 'NONE', #50769 ) ;
#21835 = EDGE_CURVE ( 'NONE', #31016, #51588, #2960, .T. ) ;
#21837 = CARTESIAN_POINT ( 'NONE',  ( -12.69999999999999396, 12.50000000000000000, -3.983716857408423628 ) ) ;
#21838 = EDGE_CURVE ( 'NONE', #111172, #77053, #101808, .T. ) ;
#21839 = ORIENTED_EDGE ( 'NONE', *, *, #59248, .T. ) ;
#21840 = ADVANCED_FACE ( 'NONE', ( #93271 ), #113720, .T. ) ;
#21841 = DIRECTION ( 'NONE',  ( 0.000000000000000000, 0.000000000000000000, 1.000000000000000000 ) ) ;
#21842 = EDGE_CURVE ( 'NONE', #45172, #21163, #31775, .T. ) ;
#21843 = AXIS2_PLACEMENT_3D ( 'NONE', #108931, #109605, #30417 ) ;
#21844 = ADVANCED_FACE ( 'NONE', ( #10803 ), #117909, .T. ) ;
#21845 = DIRECTION ( 'NONE',  ( -4.274815082592931898E-19, -0.9999939076577903929, -0.003490651415223739937 ) ) ;
#21846 = ORIENTED_EDGE ( 'NONE', *, *, #22729, .T. ) ;
#21847 = ORIENTED_EDGE ( 'NONE', *, *, #54613, .F. ) ;
#21848 = DIRECTION ( 'NONE',  ( 0.000000000000000000, 1.000000000000000000, 0.000000000000000000 ) ) ;
#21849 = DIRECTION ( 'NONE',  ( 0.000000000000000000, 0.000000000000000000, -1.000000000000000000 ) ) ;
#21850 = CARTESIAN_POINT ( 'NONE',  ( 184.3385416670080872, 6.551208109652274736, 3.782341765625001351 ) ) ;
#21851 = CARTESIAN_POINT ( 'NONE',  ( -3.950000000000025491, 2.500000000000000000, 6.148780366869520897 ) ) ;
#21852 = ADVANCED_FACE ( 'NONE', ( #40970 ), #91977, .F. ) ;
#21853 = CARTESIAN_POINT ( 'NONE',  ( -7.300000000000016698, 12.50000000000000000, -0.3464101615137783474 ) ) ;
#21854 = ORIENTED_EDGE ( 'NONE', *, *, #63191, .T. ) ;
#21855 = CIRCLE ( 'NONE', #5091, 0.06509327318403745899 ) ;
#21856 = AXIS2_PLACEMENT_3D ( 'NONE', #5633, #106425, #45586 ) ;
#21857 = DIRECTION ( 'NONE',  ( 0.000000000000000000, 0.000000000000000000, 1.000000000000000000 ) ) ;
#21858 = B_SPLINE_CURVE_WITH_KNOTS ( 'NONE', 3,
 ( #26771, #128201, #66683, #38552, #87611, #106609, #85681, #126910, #125595, #66043, #105973, #109177, #111100, #51578, #61398, #69920 ),
 .UNSPECIFIED., .F., .F.,
 ( 4, 2, 2, 2, 2, 2, 2, 4 ),
 ( 0.0007527720032349511205, 0.001260609959331164412, 0.001768447915427377812, 0.002022366893475485271, 0.002276285871523592731, 0.002784123827619805047, 0.003799799739812229678, 0.004815475652004653877 ),
 .UNSPECIFIED. ) ;
#21859 = CIRCLE ( 'NONE', #113786, 0.1000000000000000472 ) ;
#21860 = ORIENTED_EDGE ( 'NONE', *, *, #80782, .F. ) ;
#21861 = CIRCLE ( 'NONE', #115921, 0.06509327318403745899 ) ;
#21862 = CARTESIAN_POINT ( 'NONE',  ( -11.25000000000000000, 12.50000000000000000, -2.857883832488649745 ) ) ;
#21863 = LINE ( 'NONE', #91875, #81556 ) ;
#21864 = CARTESIAN_POINT ( 'NONE',  ( 186.5885416670080872, -6.551208109652273848, -3.782341765625003571 ) ) ;
#21865 = DIRECTION ( 'NONE',  ( 0.000000000000000000, -0.000000000000000000, 1.000000000000000000 ) ) ;
#21866 = DIRECTION ( 'NONE',  ( 0.000000000000000000, -0.9999939076577903929, 0.003490651415223739937 ) ) ;
#21867 = CARTESIAN_POINT ( 'NONE',  ( -6.450000000000017941, 12.50000000000000000, -2.511473670974877948 ) ) ;
#21868 = DIRECTION ( 'NONE',  ( 0.000000000000000000, 0.000000000000000000, 1.000000000000000000 ) ) ;
#21869 = VERTEX_POINT ( 'NONE', #72983 ) ;
#21870 = DIRECTION ( 'NONE',  ( 0.000000000000000000, -0.9999939076577903929, 0.003490651415223739937 ) ) ;
#21872 = DIRECTION ( 'NONE',  ( 0.000000000000000000, 0.000000000000000000, 1.000000000000000000 ) ) ;
#21871 = AXIS2_PLACEMENT_3D ( 'NONE', #72056, #9258, #100837 ) ;
#21873 = CARTESIAN_POINT ( 'NONE',  ( -2.100000000000033396, 2.500000000000000000, -3.637306695894650055 ) ) ;
#21874 = VERTEX_POINT ( 'NONE', #11481 ) ;
#21875 = CONICAL_SURFACE ( 'NONE', #38509, 0.09999999999999982514, 0.003490658503988666988 ) ;
#21876 = AXIS2_PLACEMENT_3D ( 'NONE', #16106, #113697, #44962 ) ;
#21877 = EDGE_LOOP ( 'NONE', ( #64366, #105342, #115452, #105886 ) ) ;
#21878 = DIRECTION ( 'NONE',  ( 0.000000000000000000, 1.000000000000000000, 0.000000000000000000 ) ) ;
#21879 = CIRCLE ( 'NONE', #53180, 0.09999999999999982514 ) ;
#21880 = ADVANCED_FACE ( 'NONE', ( #110950 ), #112909, .T. ) ;
#21881 = EDGE_LOOP ( 'NONE', ( #83600, #89718, #59508, #126763 ) ) ;
#21882 = AXIS2_PLACEMENT_3D ( 'NONE', #125949, #73626, #74933 ) ;
#21883 = ORIENTED_EDGE ( 'NONE', *, *, #83616, .F. ) ;
#21884 = DIRECTION ( 'NONE',  ( 0.000000000000000000, -0.9999939076577903929, 0.003490651415223739937 ) ) ;
#21885 = CIRCLE ( 'NONE', #99246, 0.06509327318403745899 ) ;
#21886 = ORIENTED_EDGE ( 'NONE', *, *, #62030, .T. ) ;
#21887 = CARTESIAN_POINT ( 'NONE',  ( -2.300000000000032685, 12.50000000000000000, -0.4115034346978157509 ) ) ;
#21888 = CARTESIAN_POINT ( 'NONE',  ( -8.750000000000005329, 2.500000000000000000, 5.802370205355744659 ) ) ;
#21889 = CARTESIAN_POINT ( 'NONE',  ( 15.86953761860679712, 2.463355995079644867, 3.896699429477471721 ) ) ;
#21890 = ORIENTED_EDGE ( 'NONE', *, *, #71847, .F. ) ;
#21891 = VECTOR ( 'NONE', #94898, 1000.000000000000000 ) ;
#21892 = AXIS2_PLACEMENT_3D ( 'NONE', #90303, #100767, #30781 ) ;
#21893 = DIRECTION ( 'NONE',  ( 0.000000000000000000, 0.000000000000000000, -1.000000000000000000 ) ) ;
#21894 = CARTESIAN_POINT ( 'NONE',  ( -1.900000000000034106, 12.50000000000000000, -4.048810130592463530 ) ) ;
#21895 = AXIS2_PLACEMENT_3D ( 'NONE', #107133, #15528, #55477 ) ;
#21896 = EDGE_CURVE ( 'NONE', #97929, #93847, #21294, .T. ) ;
#21897 = EDGE_LOOP ( 'NONE', ( #16917, #109032, #124745, #58583 ) ) ;
#21898 = EDGE_LOOP ( 'NONE', ( #32560, #44025 ) ) ;
#21899 = ORIENTED_EDGE ( 'NONE', *, *, #26968, .T. ) ;
#21900 = CARTESIAN_POINT ( 'NONE',  ( 0.3999999999999559464, 12.50000000000000000, -4.330127018922201643 ) ) ;
#21901 = PLANE ( 'NONE',  #1929 ) ;
#21902 = CARTESIAN_POINT ( 'NONE',  ( 5.849999999999933920, 12.50000000000000000, 5.802370205355744659 ) ) ;
#21903 = FACE_BOUND ( 'NONE', #24417, .T. ) ;
#21904 = ORIENTED_EDGE ( 'NONE', *, *, #15276, .T. ) ;
#21905 = CARTESIAN_POINT ( 'NONE',  ( -6.250000000000021316, 2.500000000000000000, -5.902370205355750521 ) ) ;
#21906 = DIRECTION ( 'NONE',  ( 1.000000000000000000, -0.000000000000000000, -0.000000000000000000 ) ) ;
#21907 = VECTOR ( 'NONE', #110985, 1000.000000000000000 ) ;
#21908 = VERTEX_POINT ( 'NONE', #120789 ) ;
#21909 = CARTESIAN_POINT ( 'NONE',  ( 8.949999999999917577, 12.50000000000000000, -2.511473670974877948 ) ) ;
#21910 = DIRECTION ( 'NONE',  ( -0.000000000000000000, -1.000000000000000000, -0.000000000000000000 ) ) ;
#21911 = LINE ( 'NONE', #12068, #115462 ) ;
#21912 = DIRECTION ( 'NONE',  ( -0.000000000000000000, -1.000000000000000000, -0.000000000000000000 ) ) ;
#21913 = CARTESIAN_POINT ( 'NONE',  ( -8.750000000000010658, 2.500000000000000000, -7.088010851410848190 ) ) ;
#21914 = DIRECTION ( 'NONE',  ( 0.000000000000000000, 0.000000000000000000, 1.000000000000000000 ) ) ;
#21915 = DIRECTION ( 'NONE',  ( 0.000000000000000000, 0.000000000000000000, 1.000000000000000000 ) ) ;
#21916 = CIRCLE ( 'NONE', #97118, 0.06509327318403741736 ) ;
#21917 = EDGE_CURVE ( 'NONE', #108081, #18231, #846, .T. ) ;
#21918 = ORIENTED_EDGE ( 'NONE', *, *, #4313, .F. ) ;
#21919 = EDGE_LOOP ( 'NONE', ( #34325, #57345 ) ) ;
#21920 = ORIENTED_EDGE ( 'NONE', *, *, #76289, .T. ) ;
#21921 = ORIENTED_EDGE ( 'NONE', *, *, #127946, .F. ) ;
#21922 = PLANE ( 'NONE',  #128973 ) ;
#21923 = DIRECTION ( 'NONE',  ( -0.000000000000000000, 1.000000000000000000, -0.000000000000000000 ) ) ;
#21924 = ORIENTED_EDGE ( 'NONE', *, *, #77270, .T. ) ;
#21925 = FACE_BOUND ( 'NONE', #124769, .T. ) ;
#21926 = ADVANCED_FACE ( 'NONE', ( #32443 ), #23225, .T. ) ;
#21927 = CARTESIAN_POINT ( 'NONE',  ( -13.09999999999999254, 12.50000000000000000, 0.4115034346978151958 ) ) ;
#21928 = DIRECTION ( 'NONE',  ( -0.000000000000000000, 1.000000000000000000, -0.000000000000000000 ) ) ;
#21929 = CIRCLE ( 'NONE', #80419, 0.09999999999999999167 ) ;
#21930 = DIRECTION ( 'NONE',  ( 0.000000000000000000, 0.000000000000000000, 1.000000000000000000 ) ) ;
#21931 = CARTESIAN_POINT ( 'NONE',  ( -9.600000000000008527, 12.50000000000000000, -5.088040615133786915 ) ) ;
#21932 = VECTOR ( 'NONE', #7230, 1000.000000000000000 ) ;
#21933 = DIRECTION ( 'NONE',  ( -0.000000000000000000, 1.000000000000000000, -0.000000000000000000 ) ) ;
#21934 = EDGE_CURVE ( 'NONE', #702, #78294, #101160, .T. ) ;
#21935 = DIRECTION ( 'NONE',  ( -0.000000000000000000, -1.000000000000000000, -0.000000000000000000 ) ) ;
#21936 = EDGE_CURVE ( 'NONE', #72308, #48106, #91332, .T. ) ;
#21937 = LINE ( 'NONE', #62509, #39187 ) ;
#21938 = CARTESIAN_POINT ( 'NONE',  ( 13.94999999999989271, 2.500000000000000000, -1.918653347947326004 ) ) ;
#21939 = EDGE_CURVE ( 'NONE', #106700, #100735, #94939, .T. ) ;
#21940 = DIRECTION ( 'NONE',  ( -0.000000000000000000, -1.000000000000000000, -0.000000000000000000 ) ) ;
#21941 = EDGE_CURVE ( 'NONE', #67379, #46379, #25885, .T. ) ;
#21942 = ORIENTED_EDGE ( 'NONE', *, *, #79466, .T. ) ;
#21943 = EDGE_CURVE ( 'NONE', #112402, #111058, #87780, .T. ) ;
#21944 = VERTEX_POINT ( 'NONE', #27566 ) ;
#21945 = AXIS2_PLACEMENT_3D ( 'NONE', #20275, #110585, #14768 ) ;
#21946 = ORIENTED_EDGE ( 'NONE', *, *, #110607, .T. ) ;
#21947 = VERTEX_POINT ( 'NONE', #35642 ) ;
#21948 = VECTOR ( 'NONE', #98519, 1000.000000000000000 ) ;
#21949 = ORIENTED_EDGE ( 'NONE', *, *, #101012, .F. ) ;
#21950 = ORIENTED_EDGE ( 'NONE', *, *, #83749, .T. ) ;
#21951 = ORIENTED_EDGE ( 'NONE', *, *, #46811, .F. ) ;
#21952 = CARTESIAN_POINT ( 'NONE',  ( 9.799999999999913669, 12.50000000000000000, 4.611443907251934426 ) ) ;
#21953 = VECTOR ( 'NONE', #4343, 1000.000000000000000 ) ;
#21954 = ORIENTED_EDGE ( 'NONE', *, *, #46216, .F. ) ;
#21955 = EDGE_CURVE ( 'NONE', #37658, #87328, #90735, .T. ) ;
#21956 = VERTEX_POINT ( 'NONE', #53989 ) ;
#21957 = CIRCLE ( 'NONE', #5190, 0.06509327318403745899 ) ;
#21958 = ADVANCED_FACE ( 'NONE', ( #14041 ), #76066, .T. ) ;
#21959 = ADVANCED_FACE ( 'NONE', ( #14681 ), #19630, .T. ) ;
#21960 = DIRECTION ( 'NONE',  ( -0.000000000000000000, 1.000000000000000000, -0.000000000000000000 ) ) ;
#21961 = CARTESIAN_POINT ( 'NONE',  ( 14.93723468939153420, -2.500000000000000444, 6.174425106950333308 ) ) ;
#21962 = DIRECTION ( 'NONE',  ( -0.000000000000000000, 1.000000000000000000, -0.000000000000000000 ) ) ;
#21963 = CARTESIAN_POINT ( 'NONE',  ( 9.149999999999918643, 2.500000000000000000, -6.595190528383302109 ) ) ;
#21964 = ORIENTED_EDGE ( 'NONE', *, *, #61010, .T. ) ;
#21965 = DIRECTION ( 'NONE',  ( -0.000000000000000000, -1.000000000000000000, -0.000000000000000000 ) ) ;
#21966 = VERTEX_POINT ( 'NONE', #93916 ) ;
#21968 = ORIENTED_EDGE ( 'NONE', *, *, #106467, .F. ) ;
#21967 = CONICAL_SURFACE ( 'NONE', #72124, 0.09999999999999982514, 0.003490658503988666988 ) ;
#21969 = DIRECTION ( 'NONE',  ( 0.000000000000000000, -0.9999939076577903929, 0.003490651415223739937 ) ) ;
#21970 = CIRCLE ( 'NONE', #7259, 0.06509327318403745899 ) ;
#21971 = CIRCLE ( 'NONE', #47098, 4.000000000000000000 ) ;
#21972 = DIRECTION ( 'NONE',  ( 0.000000000000000000, 0.000000000000000000, 1.000000000000000000 ) ) ;
#21973 = ORIENTED_EDGE ( 'NONE', *, *, #98410, .F. ) ;
#21974 = EDGE_LOOP ( 'NONE', ( #72200, #97243, #128332, #42716 ) ) ;
#21975 = CARTESIAN_POINT ( 'NONE',  ( -8.350000000000013856, 12.50000000000000000, -7.122917578226811486 ) ) ;
#21976 = AXIS2_PLACEMENT_3D ( 'NONE', #105184, #44995, #26632 ) ;
#21977 = CONICAL_SURFACE ( 'NONE', #105585, 0.1000000000000002554, 0.003490658503988666988 ) ;
#21978 = VECTOR ( 'NONE', #77503, 1000.000000000000000 ) ;
#21979 = DIRECTION ( 'NONE',  ( 0.000000000000000000, -0.000000000000000000, 1.000000000000000000 ) ) ;
#21980 = DIRECTION ( 'NONE',  ( 0.000000000000000000, 1.000000000000000000, 0.000000000000000000 ) ) ;
#21981 = CARTESIAN_POINT ( 'NONE',  ( 3.749999999999944045, 2.500000000000000000, -7.288010851410854585 ) ) ;
#21982 = ADVANCED_FACE ( 'NONE', ( #67482 ), #88673, .T. ) ;
#21983 = CIRCLE ( 'NONE', #74192, 0.06509327318403745899 ) ;
#21984 = DIRECTION ( 'NONE',  ( 0.000000000000000000, 0.000000000000000000, 1.000000000000000000 ) ) ;
#21985 = EDGE_LOOP ( 'NONE', ( #44848, #33587, #24089, #125288 ) ) ;
#21986 = DIRECTION ( 'NONE',  ( 0.000000000000000000, 0.000000000000000000, -1.000000000000000000 ) ) ;
#21987 = AXIS2_PLACEMENT_3D ( 'NONE', #75107, #74462, #3787 ) ;
#21988 = CIRCLE ( 'NONE', #82614, 0.06509327318403745899 ) ;
#21989 = ORIENTED_EDGE ( 'NONE', *, *, #110150, .T. ) ;
#21990 = DIRECTION ( 'NONE',  ( -0.000000000000000000, -1.000000000000000000, -0.000000000000000000 ) ) ;
#21991 = DIRECTION ( 'NONE',  ( 0.000000000000000000, 1.000000000000000000, 0.000000000000000000 ) ) ;
#21992 = FACE_OUTER_BOUND ( 'NONE', #3260, .T. ) ;
#21993 = CIRCLE ( 'NONE', #11506, 0.06509327318403745899 ) ;
#21994 = CARTESIAN_POINT ( 'NONE',  ( -7.499999999999976907, 12.50000000000000000, 4.330127018922196314 ) ) ;
#21995 = EDGE_CURVE ( 'NONE', #128788, #22282, #11307, .T. ) ;
#21996 = CARTESIAN_POINT ( 'NONE',  ( -15.59999999999998010, 2.500000000000000000, -0.3464101615137759604 ) ) ;
#21997 = VERTEX_POINT ( 'NONE', #55280 ) ;
#21998 = EDGE_CURVE ( 'NONE', #17511, #101710, #107436, .T. ) ;
#21999 = CARTESIAN_POINT ( 'NONE',  ( 9.799999999999918998, 2.500000000000000000, -0.2464101615137782308 ) ) ;
#22000 = EDGE_CURVE ( 'NONE', #106597, #7810, #111670, .T. ) ;
#22001 = LINE ( 'NONE', #90716, #113438 ) ;
#22002 = ORIENTED_EDGE ( 'NONE', *, *, #105094, .F. ) ;
#22003 = ORIENTED_EDGE ( 'NONE', *, *, #63743, .F. ) ;
#22004 = EDGE_LOOP ( 'NONE', ( #53366, #14114, #110571, #14884 ) ) ;
#22005 = DIRECTION ( 'NONE',  ( 0.000000000000000000, 1.000000000000000000, 0.000000000000000000 ) ) ;
#22006 = FACE_OUTER_BOUND ( 'NONE', #102096, .T. ) ;
#22007 = CARTESIAN_POINT ( 'NONE',  ( 187.5000000000000000, 0.000000000000000000, 0.000000000000000000 ) ) ;
#22008 = CIRCLE ( 'NONE', #63756, 0.09999999999999982514 ) ;
#22009 = CARTESIAN_POINT ( 'NONE',  ( 3.949999999999938893, 2.500000000000000000, 6.248780366869520542 ) ) ;
#22010 = EDGE_CURVE ( 'NONE', #42781, #125134, #74920, .T. ) ;
#22011 = DIRECTION ( 'NONE',  ( 0.000000000000000000, 0.000000000000000000, 1.000000000000000000 ) ) ;
#22012 = CARTESIAN_POINT ( 'NONE',  ( -13.09999999999999254, 12.50000000000000000, -0.3464101615137741286 ) ) ;
#22013 = DIRECTION ( 'NONE',  ( 0.000000000000000000, -0.9999939076577903929, 0.003490651415223739937 ) ) ;
#22014 = CARTESIAN_POINT ( 'NONE',  ( -2.050000000000032685, 2.500000000000000000, -6.495190528383302464 ) ) ;
#22015 = AXIS2_PLACEMENT_3D ( 'NONE', #92427, #2753, #40116 ) ;
#22016 = CIRCLE ( 'NONE', #128546, 0.06509327318403745899 ) ;
#22017 = ORIENTED_EDGE ( 'NONE', *, *, #2145, .T. ) ;
#22018 = DIRECTION ( 'NONE',  ( 0.000000000000000000, 0.000000000000000000, -1.000000000000000000 ) ) ;
#22019 = CARTESIAN_POINT ( 'NONE',  ( 2.699999999999947331, 2.500000000000000000, -4.676537180435978769 ) ) ;
#22020 = EDGE_CURVE ( 'NONE', #55645, #12624, #105401, .T. ) ;
#22021 = CARTESIAN_POINT ( 'NONE',  ( 4.999999999999933387, 2.500000000000000000, 5.022947341949748790 ) ) ;
#22022 = CARTESIAN_POINT ( 'NONE',  ( 0.5999999999999555689, 2.500000000000000000, 4.676537180435972552 ) ) ;
#22023 = ORIENTED_EDGE ( 'NONE', *, *, #97778, .F. ) ;
#22024 = DIRECTION ( 'NONE',  ( -4.274815082592931898E-19, -0.9999939076577903929, -0.003490651415223739937 ) ) ;
#22025 = AXIS2_PLACEMENT_3D ( 'NONE', #127636, #16366, #66771 ) ;
#22026 = AXIS2_PLACEMENT_3D ( 'NONE', #64723, #56188, #123633 ) ;
#22027 = CARTESIAN_POINT ( 'NONE',  ( -10.45000000000000107, 2.500000000000000000, 2.265063509461097357 ) ) ;
#22029 = ORIENTED_EDGE ( 'NONE', *, *, #98310, .F. ) ;
#22028 = CARTESIAN_POINT ( 'NONE',  ( 0.000000000000000000, 2.500000000000000000, 0.000000000000000000 ) ) ;
#22030 = ORIENTED_EDGE ( 'NONE', *, *, #69193, .T. ) ;
#22031 = FACE_OUTER_BOUND ( 'NONE', #84302, .T. ) ;
#22032 = CONICAL_SURFACE ( 'NONE', #3243, 0.09999999999999982514, 0.003490658503988666988 ) ;
#22033 = AXIS2_PLACEMENT_3D ( 'NONE', #6750, #84046, #15293 ) ;
#22034 = ADVANCED_FACE ( 'NONE', ( #47887 ), #124009, .T. ) ;
#22035 = EDGE_LOOP ( 'NONE', ( #112711, #105125, #24153, #53753 ) ) ;
#22036 = VERTEX_POINT ( 'NONE', #127716 ) ;
#22037 = CARTESIAN_POINT ( 'NONE',  ( 11.44999999999990692, 2.500000000000000000, -6.841600689897078702 ) ) ;
#22038 = EDGE_CURVE ( 'NONE', #125864, #88124, #38057, .T. ) ;
#22039 = DIRECTION ( 'NONE',  ( 0.000000000000000000, 1.000000000000000000, 0.000000000000000000 ) ) ;
#22040 = DIRECTION ( 'NONE',  ( 0.000000000000000000, 0.000000000000000000, -1.000000000000000000 ) ) ;
#22041 = LINE ( 'NONE', #121490, #62562 ) ;
#22042 = ORIENTED_EDGE ( 'NONE', *, *, #28444, .T. ) ;
#22043 = CIRCLE ( 'NONE', #111913, 0.1000000000000002554 ) ;
#22044 = CARTESIAN_POINT ( 'NONE',  ( -4.350000000000023626, 12.50000000000000000, 1.818653347947321475 ) ) ;
#22045 = ORIENTED_EDGE ( 'NONE', *, *, #39691, .T. ) ;
#22046 = CARTESIAN_POINT ( 'NONE',  ( 17.50000000000011013, 2.262036863575971335, 3.993716676843428015 ) ) ;
#22047 = EDGE_CURVE ( 'NONE', #29184, #121009, #23837, .T. ) ;
#22048 = CARTESIAN_POINT ( 'NONE',  ( -6.250000000000019540, 2.500000000000000000, -2.957883832488653830 ) ) ;
#22049 = CIRCLE ( 'NONE', #99311, 0.1000000000000002554 ) ;
#22050 = ORIENTED_EDGE ( 'NONE', *, *, #72344, .T. ) ;
#22051 = CIRCLE ( 'NONE', #57551, 0.06509327318403745899 ) ;
#22052 = ORIENTED_EDGE ( 'NONE', *, *, #119170, .T. ) ;
#22053 = AXIS2_PLACEMENT_3D ( 'NONE', #65765, #6824, #24563 ) ;
#22054 = ORIENTED_EDGE ( 'NONE', *, *, #36591, .F. ) ;
#22055 = EDGE_LOOP ( 'NONE', ( #21756, #59529, #23883, #78552 ) ) ;
#22056 = CARTESIAN_POINT ( 'NONE',  ( -9.600000000000008527, 12.50000000000000000, -0.06509327318403980434 ) ) ;
#22057 = CARTESIAN_POINT ( 'NONE',  ( 15.40585131749456949, 2.500000000000000000, 5.817868756320654811 ) ) ;
#22058 = DIRECTION ( 'NONE',  ( 0.000000000000000000, 0.000000000000000000, 1.000000000000000000 ) ) ;
#22059 = FACE_BOUND ( 'NONE', #63542, .T. ) ;
#22060 = ORIENTED_EDGE ( 'NONE', *, *, #50028, .F. ) ;
#22061 = DIRECTION ( 'NONE',  ( 0.000000000000000000, -0.000000000000000000, 1.000000000000000000 ) ) ;
#22062 = CARTESIAN_POINT ( 'NONE',  ( 183.9479166673494603, -6.668395609140176816, -3.850000000000003642 ) ) ;
#22063 = CARTESIAN_POINT ( 'NONE',  ( -11.84999999999999787, 12.50000000000000000, -1.818653347947321919 ) ) ;
#22064 = CARTESIAN_POINT ( 'NONE',  ( 12.49999999999993605, 2.500000000000000000, -2.276824562219559311E-15 ) ) ;
#22065 = AXIS2_PLACEMENT_3D ( 'NONE', #74138, #4090, #23098 ) ;
#22066 = AXIS2_PLACEMENT_3D ( 'NONE', #17568, #108541, #50273 ) ;
#22067 = CONICAL_SURFACE ( 'NONE', #19915, 0.1000000000000000472, 0.003490658503988666988 ) ;
#22068 = CARTESIAN_POINT ( 'NONE',  ( -12.49999999999999289, 2.500000000000000000, 4.922947341949748257 ) ) ;
#22069 = CONICAL_SURFACE ( 'NONE', #7365, 0.1000000000000000472, 0.003490658503988666988 ) ;
#22070 = DIRECTION ( 'NONE',  ( -0.000000000000000000, -1.000000000000000000, -0.000000000000000000 ) ) ;
#22071 = FACE_OUTER_BOUND ( 'NONE', #1001, .T. ) ;
#22072 = CIRCLE ( 'NONE', #76437, 0.06509327318403745899 ) ;
#22073 = DIRECTION ( 'NONE',  ( -0.000000000000000000, 1.000000000000000000, -0.000000000000000000 ) ) ;
#22075 = ADVANCED_FACE ( 'NONE', ( #58356 ), #59159, .T. ) ;
#22074 = AXIS2_PLACEMENT_3D ( 'NONE', #76849, #127869, #97768 ) ;
#22076 = ORIENTED_EDGE ( 'NONE', *, *, #30499, .F. ) ;
#22077 = ORIENTED_EDGE ( 'NONE', *, *, #50450, .T. ) ;
#22078 = EDGE_LOOP ( 'NONE', ( #69342, #29103 ) ) ;
#22079 = EDGE_LOOP ( 'NONE', ( #52472, #35518, #97164, #109649 ) ) ;
#22080 = ORIENTED_EDGE ( 'NONE', *, *, #114243, .F. ) ;
#22081 = DIRECTION ( 'NONE',  ( -0.000000000000000000, 1.000000000000000000, -0.000000000000000000 ) ) ;
#22082 = PLANE ( 'NONE',  #17327 ) ;
#22083 = ORIENTED_EDGE ( 'NONE', *, *, #48287, .F. ) ;
#22084 = FACE_BOUND ( 'NONE', #93430, .T. ) ;
#22085 = DIRECTION ( 'NONE',  ( -0.000000000000000000, -1.000000000000000000, -0.000000000000000000 ) ) ;
#22086 = ADVANCED_FACE ( 'NONE', ( #28240 ), #68145, .T. ) ;
#22087 = ORIENTED_EDGE ( 'NONE', *, *, #16900, .T. ) ;
#22088 = EDGE_CURVE ( 'NONE', #77067, #51687, #113548, .T. ) ;
#22089 = DIRECTION ( 'NONE',  ( -4.274815082592931898E-19, -0.9999939076577903929, -0.003490651415223739937 ) ) ;
#22090 = ADVANCED_FACE ( 'NONE', ( #30185 ), #103049, .T. ) ;
#22091 = DIRECTION ( 'NONE',  ( -0.000000000000000000, -1.000000000000000000, -0.000000000000000000 ) ) ;
#22092 = EDGE_CURVE ( 'NONE', #110447, #89399, #23629, .T. ) ;
#22093 = DIRECTION ( 'NONE',  ( 0.000000000000000000, 0.000000000000000000, 1.000000000000000000 ) ) ;
#22094 = EDGE_CURVE ( 'NONE', #72573, #36539, #75852, .T. ) ;
#22096 = VERTEX_POINT ( 'NONE', #31465 ) ;
#22095 = CIRCLE ( 'NONE', #95245, 0.06509327318403745899 ) ;
#22097 = DIRECTION ( 'NONE',  ( -0.000000000000000000, 1.000000000000000000, -0.000000000000000000 ) ) ;
#22098 = ORIENTED_EDGE ( 'NONE', *, *, #47377, .F. ) ;
#22099 = VERTEX_POINT ( 'NONE', #1342 ) ;
#22100 = ADVANCED_FACE ( 'NONE', ( #21640 ), #27828, .T. ) ;
#22101 = ORIENTED_EDGE ( 'NONE', *, *, #96858, .T. ) ;
#22102 = FACE_OUTER_BOUND ( 'NONE', #72278, .T. ) ;
#22103 = ADVANCED_FACE ( 'NONE', ( #99566 ), #115549, .T. ) ;
#22104 = DIRECTION ( 'NONE',  ( 0.000000000000000000, 0.000000000000000000, 1.000000000000000000 ) ) ;
#22105 = CIRCLE ( 'NONE', #97300, 0.1000000000000002554 ) ;
#22106 = ORIENTED_EDGE ( 'NONE', *, *, #18236, .F. ) ;
#22107 = ADVANCED_FACE ( 'NONE', ( #11159 ), #6876, .T. ) ;
#22108 = DIRECTION ( 'NONE',  ( -4.274815082592931898E-19, -0.9999939076577903929, -0.003490651415223739937 ) ) ;
#22109 = AXIS2_PLACEMENT_3D ( 'NONE', #129174, #28375, #79413 ) ;
#22110 = AXIS2_PLACEMENT_3D ( 'NONE', #25250, #65173, #64547 ) ;
#22111 = ADVANCED_FACE ( 'NONE', ( #108719 ), #11093, .T. ) ;
#22112 = CARTESIAN_POINT ( 'NONE',  ( 10.64999999999991331, 2.500000000000000000, -2.511473670974877948 ) ) ;
#22113 = EDGE_CURVE ( 'NONE', #103547, #30982, #119833, .T. ) ;
#22114 = DIRECTION ( 'NONE',  ( 0.000000000000000000, 0.000000000000000000, 1.000000000000000000 ) ) ;
#22115 = CARTESIAN_POINT ( 'NONE',  ( 10.44999999999991402, 12.50000000000000000, 6.495190528383297135 ) ) ;
#22116 = CARTESIAN_POINT ( 'NONE',  ( 185.9062500006828316, -8.891194145520236347, -1.633285867636356693E-15 ) ) ;
#22117 = ORIENTED_EDGE ( 'NONE', *, *, #2864, .F. ) ;
#22118 = CARTESIAN_POINT ( 'NONE',  ( -7.500000000000001776, 1.500000000000000000, 1.734723475976807094E-15 ) ) ;
#22119 = EDGE_CURVE ( 'NONE', #41869, #7747, #49827, .T. ) ;
#22120 = ORIENTED_EDGE ( 'NONE', *, *, #114538, .F. ) ;
#22121 = CARTESIAN_POINT ( 'NONE',  ( 11.44999999999991047, 2.500000000000000000, 6.148780366869520009 ) ) ;
#22122 = VECTOR ( 'NONE', #76608, 1000.000000000000000 ) ;
#22123 = ORIENTED_EDGE ( 'NONE', *, *, #48529, .T. ) ;
#22125 = DIRECTION ( 'NONE',  ( -0.000000000000000000, 1.000000000000000000, -0.000000000000000000 ) ) ;
#22124 = CIRCLE ( 'NONE', #19954, 0.06509327318403745899 ) ;
#22126 = ORIENTED_EDGE ( 'NONE', *, *, #46022, .T. ) ;
#22127 = DIRECTION ( 'NONE',  ( 0.000000000000000000, 0.000000000000000000, 1.000000000000000000 ) ) ;
#22128 = DIRECTION ( 'NONE',  ( -0.000000000000000000, -1.000000000000000000, -0.000000000000000000 ) ) ;
#22129 = DIRECTION ( 'NONE',  ( 0.000000000000000000, -0.000000000000000000, 1.000000000000000000 ) ) ;
#22130 = DIRECTION ( 'NONE',  ( 0.000000000000000000, 0.000000000000000000, 1.000000000000000000 ) ) ;
#22131 = PLANE ( 'NONE',  #24459 ) ;
#22132 = ORIENTED_EDGE ( 'NONE', *, *, #79002, .T. ) ;
#22133 = EDGE_LOOP ( 'NONE', ( #41049, #129067 ) ) ;
#22134 = DIRECTION ( 'NONE',  ( 0.000000000000000000, -0.000000000000000000, 1.000000000000000000 ) ) ;
#22135 = CIRCLE ( 'NONE', #107791, 0.06509327318403745899 ) ;
#22136 = VECTOR ( 'NONE', #104188, 1000.000000000000000 ) ;
#22137 = CARTESIAN_POINT ( 'NONE',  ( 9.399999999999918643, 2.500000000000000000, 0.4464101615137736623 ) ) ;
#22138 = DIRECTION ( 'NONE',  ( 0.000000000000000000, 0.000000000000000000, 1.000000000000000000 ) ) ;
#22140 = VERTEX_POINT ( 'NONE', #110655 ) ;
#22139 = EDGE_LOOP ( 'NONE', ( #57115, #111686 ) ) ;
#22141 = ORIENTED_EDGE ( 'NONE', *, *, #65149, .T. ) ;
#22142 = CARTESIAN_POINT ( 'NONE',  ( 3.149999999999942624, 12.50000000000000000, 6.841600689897072485 ) ) ;
#22143 = EDGE_LOOP ( 'NONE', ( #60107, #33101, #66086, #84375 ) ) ;
#22144 = DIRECTION ( 'NONE',  ( 0.000000000000000000, 0.000000000000000000, 1.000000000000000000 ) ) ;
#22145 = DIRECTION ( 'NONE',  ( -0.000000000000000000, -1.000000000000000000, -0.000000000000000000 ) ) ;
#22146 = LINE ( 'NONE', #41787, #86603 ) ;
#22147 = ORIENTED_EDGE ( 'NONE', *, *, #41477, .F. ) ;
#22148 = CARTESIAN_POINT ( 'NONE',  ( -11.05000000000000071, 12.50000000000000000, 6.841600689897072485 ) ) ;
#22149 = DIRECTION ( 'NONE',  ( 0.000000000000000000, 0.000000000000000000, 1.000000000000000000 ) ) ;
#22150 = CARTESIAN_POINT ( 'NONE',  ( -6.650000000000015454, 2.500000000000000000, 2.857883832488649301 ) ) ;
#22151 = FACE_OUTER_BOUND ( 'NONE', #9147, .T. ) ;
#22152 = DIRECTION ( 'NONE',  ( -0.000000000000000000, 1.000000000000000000, -0.000000000000000000 ) ) ;
#22153 = ORIENTED_EDGE ( 'NONE', *, *, #62853, .T. ) ;
#22154 = ADVANCED_FACE ( 'NONE', ( #111279 ), #19414, .T. ) ;
#22155 = CARTESIAN_POINT ( 'NONE',  ( 4.199999999999941558, 2.500000000000000000, -4.430127018922202176 ) ) ;
#22156 = AXIS2_PLACEMENT_3D ( 'NONE', #23062, #92438, #91801 ) ;
#22157 = VECTOR ( 'NONE', #90565, 1000.000000000000000 ) ;
#22159 = ADVANCED_FACE ( 'NONE', ( #79911 ), #81211, .T. ) ;
#22158 = FACE_OUTER_BOUND ( 'NONE', #81583, .T. ) ;
#22160 = EDGE_LOOP ( 'NONE', ( #83291, #83022, #84538, #101307 ) ) ;
#22161 = VERTEX_POINT ( 'NONE', #89093 ) ;
#22162 = CARTESIAN_POINT ( 'NONE',  ( 184.2760416670080588, 6.551208109652274736, 3.782341765625001351 ) ) ;
#22163 = DIRECTION ( 'NONE',  ( 0.000000000000000000, -0.9999939076577903929, 0.003490651415223739937 ) ) ;
#22164 = CARTESIAN_POINT ( 'NONE',  ( 6.699999999999928235, 2.500000000000000000, -2.276824562219559311E-15 ) ) ;
#22165 = FACE_OUTER_BOUND ( 'NONE', #124957, .T. ) ;
#22166 = ADVANCED_FACE ( 'NONE', ( #118535 ), #73800, .T. ) ;
#22167 = CARTESIAN_POINT ( 'NONE',  ( -10.65000000000000213, 2.500000000000000000, 2.511473670974873507 ) ) ;
#22168 = EDGE_CURVE ( 'NONE', #118189, #39604, #100822, .T. ) ;
#22169 = DIRECTION ( 'NONE',  ( 0.000000000000000000, 0.000000000000000000, 1.000000000000000000 ) ) ;
#22170 = CARTESIAN_POINT ( 'NONE',  ( 1.899999999999951283, 12.50000000000000000, -0.2813168883297408329 ) ) ;
#22171 = LINE ( 'NONE', #42444, #120906 ) ;
#22172 = CIRCLE ( 'NONE', #9619, 0.06509327318403745899 ) ;
#22173 = CARTESIAN_POINT ( 'NONE',  ( -0.8500000000000390576, 2.500000000000000000, -2.165063509461101710 ) ) ;
#22174 = AXIS2_PLACEMENT_3D ( 'NONE', #101685, #121316, #19232 ) ;
#22175 = AXIS2_PLACEMENT_3D ( 'NONE', #1948, #22271, #91630 ) ;
#22176 = EDGE_LOOP ( 'NONE', ( #74624, #16150 ) ) ;
#22177 = ORIENTED_EDGE ( 'NONE', *, *, #44319, .F. ) ;
#22178 = ORIENTED_EDGE ( 'NONE', *, *, #50281, .F. ) ;
#22179 = CONICAL_SURFACE ( 'NONE', #95315, 0.1000000000000002554, 0.003490658503988666988 ) ;
#22180 = VERTEX_POINT ( 'NONE', #29529 ) ;
#22181 = CARTESIAN_POINT ( 'NONE',  ( 5.199999999999937117, 2.500000000000000000, -4.776537180435978414 ) ) ;
#22182 = LINE ( 'NONE', #102639, #123136 ) ;
#22183 = EDGE_LOOP ( 'NONE', ( #51900, #121292 ) ) ;
#22184 = DIRECTION ( 'NONE',  ( -0.000000000000000000, -1.000000000000000000, -0.000000000000000000 ) ) ;
#22185 = PLANE ( 'NONE',  #101574 ) ;
#22187 = VERTEX_POINT ( 'NONE', #51113 ) ;
#22186 = CARTESIAN_POINT ( 'NONE',  ( 5.849999999999935696, 2.500000000000000000, -6.395190528383301931 ) ) ;
#22188 = FACE_OUTER_BOUND ( 'NONE', #28766, .T. ) ;
#22189 = CIRCLE ( 'NONE', #122518, 0.06509327318403745899 ) ;
#22190 = FACE_OUTER_BOUND ( 'NONE', #111692, .T. ) ;
#22191 = ADVANCED_FACE ( 'NONE', ( #39371 ), #36173, .T. ) ;
#22192 = EDGE_LOOP ( 'NONE', ( #35377, #96186, #95894, #3351 ) ) ;
#22193 = ORIENTED_EDGE ( 'NONE', *, *, #46305, .F. ) ;
#22194 = ORIENTED_EDGE ( 'NONE', *, *, #4265, .F. ) ;
#22195 = ORIENTED_EDGE ( 'NONE', *, *, #97283, .F. ) ;
#22196 = CARTESIAN_POINT ( 'NONE',  ( 1.849999999999949685, 2.500000000000000000, -2.511473670974877948 ) ) ;
#22197 = CIRCLE ( 'NONE', #38934, 0.06509327318403743123 ) ;
#22198 = AXIS2_PLACEMENT_3D ( 'NONE', #19817, #70200, #87881 ) ;
#22199 = CARTESIAN_POINT ( 'NONE',  ( 6.649999999999931966, 2.500000000000000000, -7.288010851410854585 ) ) ;
#22200 = CARTESIAN_POINT ( 'NONE',  ( 10.84999999999990905, 2.500000000000000000, 1.372243186433545370 ) ) ;
#22201 = EDGE_LOOP ( 'NONE', ( #46484, #112101 ) ) ;
#22202 = CIRCLE ( 'NONE', #95344, 0.1000000000000002554 ) ;
#22203 = DIRECTION ( 'NONE',  ( 0.000000000000000000, 0.000000000000000000, 1.000000000000000000 ) ) ;
#22205 = VERTEX_POINT ( 'NONE', #38732 ) ;
#22204 = EDGE_CURVE ( 'NONE', #124884, #20780, #59664, .T. ) ;
#22206 = DIRECTION ( 'NONE',  ( 0.000000000000000000, 1.000000000000000000, 0.000000000000000000 ) ) ;
#22207 = CARTESIAN_POINT ( 'NONE',  ( 3.677919667776838875, -2.499999999999999556, -8.999999999883526058 ) ) ;
#22208 = DIRECTION ( 'NONE',  ( -0.000000000000000000, -1.000000000000000000, -0.000000000000000000 ) ) ;
#22209 = DIRECTION ( 'NONE',  ( 0.000000000000000000, 0.000000000000000000, -1.000000000000000000 ) ) ;
#22210 = ADVANCED_FACE ( 'NONE', ( #78644 ), #119775, .T. ) ;
#22211 = AXIS2_PLACEMENT_3D ( 'NONE', #107845, #117638, #38488 ) ;
#22212 = VERTEX_POINT ( 'NONE', #13733 ) ;
#22214 = AXIS2_PLACEMENT_3D ( 'NONE', #121894, #34171, #114017 ) ;
#22213 = AXIS2_PLACEMENT_3D ( 'NONE', #10497, #100188, #91008 ) ;
#22215 = ORIENTED_EDGE ( 'NONE', *, *, #109575, .T. ) ;
#22216 = VERTEX_POINT ( 'NONE', #121760 ) ;
#22217 = DIRECTION ( 'NONE',  ( 0.000000000000000000, 0.000000000000000000, -1.000000000000000000 ) ) ;
#22218 = FACE_OUTER_BOUND ( 'NONE', #82196, .T. ) ;
#22219 = EDGE_CURVE ( 'NONE', #7581, #39960, #44565, .T. ) ;
#22220 = CARTESIAN_POINT ( 'NONE',  ( 1.849999999999948130, 2.500000000000000000, 6.148780366869520009 ) ) ;
#22221 = FACE_BOUND ( 'NONE', #82615, .T. ) ;
#22222 = CARTESIAN_POINT ( 'NONE',  ( 7.899999999999923084, 2.500000000000000000, -0.5928203230275542746 ) ) ;
#22223 = DIRECTION ( 'NONE',  ( 0.000000000000000000, 1.000000000000000000, 0.000000000000000000 ) ) ;
#22224 = CARTESIAN_POINT ( 'NONE',  ( -2.700000000000029932, 2.500000000000000000, -0.2464101615137782308 ) ) ;
#22225 = DIRECTION ( 'NONE',  ( 0.000000000000000000, -0.9999939076577903929, 0.003490651415223739937 ) ) ;
#22226 = FACE_OUTER_BOUND ( 'NONE', #71483, .T. ) ;
#22227 = DIRECTION ( 'NONE',  ( 0.000000000000000000, -0.000000000000000000, 1.000000000000000000 ) ) ;
#22228 = EDGE_LOOP ( 'NONE', ( #6153, #42495, #101289, #89419 ) ) ;
#22229 = FACE_OUTER_BOUND ( 'NONE', #45379, .T. ) ;
#22230 = DIRECTION ( 'NONE',  ( 0.000000000000000000, 0.000000000000000000, 1.000000000000000000 ) ) ;
#22231 = VERTEX_POINT ( 'NONE', #34703 ) ;
#22232 = ORIENTED_EDGE ( 'NONE', *, *, #66381, .F. ) ;
#22233 = FACE_OUTER_BOUND ( 'NONE', #76771, .T. ) ;
#22234 = FACE_OUTER_BOUND ( 'NONE', #118501, .T. ) ;
#22235 = FACE_BOUND ( 'NONE', #92804, .T. ) ;
#22236 = DIRECTION ( 'NONE',  ( -4.274815082592931898E-19, -0.9999939076577903929, -0.003490651415223739937 ) ) ;
#22237 = ADVANCED_FACE ( 'NONE', ( #92300 ), #111344, .T. ) ;
#22238 = VECTOR ( 'NONE', #85829, 1000.000000000000000 ) ;
#22239 = AXIS2_PLACEMENT_3D ( 'NONE', #56280, #44536, #64172 ) ;
#22240 = ORIENTED_EDGE ( 'NONE', *, *, #126017, .F. ) ;
#22241 = CARTESIAN_POINT ( 'NONE',  ( -14.59999999999998366, 2.500000000000000000, -0.1000000000000001166 ) ) ;
#22242 = ADVANCED_FACE ( 'NONE', ( #4537 ), #82131, .T. ) ;
#22243 = LINE ( 'NONE', #50391, #93775 ) ;
#22244 = EDGE_CURVE ( 'NONE', #98982, #122996, #38228, .T. ) ;
#22245 = EDGE_CURVE ( 'NONE', #71349, #24092, #1984, .T. ) ;
#22246 = ORIENTED_EDGE ( 'NONE', *, *, #85992, .T. ) ;
#22247 = DIRECTION ( 'NONE',  ( 0.000000000000000000, 1.000000000000000000, 0.000000000000000000 ) ) ;
#22248 = CARTESIAN_POINT ( 'NONE',  ( -3.150000000000030109, 12.50000000000000000, 1.883746621131358934 ) ) ;
#22250 = AXIS2_PLACEMENT_3D ( 'NONE', #118319, #48953, #116375 ) ;
#22249 = AXIS2_PLACEMENT_3D ( 'NONE', #84482, #123735, #22991 ) ;
#22251 = EDGE_CURVE ( 'NONE', #95698, #87872, #98838, .T. ) ;
#22252 = ORIENTED_EDGE ( 'NONE', *, *, #16265, .T. ) ;
#22253 = ADVANCED_FACE ( 'NONE', ( #32119 ), #64131, .T. ) ;
#22254 = DIRECTION ( 'NONE',  ( 0.000000000000000000, 1.000000000000000000, 0.000000000000000000 ) ) ;
#22255 = EDGE_CURVE ( 'NONE', #34595, #71534, #40377, .T. ) ;
#22256 = FACE_OUTER_BOUND ( 'NONE', #114472, .T. ) ;
#22258 = AXIS2_PLACEMENT_3D ( 'NONE', #122505, #51194, #32209 ) ;
#22257 = AXIS2_PLACEMENT_3D ( 'NONE', #13928, #104259, #102330 ) ;
#22259 = ORIENTED_EDGE ( 'NONE', *, *, #14243, .F. ) ;
#22260 = AXIS2_PLACEMENT_3D ( 'NONE', #108716, #9880, #49822 ) ;
#22261 = DIRECTION ( 'NONE',  ( 0.000000000000000000, 0.000000000000000000, 1.000000000000000000 ) ) ;
#22262 = EDGE_CURVE ( 'NONE', #126749, #18676, #51748, .T. ) ;
#22263 = LINE ( 'NONE', #79871, #26818 ) ;
#22264 = LINE ( 'NONE', #31427, #82822 ) ;
#22265 = EDGE_LOOP ( 'NONE', ( #35002, #33247 ) ) ;
#22266 = VERTEX_POINT ( 'NONE', #11808 ) ;
#22267 = ADVANCED_FACE ( 'NONE', ( #52384 ), #34105, .T. ) ;
#22268 = DIRECTION ( 'NONE',  ( -0.000000000000000000, 1.000000000000000000, -0.000000000000000000 ) ) ;
#22269 = EDGE_CURVE ( 'NONE', #99205, #52516, #17348, .T. ) ;
#22270 = ORIENTED_EDGE ( 'NONE', *, *, #88137, .F. ) ;
#22271 = DIRECTION ( 'NONE',  ( -0.000000000000000000, 1.000000000000000000, -0.000000000000000000 ) ) ;
#22272 = CARTESIAN_POINT ( 'NONE',  ( -8.350000000000010303, 12.50000000000000000, 6.430097255199259010 ) ) ;
#22273 = FACE_OUTER_BOUND ( 'NONE', #85958, .T. ) ;
#22274 = ORIENTED_EDGE ( 'NONE', *, *, #110853, .T. ) ;
#22275 = FACE_OUTER_BOUND ( 'NONE', #90452, .T. ) ;
#22276 = LINE ( 'NONE', #62199, #1727 ) ;
#22277 = CARTESIAN_POINT ( 'NONE',  ( -6.650000000000018119, 12.50000000000000000, -7.188010851410854052 ) ) ;
#22278 = DIRECTION ( 'NONE',  ( -0.000000000000000000, 1.000000000000000000, -0.000000000000000000 ) ) ;
#22279 = LINE ( 'NONE', #53648, #69581 ) ;
#22280 = AXIS2_PLACEMENT_3D ( 'NONE', #18209, #117682, #20804 ) ;
#22281 = CARTESIAN_POINT ( 'NONE',  ( 10.64999999999990976, 12.50000000000000000, 1.818653347947321475 ) ) ;
#22282 = VERTEX_POINT ( 'NONE', #122426 ) ;
#22283 = VERTEX_POINT ( 'NONE', #113225 ) ;
#22284 = DIRECTION ( 'NONE',  ( 0.000000000000000000, -0.000000000000000000, 1.000000000000000000 ) ) ;
#22285 = ORIENTED_EDGE ( 'NONE', *, *, #27456, .F. ) ;
#22286 = VECTOR ( 'NONE', #108312, 1000.000000000000000 ) ;
#22287 = CIRCLE ( 'NONE', #11794, 0.1000000000000002554 ) ;
#22288 = CARTESIAN_POINT ( 'NONE',  ( 103.0088460997482400, 7.694247472631703388, 0.3420374265531280211 ) ) ;
#22290 = VERTEX_POINT ( 'NONE', #14373 ) ;
#22289 = EDGE_LOOP ( 'NONE', ( #53525, #83470 ) ) ;
#22291 = AXIS2_PLACEMENT_3D ( 'NONE', #81016, #62026, #20806 ) ;
#22292 = ORIENTED_EDGE ( 'NONE', *, *, #34363, .F. ) ;
#22293 = DIRECTION ( 'NONE',  ( 0.000000000000000000, 0.000000000000000000, -1.000000000000000000 ) ) ;
#22294 = AXIS2_PLACEMENT_3D ( 'NONE', #53142, #3384, #22404 ) ;
#22295 = AXIS2_PLACEMENT_3D ( 'NONE', #8044, #127826, #38163 ) ;
#22296 = DIRECTION ( 'NONE',  ( 0.000000000000000000, -0.000000000000000000, 1.000000000000000000 ) ) ;
#22297 = DIRECTION ( 'NONE',  ( 0.000000000000000000, 0.000000000000000000, 1.000000000000000000 ) ) ;
#22298 = AXIS2_PLACEMENT_3D ( 'NONE', #77122, #115743, #27351 ) ;
#22299 =( NAMED_UNIT ( * ) PLANE_ANGLE_UNIT ( ) SI_UNIT ( $, .RADIAN. ) );
#22300 = PLANE ( 'NONE',  #101674 ) ;
#22301 = DIRECTION ( 'NONE',  ( 0.000000000000000000, 0.000000000000000000, -1.000000000000000000 ) ) ;
#22302 = DIRECTION ( 'NONE',  ( -4.274815082592931898E-19, -0.9999939076577903929, -0.003490651415223739937 ) ) ;
#22303 = CARTESIAN_POINT ( 'NONE',  ( -0.6000000000000388356, 12.50000000000000000, 4.048810130592458201 ) ) ;
#22304 = DIRECTION ( 'NONE',  ( 0.000000000000000000, 1.000000000000000000, 0.000000000000000000 ) ) ;
#22305 = DIRECTION ( 'NONE',  ( 0.000000000000000000, 1.000000000000000000, 0.000000000000000000 ) ) ;
#22306 = AXIS2_PLACEMENT_3D ( 'NONE', #78733, #125866, #28332 ) ;
#22307 = ORIENTED_EDGE ( 'NONE', *, *, #87154, .T. ) ;
#22308 = EDGE_CURVE ( 'NONE', #48610, #46747, #36267, .T. ) ;
#22310 = VECTOR ( 'NONE', #5968, 1000.000000000000000 ) ;
#22309 = AXIS2_PLACEMENT_3D ( 'NONE', #27253, #14833, #116276 ) ;
#22311 = EDGE_CURVE ( 'NONE', #88940, #59733, #107343, .T. ) ;
#22312 = DIRECTION ( 'NONE',  ( -4.274815082592931898E-19, -0.9999939076577903929, -0.003490651415223739937 ) ) ;
#22313 = EDGE_LOOP ( 'NONE', ( #109568, #71491, #65358, #59279 ) ) ;
#22314 = VERTEX_POINT ( 'NONE', #72676 ) ;
#22315 = DIRECTION ( 'NONE',  ( 0.000000000000000000, 1.000000000000000000, 0.000000000000000000 ) ) ;
#22316 = DIRECTION ( 'NONE',  ( -0.000000000000000000, -1.000000000000000000, -0.000000000000000000 ) ) ;
#22317 = CARTESIAN_POINT ( 'NONE',  ( 8.099999999999921485, 2.500000000000000000, -0.2464101615137783419 ) ) ;
#22318 = DIRECTION ( 'NONE',  ( -0.000000000000000000, -1.000000000000000000, -0.000000000000000000 ) ) ;
#22319 = DIRECTION ( 'NONE',  ( -0.000000000000000000, 1.000000000000000000, -0.000000000000000000 ) ) ;
#22320 = CARTESIAN_POINT ( 'NONE',  ( -10.40000000000000213, 2.500000000000000000, -4.230127018922197557 ) ) ;
#22321 = CARTESIAN_POINT ( 'NONE',  ( -6.050000000000020250, 2.500000000000000000, -6.941600689897078347 ) ) ;
#22322 = ORIENTED_EDGE ( 'NONE', *, *, #126274, .T. ) ;
#22323 = ORIENTED_EDGE ( 'NONE', *, *, #476, .F. ) ;
#22324 = ORIENTED_EDGE ( 'NONE', *, *, #118289, .F. ) ;
#22325 = ORIENTED_EDGE ( 'NONE', *, *, #4313, .T. ) ;
#22326 = VERTEX_POINT ( 'NONE', #33409 ) ;
#22327 = CARTESIAN_POINT ( 'NONE',  ( 9.999999999999912959, 2.500000000000000000, 3.637306695894644726 ) ) ;
#22328 = CARTESIAN_POINT ( 'NONE',  ( -10.20000000000000284, 2.500000000000000000, -0.3464101615137782364 ) ) ;
#22329 = AXIS2_PLACEMENT_3D ( 'NONE', #41275, #2598, #50426 ) ;
#22330 = DIRECTION ( 'NONE',  ( -0.000000000000000000, 1.000000000000000000, -0.000000000000000000 ) ) ;
#22332 = FACE_OUTER_BOUND ( 'NONE', #63409, .T. ) ;
#22331 = AXIS2_PLACEMENT_3D ( 'NONE', #16964, #68037, #96846 ) ;
#22333 = DIRECTION ( 'NONE',  ( 0.000000000000000000, 0.000000000000000000, -1.000000000000000000 ) ) ;
#22334 = VERTEX_POINT ( 'NONE', #74602 ) ;
#22335 = DIRECTION ( 'NONE',  ( 0.000000000000000000, 0.000000000000000000, 1.000000000000000000 ) ) ;
#22336 = CARTESIAN_POINT ( 'NONE',  ( 48.83367120242080972, -2.320420704099642517, 5.300559036899318066 ) ) ;
#22337 = CARTESIAN_POINT ( 'NONE',  ( 12.69999999999989804, 12.50000000000000000, 0.3464101615137735735 ) ) ;
#22338 = CARTESIAN_POINT ( 'NONE',  ( 11.24999999999990763, 12.50000000000000000, -7.188010851410854052 ) ) ;
#22340 = AXIS2_PLACEMENT_3D ( 'NONE', #70199, #65833, #129147 ) ;
#22339 = CIRCLE ( 'NONE', #68373, 0.06509327318403745899 ) ;
#22341 = DIRECTION ( 'NONE',  ( 0.000000000000000000, 1.000000000000000000, 0.000000000000000000 ) ) ;
#22342 = EDGE_CURVE ( 'NONE', #66463, #9837, #50930, .T. ) ;
#22343 = ORIENTED_EDGE ( 'NONE', *, *, #30915, .F. ) ;
#22344 = ORIENTED_EDGE ( 'NONE', *, *, #973, .T. ) ;
#22345 = ORIENTED_EDGE ( 'NONE', *, *, #104762, .T. ) ;
#22346 = DIRECTION ( 'NONE',  ( 0.000000000000000000, 1.000000000000000000, 0.000000000000000000 ) ) ;
#22347 = AXIS2_PLACEMENT_3D ( 'NONE', #23702, #34176, #44631 ) ;
#22348 = ORIENTED_EDGE ( 'NONE', *, *, #78930, .T. ) ;
#22350 = AXIS2_PLACEMENT_3D ( 'NONE', #626, #49762, #70031 ) ;
#22349 = CIRCLE ( 'NONE', #91284, 0.1000000000000002554 ) ;
#22351 = DIRECTION ( 'NONE',  ( -0.000000000000000000, -1.000000000000000000, -0.000000000000000000 ) ) ;
#22353 = EDGE_CURVE ( 'NONE', #56590, #92818, #69693, .T. ) ;
#22352 = LINE ( 'NONE', #42643, #8463 ) ;
#22354 = AXIS2_PLACEMENT_3D ( 'NONE', #52646, #2921, #41570 ) ;
#22356 = ORIENTED_EDGE ( 'NONE', *, *, #43401, .T. ) ;
#22355 = EDGE_CURVE ( 'NONE', #51914, #41353, #48778, .T. ) ;
#22357 = CARTESIAN_POINT ( 'NONE',  ( 9.349999999999916156, 2.500000000000000000, 6.941600689897073018 ) ) ;
#22358 = CARTESIAN_POINT ( 'NONE',  ( -10.60000000000000142, 2.500000000000000000, -0.2464101615137782308 ) ) ;
#22359 = CARTESIAN_POINT ( 'NONE',  ( -7.100000000000013856, 12.50000000000000000, 4.957854068765711553 ) ) ;
#22360 = EDGE_CURVE ( 'NONE', #30210, #120000, #107280, .T. ) ;
#22361 = CARTESIAN_POINT ( 'NONE',  ( -11.84999999999999609, 12.50000000000000000, 1.818653347947321475 ) ) ;
#22362 = CARTESIAN_POINT ( 'NONE',  ( -6.900000000000015454, 12.50000000000000000, 3.918623584224382839 ) ) ;
#22363 = ORIENTED_EDGE ( 'NONE', *, *, #50019, .F. ) ;
#22364 = ORIENTED_EDGE ( 'NONE', *, *, #114056, .F. ) ;
#22365 = EDGE_CURVE ( 'NONE', #114968, #49230, #94732, .T. ) ;
#22366 = CARTESIAN_POINT ( 'NONE',  ( 187.1666666666666856, -6.668395609140176816, -3.850000000000003642 ) ) ;
#22367 = VECTOR ( 'NONE', #126743, 1000.000000000000000 ) ;
#22368 = CARTESIAN_POINT ( 'NONE',  ( -0.2000000000000404232, 12.50000000000000000, 3.983716857408420964 ) ) ;
#22369 = CIRCLE ( 'NONE', #39099, 4.000000000000000000 ) ;
#22370 = DIRECTION ( 'NONE',  ( 0.000000000000000000, 0.000000000000000000, -1.000000000000000000 ) ) ;
#22371 = CONICAL_SURFACE ( 'NONE', #74673, 0.09999999999999982514, 0.003490658503988666988 ) ;
#22372 = DIRECTION ( 'NONE',  ( -0.000000000000000000, -1.000000000000000000, -0.000000000000000000 ) ) ;
#22373 = EDGE_LOOP ( 'NONE', ( #26423, #28835 ) ) ;
#22374 = CIRCLE ( 'NONE', #57962, 0.09999999999999982514 ) ;
#22375 = EDGE_LOOP ( 'NONE', ( #31992, #68819 ) ) ;
#22376 = FACE_OUTER_BOUND ( 'NONE', #102081, .T. ) ;
#22377 = LINE ( 'NONE', #43304, #96910 ) ;
#22378 = CARTESIAN_POINT ( 'NONE',  ( 2.099999999999950351, 2.500000000000000000, -0.7928203230275542301 ) ) ;
#22380 = DIRECTION ( 'NONE',  ( 0.000000000000000000, -0.000000000000000000, 1.000000000000000000 ) ) ;
#22379 = AXIS2_PLACEMENT_3D ( 'NONE', #111070, #61363, #91453 ) ;
#22381 = ORIENTED_EDGE ( 'NONE', *, *, #80202, .F. ) ;
#22382 = CARTESIAN_POINT ( 'NONE',  ( -3.350000000000028511, 12.50000000000000000, 2.922977105672686982 ) ) ;
#22383 = VECTOR ( 'NONE', #38785, 1000.000000000000000 ) ;
#22384 = DIRECTION ( 'NONE',  ( -0.000000000000000000, 1.000000000000000000, -0.000000000000000000 ) ) ;
#22385 = ORIENTED_EDGE ( 'NONE', *, *, #55205, .T. ) ;
#22386 = DIRECTION ( 'NONE',  ( 0.000000000000000000, 0.000000000000000000, 1.000000000000000000 ) ) ;
#22387 = ORIENTED_EDGE ( 'NONE', *, *, #122862, .F. ) ;
#22389 = CARTESIAN_POINT ( 'NONE',  ( -3.350000000000028511, 2.500000000000000000, -1.372243186433550033 ) ) ;
#22388 = AXIS2_PLACEMENT_3D ( 'NONE', #74694, #125080, #72123 ) ;
#22390 = EDGE_CURVE ( 'NONE', #2669, #125527, #111454, .T. ) ;
#22391 = AXIS2_PLACEMENT_3D ( 'NONE', #73927, #115111, #115782 ) ;
#22392 = EDGE_LOOP ( 'NONE', ( #113341, #49257 ) ) ;
#22393 = LINE ( 'NONE', #53764, #115430 ) ;
#22394 = CARTESIAN_POINT ( 'NONE',  ( 0.3999999999999568345, 2.500000000000000000, -3.637306695894650055 ) ) ;
#22395 = ORIENTED_EDGE ( 'NONE', *, *, #11140, .F. ) ;
#22396 = EDGE_LOOP ( 'NONE', ( #71494, #101925, #64104, #95498 ) ) ;
#22397 = ADVANCED_FACE ( 'NONE', ( #65416 ), #78014, .T. ) ;
#22398 = FACE_OUTER_BOUND ( 'NONE', #35561, .T. ) ;
#22399 = LINE ( 'NONE', #62944, #87379 ) ;
#22400 = EDGE_CURVE ( 'NONE', #67418, #86712, #13246, .T. ) ;
#22401 = FACE_OUTER_BOUND ( 'NONE', #3009, .T. ) ;
#22402 = CARTESIAN_POINT ( 'NONE',  ( 184.5677083336747444, -4.367472073101514418, -7.564683531250002702 ) ) ;
#22403 = DIRECTION ( 'NONE',  ( 0.000000000000000000, 0.000000000000000000, 1.000000000000000000 ) ) ;
#22404 = DIRECTION ( 'NONE',  ( 0.000000000000000000, 0.000000000000000000, 1.000000000000000000 ) ) ;
#22405 = DIRECTION ( 'NONE',  ( 0.000000000000000000, -0.9999939076577903929, 0.003490651415223739937 ) ) ;
#22406 = EDGE_CURVE ( 'NONE', #28605, #80531, #54955, .T. ) ;
#22407 = EDGE_CURVE ( 'NONE', #7993, #45906, #105197, .T. ) ;
#22408 = CARTESIAN_POINT ( 'NONE',  ( -7.500000000000016875, 2.500000000000000000, -3.737306695894649700 ) ) ;
#22409 = CARTESIAN_POINT ( 'NONE',  ( 13.09999999999990195, 2.500000000000000000, -4.776537180435978414 ) ) ;
#22410 = EDGE_CURVE ( 'NONE', #102525, #66158, #11196, .T. ) ;
#22411 = VECTOR ( 'NONE', #22760, 1000.000000000000000 ) ;
#22412 = EDGE_CURVE ( 'NONE', #12097, #57754, #25781, .T. ) ;
#22413 = ORIENTED_EDGE ( 'NONE', *, *, #128966, .T. ) ;
#22414 = EDGE_LOOP ( 'NONE', ( #53270, #52441 ) ) ;
#22415 = CARTESIAN_POINT ( 'NONE',  ( -10.40000000000000213, 12.50000000000000000, 3.637306695894644726 ) ) ;
#22416 = ADVANCED_FACE ( 'NONE', ( #56241 ), #27929, .T. ) ;
#22417 = ORIENTED_EDGE ( 'NONE', *, *, #124898, .T. ) ;
#22418 = DIRECTION ( 'NONE',  ( 0.000000000000000000, -0.000000000000000000, 1.000000000000000000 ) ) ;
#22419 = FACE_OUTER_BOUND ( 'NONE', #95588, .T. ) ;
#22420 = CARTESIAN_POINT ( 'NONE',  ( -3.750000000000027534, 12.50000000000000000, 2.857883832488649301 ) ) ;
#22422 = ORIENTED_EDGE ( 'NONE', *, *, #84747, .T. ) ;
#22421 = ORIENTED_EDGE ( 'NONE', *, *, #103486, .T. ) ;
#22423 = FACE_BOUND ( 'NONE', #123725, .T. ) ;
#22424 = ORIENTED_EDGE ( 'NONE', *, *, #68680, .T. ) ;
#22425 = DIRECTION ( 'NONE',  ( -0.000000000000000000, -1.000000000000000000, -0.000000000000000000 ) ) ;
#22426 = FACE_OUTER_BOUND ( 'NONE', #34847, .T. ) ;
#22427 = ADVANCED_FACE ( 'NONE', ( #104689 ), #5199, .T. ) ;
#22428 = DIRECTION ( 'NONE',  ( 0.000000000000000000, -0.9999939076577903929, 0.003490651415223739937 ) ) ;
#22429 = DIRECTION ( 'NONE',  ( 0.000000000000000000, -0.9999939076577903929, 0.003490651415223739937 ) ) ;
#22430 = CIRCLE ( 'NONE', #118540, 0.06509327318403745899 ) ;
#22431 = DIRECTION ( 'NONE',  ( -0.000000000000000000, 1.000000000000000000, -0.000000000000000000 ) ) ;
#22432 = AXIS2_PLACEMENT_3D ( 'NONE', #12964, #52920, #93491 ) ;
#22433 = DIRECTION ( 'NONE',  ( -0.000000000000000000, -1.000000000000000000, -0.000000000000000000 ) ) ;
#22434 = CARTESIAN_POINT ( 'NONE',  ( -15.79999999999998117, 12.50000000000000000, 0.000000000000000000 ) ) ;
#22435 = LINE ( 'NONE', #119969, #19195 ) ;
#22436 = DIRECTION ( 'NONE',  ( 0.000000000000000000, 0.000000000000000000, 1.000000000000000000 ) ) ;
#22437 = DIRECTION ( 'NONE',  ( 0.000000000000000000, 0.000000000000000000, -1.000000000000000000 ) ) ;
#22438 = LINE ( 'NONE', #71507, #38980 ) ;
#22440 = VECTOR ( 'NONE', #110540, 1000.000000000000000 ) ;
#22439 = AXIS2_PLACEMENT_3D ( 'NONE', #20896, #9139, #60825 ) ;
#22441 = ORIENTED_EDGE ( 'NONE', *, *, #31666, .T. ) ;
#22442 = ORIENTED_EDGE ( 'NONE', *, *, #92244, .F. ) ;
#22443 = VERTEX_POINT ( 'NONE', #126286 ) ;
#22444 = DIRECTION ( 'NONE',  ( 0.000000000000000000, 0.000000000000000000, 1.000000000000000000 ) ) ;
#22445 = ORIENTED_EDGE ( 'NONE', *, *, #24124, .F. ) ;
#22446 = LINE ( 'NONE', #70239, #83163 ) ;
#22447 = DIRECTION ( 'NONE',  ( 0.000000000000000000, 1.000000000000000000, 0.000000000000000000 ) ) ;
#22449 = ORIENTED_EDGE ( 'NONE', *, *, #72836, .T. ) ;
#22448 = VERTEX_POINT ( 'NONE', #67323 ) ;
#22450 = ORIENTED_EDGE ( 'NONE', *, *, #49296, .T. ) ;
#22451 = DIRECTION ( 'NONE',  ( 0.000000000000000000, 1.000000000000000000, 0.000000000000000000 ) ) ;
#22452 = CONICAL_SURFACE ( 'NONE', #91375, 0.09999999999999982514, 0.003490658503988666988 ) ;
#22453 = AXIS2_PLACEMENT_3D ( 'NONE', #69552, #111400, #92417 ) ;
#22454 = DIRECTION ( 'NONE',  ( 0.000000000000000000, 0.000000000000000000, -1.000000000000000000 ) ) ;
#22455 = CARTESIAN_POINT ( 'NONE',  ( -2.900000000000029221, 12.50000000000000000, 0.06509327318403515528 ) ) ;
#22456 = DIRECTION ( 'NONE',  ( -0.000000000000000000, -1.000000000000000000, -0.000000000000000000 ) ) ;
#22457 = DIRECTION ( 'NONE',  ( 0.000000000000000000, 0.000000000000000000, 1.000000000000000000 ) ) ;
#22458 = DIRECTION ( 'NONE',  ( 0.000000000000000000, 0.000000000000000000, 1.000000000000000000 ) ) ;
#22459 = ORIENTED_EDGE ( 'NONE', *, *, #67561, .T. ) ;
#22460 = DIRECTION ( 'NONE',  ( 0.000000000000000000, 0.000000000000000000, 1.000000000000000000 ) ) ;
#22461 = VERTEX_POINT ( 'NONE', #77808 ) ;
#22462 = AXIS2_PLACEMENT_3D ( 'NONE', #24499, #95813, #26439 ) ;
#22463 = EDGE_LOOP ( 'NONE', ( #51362, #101986, #55613, #41326 ) ) ;
#22464 = EDGE_CURVE ( 'NONE', #35194, #22628, #82222, .T. ) ;
#22465 = EDGE_LOOP ( 'NONE', ( #101232, #5698, #64797, #66986 ) ) ;
#22466 = FACE_OUTER_BOUND ( 'NONE', #19643, .T. ) ;
#22467 = ORIENTED_EDGE ( 'NONE', *, *, #110254, .F. ) ;
#22468 = VERTEX_POINT ( 'NONE', #26152 ) ;
#22469 = ORIENTED_EDGE ( 'NONE', *, *, #51756, .F. ) ;
#22470 = AXIS2_PLACEMENT_3D ( 'NONE', #72011, #2592, #53010 ) ;
#22472 =( LENGTH_UNIT ( ) NAMED_UNIT ( * ) SI_UNIT ( .MILLI., .METRE. ) );
#22471 = AXIS2_PLACEMENT_3D ( 'NONE', #80319, #79035, #37806 ) ;
#22473 = EDGE_CURVE ( 'NONE', #103996, #48300, #125617, .T. ) ;
#22474 = FACE_OUTER_BOUND ( 'NONE', #20928, .T. ) ;
#22476 = AXIS2_PLACEMENT_3D ( 'NONE', #46813, #126661, #76269 ) ;
#22475 = DIRECTION ( 'NONE',  ( 0.000000000000000000, 0.000000000000000000, 1.000000000000000000 ) ) ;
#22477 = DIRECTION ( 'NONE',  ( 0.000000000000000000, 1.000000000000000000, 0.000000000000000000 ) ) ;
#22478 = CARTESIAN_POINT ( 'NONE',  ( -1.850000000000033396, 12.50000000000000000, -6.776507416713039689 ) ) ;
#22479 = DIRECTION ( 'NONE',  ( 0.000000000000000000, 0.000000000000000000, 1.000000000000000000 ) ) ;
#22480 = CIRCLE ( 'NONE', #93554, 0.06509327318403745899 ) ;
#22482 = VECTOR ( 'NONE', #27221, 1000.000000000000000 ) ;
#22481 = CARTESIAN_POINT ( 'NONE',  ( 14.34999999999989662, 2.500000000000000000, 1.918653347947321564 ) ) ;
#22483 = ORIENTED_EDGE ( 'NONE', *, *, #80475, .T. ) ;
#22484 = AXIS2_PLACEMENT_3D ( 'NONE', #34723, #3940, #104709 ) ;
#22485 = AXIS2_PLACEMENT_3D ( 'NONE', #124408, #24266, #45207 ) ;
#22486 = DIRECTION ( 'NONE',  ( 0.000000000000000000, 1.000000000000000000, 0.000000000000000000 ) ) ;
#22487 = ORIENTED_EDGE ( 'NONE', *, *, #99399, .F. ) ;
#22488 = FACE_OUTER_BOUND ( 'NONE', #37181, .T. ) ;
#22489 = ORIENTED_EDGE ( 'NONE', *, *, #128105, .F. ) ;
#22490 = DIRECTION ( 'NONE',  ( -0.000000000000000000, -1.000000000000000000, -0.000000000000000000 ) ) ;
#22491 = AXIS2_PLACEMENT_3D ( 'NONE', #41773, #51584, #62048 ) ;
#22492 = VERTEX_POINT ( 'NONE', #75885 ) ;
#22493 = CARTESIAN_POINT ( 'NONE',  ( 10.39999999999991154, 2.500000000000000000, 3.537306695894645081 ) ) ;
#22495 = AXIS2_PLACEMENT_3D ( 'NONE', #52832, #82950, #16104 ) ;
#22494 = CIRCLE ( 'NONE', #55910, 0.09999999999999999167 ) ;
#22496 = DIRECTION ( 'NONE',  ( 0.000000000000000000, 0.000000000000000000, -1.000000000000000000 ) ) ;
#22497 = EDGE_LOOP ( 'NONE', ( #108127, #43946 ) ) ;
#22498 = ORIENTED_EDGE ( 'NONE', *, *, #126836, .T. ) ;
#22499 = DIRECTION ( 'NONE',  ( 0.000000000000000000, -0.9999939076577903929, 0.003490651415223739937 ) ) ;
#22500 = FACE_OUTER_BOUND ( 'NONE', #17604, .T. ) ;
#22501 = DIRECTION ( 'NONE',  ( 0.000000000000000000, -0.9999939076577903929, 0.003490651415223739937 ) ) ;
#22502 = LINE ( 'NONE', #62419, #95290 ) ;
#22503 = DIRECTION ( 'NONE',  ( 0.000000000000000000, 1.000000000000000000, 0.000000000000000000 ) ) ;
#22504 = ADVANCED_FACE ( 'NONE', ( #66062 ), #96873, .T. ) ;
#22505 = ORIENTED_EDGE ( 'NONE', *, *, #97923, .T. ) ;
#22506 = DIRECTION ( 'NONE',  ( 0.000000000000000000, -0.9999939076577903929, 0.003490651415223739937 ) ) ;
#22507 = AXIS2_PLACEMENT_3D ( 'NONE', #16535, #68872, #27030 ) ;
#22508 = ORIENTED_EDGE ( 'NONE', *, *, #1803, .F. ) ;
#22509 = FACE_OUTER_BOUND ( 'NONE', #17626, .T. ) ;
#22511 = EDGE_CURVE ( 'NONE', #18296, #81272, #76542, .T. ) ;
#22510 = DIRECTION ( 'NONE',  ( -0.000000000000000000, 1.000000000000000000, -0.000000000000000000 ) ) ;
#22512 = EDGE_CURVE ( 'NONE', #86788, #43040, #57175, .T. ) ;
#22513 = ADVANCED_FACE ( 'NONE', ( #86994 ), #42529, .T. ) ;
#22514 = DIRECTION ( 'NONE',  ( -0.000000000000000000, -1.000000000000000000, -0.000000000000000000 ) ) ;
#22515 = LINE ( 'NONE', #59870, #7079 ) ;
#22516 = DIRECTION ( 'NONE',  ( 0.000000000000000000, 0.000000000000000000, 1.000000000000000000 ) ) ;
#22517 = DIRECTION ( 'NONE',  ( 0.000000000000000000, -0.9999939076577903929, 0.003490651415223739937 ) ) ;
#22518 = EDGE_CURVE ( 'NONE', #77451, #60396, #101087, .T. ) ;
#22519 = DIRECTION ( 'NONE',  ( 1.000000000000000000, 0.000000000000000000, 0.000000000000000000 ) ) ;
#22520 = ORIENTED_EDGE ( 'NONE', *, *, #126109, .F. ) ;
#22521 = VECTOR ( 'NONE', #33852, 1000.000000000000000 ) ;
#22522 = FACE_OUTER_BOUND ( 'NONE', #21235, .T. ) ;
#22523 = AXIS2_PLACEMENT_3D ( 'NONE', #25071, #6058, #74819 ) ;
#22524 = DIRECTION ( 'NONE',  ( -0.000000000000000000, -1.000000000000000000, -0.000000000000000000 ) ) ;
#22525 = DIRECTION ( 'NONE',  ( 0.000000000000000000, 1.000000000000000000, 0.000000000000000000 ) ) ;
#22526 = EDGE_CURVE ( 'NONE', #39789, #119576, #15298, .T. ) ;
#22527 = ORIENTED_EDGE ( 'NONE', *, *, #97497, .F. ) ;
#22528 = EDGE_CURVE ( 'NONE', #114300, #1392, #49675, .T. ) ;
#22529 = ORIENTED_EDGE ( 'NONE', *, *, #115908, .T. ) ;
#22530 = DIRECTION ( 'NONE',  ( 0.000000000000000000, 0.000000000000000000, 1.000000000000000000 ) ) ;
#22531 = CIRCLE ( 'NONE', #129432, 0.1000000000000002554 ) ;
#22532 = ORIENTED_EDGE ( 'NONE', *, *, #45344, .T. ) ;
#22533 = ORIENTED_EDGE ( 'NONE', *, *, #73086, .F. ) ;
#22534 = DIRECTION ( 'NONE',  ( 0.000000000000000000, 0.000000000000000000, 1.000000000000000000 ) ) ;
#22535 = EDGE_LOOP ( 'NONE', ( #16959, #109650 ) ) ;
#22536 = DIRECTION ( 'NONE',  ( 0.000000000000000000, 1.000000000000000000, 0.000000000000000000 ) ) ;
#22537 = DIRECTION ( 'NONE',  ( -0.000000000000000000, 1.000000000000000000, -0.000000000000000000 ) ) ;
#22538 = CARTESIAN_POINT ( 'NONE',  ( -9.600000000000006750, 12.50000000000000000, -0.7579135962115917113 ) ) ;
#22539 = ORIENTED_EDGE ( 'NONE', *, *, #76315, .T. ) ;
#22540 = AXIS2_PLACEMENT_3D ( 'NONE', #51711, #13, #80529 ) ;
#22541 = FACE_OUTER_BOUND ( 'NONE', #71226, .T. ) ;
#22542 = CARTESIAN_POINT ( 'NONE',  ( 8.149999999999920419, 12.50000000000000000, -2.511473670974877948 ) ) ;
#22543 = ORIENTED_EDGE ( 'NONE', *, *, #111519, .T. ) ;
#22544 = VERTEX_POINT ( 'NONE', #10371 ) ;
#22545 = ORIENTED_EDGE ( 'NONE', *, *, #38255, .F. ) ;
#22546 = CIRCLE ( 'NONE', #101953, 0.09999999999999982514 ) ;
#22547 = DIRECTION ( 'NONE',  ( 0.000000000000000000, 0.000000000000000000, 1.000000000000000000 ) ) ;
#22548 = CARTESIAN_POINT ( 'NONE',  ( 183.9479166673494603, -6.668395609140176816, -3.850000000000003642 ) ) ;
#22549 = CARTESIAN_POINT ( 'NONE',  ( 10.19999999999991402, 12.50000000000000000, 0.2813168883297361700 ) ) ;
#22550 = FACE_BOUND ( 'NONE', #5234, .T. ) ;
#22551 = VERTEX_POINT ( 'NONE', #48362 ) ;
#22552 = CIRCLE ( 'NONE', #37126, 0.06509327318403741736 ) ;
#22553 = CARTESIAN_POINT ( 'NONE',  ( 3.349999999999945466, 2.500000000000000000, -2.957883832488653830 ) ) ;
#22554 = CARTESIAN_POINT ( 'NONE',  ( -7.900000000000011013, 2.500000000000000000, 4.230127018922196669 ) ) ;
#22555 = AXIS2_PLACEMENT_3D ( 'NONE', #75876, #85051, #105989 ) ;
#22556 = ORIENTED_EDGE ( 'NONE', *, *, #81654, .F. ) ;
#22557 = CARTESIAN_POINT ( 'NONE',  ( 6.049999999999934097, 12.50000000000000000, 6.148780366869520897 ) ) ;
#22558 = CARTESIAN_POINT ( 'NONE',  ( 11.84999999999990372, 2.500000000000000000, -6.148780366869526226 ) ) ;
#22559 = VECTOR ( 'NONE', #116672, 1000.000000000000000 ) ;
#22561 = ADVANCED_FACE ( 'NONE', ( #60766 ), #34208, .T. ) ;
#22560 = LINE ( 'NONE', #64392, #11014 ) ;
#22562 = DIRECTION ( 'NONE',  ( 0.000000000000000000, 1.000000000000000000, 0.000000000000000000 ) ) ;
#22563 = CARTESIAN_POINT ( 'NONE',  ( -0.6500000000000394351, 2.500000000000000000, 6.841600689897072485 ) ) ;
#22564 = ADVANCED_FACE ( 'NONE', ( #109202 ), #19545, .F. ) ;
#22565 = DIRECTION ( 'NONE',  ( 0.000000000000000000, 0.000000000000000000, 1.000000000000000000 ) ) ;
#22566 = CARTESIAN_POINT ( 'NONE',  ( -12.29999999999999538, 2.500000000000000000, -4.776537180435975749 ) ) ;
#22567 = ADVANCED_FACE ( 'NONE', ( #78491 ), #65480, .T. ) ;
#22568 = CIRCLE ( 'NONE', #87287, 0.06509327318403745899 ) ;
#22569 = EDGE_CURVE ( 'NONE', #39091, #120001, #32062, .T. ) ;
#22570 = AXIS2_PLACEMENT_3D ( 'NONE', #9140, #20252, #49088 ) ;
#22571 = ORIENTED_EDGE ( 'NONE', *, *, #68573, .T. ) ;
#22572 = ORIENTED_EDGE ( 'NONE', *, *, #120553, .F. ) ;
#22574 = ORIENTED_EDGE ( 'NONE', *, *, #42244, .F. ) ;
#22573 = EDGE_CURVE ( 'NONE', #118322, #100139, #99410, .T. ) ;
#22575 = VERTEX_POINT ( 'NONE', #18892 ) ;
#22576 = DIRECTION ( 'NONE',  ( -4.274815082592931898E-19, -0.9999939076577903929, -0.003490651415223739937 ) ) ;
#22577 = DIRECTION ( 'NONE',  ( -0.000000000000000000, 1.000000000000000000, -0.000000000000000000 ) ) ;
#22578 = FACE_OUTER_BOUND ( 'NONE', #121036, .T. ) ;
#22579 = CIRCLE ( 'NONE', #10041, 0.09999999999999982514 ) ;
#22580 = VERTEX_POINT ( 'NONE', #90864 ) ;
#22581 = FACE_BOUND ( 'NONE', #106573, .T. ) ;
#22582 = DIRECTION ( 'NONE',  ( 0.000000000000000000, 0.000000000000000000, 1.000000000000000000 ) ) ;
#22583 = DIRECTION ( 'NONE',  ( 0.000000000000000000, 1.000000000000000000, 0.000000000000000000 ) ) ;
#22584 = EDGE_CURVE ( 'NONE', #81852, #113860, #58831, .T. ) ;
#22585 = CARTESIAN_POINT ( 'NONE',  ( 4.549999999999937650, 2.500000000000000000, 2.265063509461097357 ) ) ;
#22588 = EDGE_CURVE ( 'NONE', #79738, #15950, #19516, .T. ) ;
#22587 = VECTOR ( 'NONE', #48829, 1000.000000000000000 ) ;
#22586 = AXIS2_PLACEMENT_3D ( 'NONE', #4712, #103597, #125781 ) ;
#22589 = LINE ( 'NONE', #82789, #65826 ) ;
#22590 = CARTESIAN_POINT ( 'NONE',  ( 0.1999999999999571565, 12.50000000000000000, 3.983716857408420076 ) ) ;
#22591 = FACE_OUTER_BOUND ( 'NONE', #100657, .T. ) ;
#22592 = FACE_OUTER_BOUND ( 'NONE', #60665, .T. ) ;
#22593 = DIRECTION ( 'NONE',  ( 0.000000000000000000, -0.9999939076577903929, 0.003490651415223739937 ) ) ;
#22594 = CARTESIAN_POINT ( 'NONE',  ( -7.100000000000014744, 2.500000000000000000, 4.330127018922196314 ) ) ;
#22595 = ADVANCED_FACE ( 'NONE', ( #109870 ), #92683, .T. ) ;
#22596 = ORIENTED_EDGE ( 'NONE', *, *, #116372, .F. ) ;
#22597 = ORIENTED_EDGE ( 'NONE', *, *, #26500, .F. ) ;
#22598 = VERTEX_POINT ( 'NONE', #81058 ) ;
#22599 = EDGE_LOOP ( 'NONE', ( #62449, #103802, #17418, #22543 ) ) ;
#22600 = ORIENTED_EDGE ( 'NONE', *, *, #126836, .F. ) ;
#22601 = VERTEX_POINT ( 'NONE', #20195 ) ;
#22602 = CARTESIAN_POINT ( 'NONE',  ( -5.600000000000023626, 12.50000000000000000, -4.741630453620015118 ) ) ;
#22603 = ORIENTED_EDGE ( 'NONE', *, *, #65701, .F. ) ;
#22604 = ORIENTED_EDGE ( 'NONE', *, *, #116704, .T. ) ;
#22605 = CARTESIAN_POINT ( 'NONE',  ( -4.150000000000024336, 12.50000000000000000, 2.165063509461097713 ) ) ;
#22606 = CARTESIAN_POINT ( 'NONE',  ( 14.69113575703618402, -2.499999999999999556, 6.337000354878961517 ) ) ;
#22607 = LINE ( 'NONE', #90675, #45817 ) ;
#22608 = FACE_OUTER_BOUND ( 'NONE', #128588, .T. ) ;
#22609 = CONICAL_SURFACE ( 'NONE', #118728, 0.09999999999999999167, 0.003490658503988666988 ) ;
#22610 = ORIENTED_EDGE ( 'NONE', *, *, #31488, .T. ) ;
#22611 = DIRECTION ( 'NONE',  ( 0.000000000000000000, -0.9999939076577903929, 0.003490651415223739937 ) ) ;
#22612 = AXIS2_PLACEMENT_3D ( 'NONE', #26312, #55754, #74763 ) ;
#22613 = EDGE_LOOP ( 'NONE', ( #68571, #9359 ) ) ;
#22614 = AXIS2_PLACEMENT_3D ( 'NONE', #22995, #70793, #23626 ) ;
#22615 = VERTEX_POINT ( 'NONE', #129534 ) ;
#22616 = DIRECTION ( 'NONE',  ( 0.000000000000000000, 0.000000000000000000, 1.000000000000000000 ) ) ;
#22617 = CARTESIAN_POINT ( 'NONE',  ( -2.100000000000034284, 2.500000000000000000, -4.430127018922202176 ) ) ;
#22618 = ORIENTED_EDGE ( 'NONE', *, *, #16005, .T. ) ;
#22620 = VERTEX_POINT ( 'NONE', #49028 ) ;
#22619 = CIRCLE ( 'NONE', #102022, 0.1000000000000002554 ) ;
#22621 = DIRECTION ( 'NONE',  ( -4.274815082592931898E-19, -0.9999939076577903929, -0.003490651415223739937 ) ) ;
#22622 = EDGE_CURVE ( 'NONE', #85816, #99488, #121934, .T. ) ;
#22623 = CONICAL_SURFACE ( 'NONE', #114619, 0.1000000000000000056, 0.003490658503988666988 ) ;
#22624 = CARTESIAN_POINT ( 'NONE',  ( 5.649999999999936406, 12.50000000000000000, -6.841600689897077814 ) ) ;
#22625 = FACE_OUTER_BOUND ( 'NONE', #92953, .T. ) ;
#22626 = CARTESIAN_POINT ( 'NONE',  ( 7.299999999999924327, 2.500000000000000000, 0.4464101615137735513 ) ) ;
#22627 = CARTESIAN_POINT ( 'NONE',  ( -13.14999999999999147, 12.50000000000000000, -2.576566944158912964 ) ) ;
#22628 = VERTEX_POINT ( 'NONE', #79755 ) ;
#22629 = CARTESIAN_POINT ( 'NONE',  ( -0.8500000000000386136, 2.500000000000000000, 2.957883832488649389 ) ) ;
#22630 = AXIS2_PLACEMENT_3D ( 'NONE', #57507, #67277, #7091 ) ;
#22631 = ORIENTED_EDGE ( 'NONE', *, *, #96520, .F. ) ;
#22632 = DIRECTION ( 'NONE',  ( 0.000000000000000000, 0.000000000000000000, 1.000000000000000000 ) ) ;
#22633 = CARTESIAN_POINT ( 'NONE',  ( -10.85000000000000142, 2.500000000000000000, -2.065063509461098068 ) ) ;
#22634 = DIRECTION ( 'NONE',  ( -0.000000000000000000, -1.000000000000000000, -0.000000000000000000 ) ) ;
#22635 = DIRECTION ( 'NONE',  ( -0.000000000000000000, 1.000000000000000000, -0.000000000000000000 ) ) ;
#22636 = CARTESIAN_POINT ( 'NONE',  ( 4.149999999999936406, 12.50000000000000000, 6.560283801567334372 ) ) ;
#22637 = EDGE_LOOP ( 'NONE', ( #5573, #83462, #124417, #103571 ) ) ;
#22639 = AXIS2_PLACEMENT_3D ( 'NONE', #29401, #16947, #57570 ) ;
#22638 = LINE ( 'NONE', #52722, #109460 ) ;
#22640 = CARTESIAN_POINT ( 'NONE',  ( -13.74999999999998757, 2.500000000000000000, 1.372243186433549367 ) ) ;
#22641 = ORIENTED_EDGE ( 'NONE', *, *, #38089, .F. ) ;
#22642 = ORIENTED_EDGE ( 'NONE', *, *, #57300, .F. ) ;
#22643 = ORIENTED_EDGE ( 'NONE', *, *, #97859, .T. ) ;
#22644 = CARTESIAN_POINT ( 'NONE',  ( 2.500000000000002220, 0.9166666666666682950, 10.00000000000000178 ) ) ;
#22645 = DIRECTION ( 'NONE',  ( 0.000000000000000000, 0.000000000000000000, 1.000000000000000000 ) ) ;
#22646 = CARTESIAN_POINT ( 'NONE',  ( 186.2343750003414016, 8.734944146203032389, 5.348610694689227483E-16 ) ) ;
#22647 = AXIS2_PLACEMENT_3D ( 'NONE', #3432, #112755, #83301 ) ;
#22648 = CARTESIAN_POINT ( 'NONE',  ( 0.8499999999999557909, 12.50000000000000000, -7.122917578226816815 ) ) ;
#22649 = DIRECTION ( 'NONE',  ( 0.000000000000000000, 0.000000000000000000, -1.000000000000000000 ) ) ;
#22650 = CIRCLE ( 'NONE', #85417, 0.09999999999999982514 ) ;
#22651 = CARTESIAN_POINT ( 'NONE',  ( -14.34999999999998543, 12.50000000000000000, 1.818653347947325472 ) ) ;
#22652 = CARTESIAN_POINT ( 'NONE',  ( 184.5000000000000000, 0.000000000000000000, 0.000000000000000000 ) ) ;
#22653 = CONICAL_SURFACE ( 'NONE', #18133, 0.1000000000000002554, 0.003490658503988666988 ) ;
#22654 = DIRECTION ( 'NONE',  ( 0.000000000000000000, 0.000000000000000000, -1.000000000000000000 ) ) ;
#22655 = EDGE_CURVE ( 'NONE', #80727, #116053, #119970, .T. ) ;
#22656 = ORIENTED_EDGE ( 'NONE', *, *, #36673, .F. ) ;
#22657 = CARTESIAN_POINT ( 'NONE',  ( -9.150000000000009237, 2.500000000000000000, -2.065063509461102065 ) ) ;
#22658 = CIRCLE ( 'NONE', #49851, 0.09999999999999982514 ) ;
#22659 = ADVANCED_FACE ( 'NONE', ( #120969 ), #86506, .T. ) ;
#22660 = CARTESIAN_POINT ( 'NONE',  ( 13.54999999999989591, 2.500000000000000000, -1.918653347947326004 ) ) ;
#22661 = DIRECTION ( 'NONE',  ( 0.000000000000000000, -0.000000000000000000, 1.000000000000000000 ) ) ;
#22662 = DIRECTION ( 'NONE',  ( 0.000000000000000000, 0.000000000000000000, 1.000000000000000000 ) ) ;
#22663 = EDGE_CURVE ( 'NONE', #35730, #79726, #88565, .T. ) ;
#22664 = ORIENTED_EDGE ( 'NONE', *, *, #59188, .F. ) ;
#22665 = LINE ( 'NONE', #82871, #6893 ) ;
#22667 = AXIS2_PLACEMENT_3D ( 'NONE', #102821, #74028, #63570 ) ;
#22666 = AXIS2_PLACEMENT_3D ( 'NONE', #110512, #100676, #543 ) ;
#22668 = DIRECTION ( 'NONE',  ( -0.000000000000000000, 1.000000000000000000, -0.000000000000000000 ) ) ;
#22670 = ORIENTED_EDGE ( 'NONE', *, *, #6078, .F. ) ;
#22669 = DIRECTION ( 'NONE',  ( 0.000000000000000000, -0.9999939076577903929, 0.003490651415223739937 ) ) ;
#22671 = EDGE_CURVE ( 'NONE', #37370, #11311, #30103, .T. ) ;
#22672 = EDGE_CURVE ( 'NONE', #124700, #103089, #69790, .T. ) ;
#22673 = EDGE_CURVE ( 'NONE', #26935, #128257, #23824, .T. ) ;
#22674 = EDGE_CURVE ( 'NONE', #53806, #6433, #92815, .T. ) ;
#22675 = EDGE_CURVE ( 'NONE', #87575, #84227, #44758, .T. ) ;
#22676 = ORIENTED_EDGE ( 'NONE', *, *, #67736, .T. ) ;
#22677 = DIRECTION ( 'NONE',  ( -0.000000000000000000, -1.000000000000000000, -0.000000000000000000 ) ) ;
#22678 = VERTEX_POINT ( 'NONE', #52880 ) ;
#22679 = EDGE_LOOP ( 'NONE', ( #35318, #20280, #89017, #49040 ) ) ;
#22680 = DIRECTION ( 'NONE',  ( 0.000000000000000000, -0.9999939076577903929, 0.003490651415223739937 ) ) ;
#22681 = AXIS2_PLACEMENT_3D ( 'NONE', #1441, #40091, #89823 ) ;
#22682 = ADVANCED_FACE ( 'NONE', ( #103273 ), #73793, .T. ) ;
#22683 = DIRECTION ( 'NONE',  ( 0.000000000000000000, 0.000000000000000000, -1.000000000000000000 ) ) ;
#22684 = CARTESIAN_POINT ( 'NONE',  ( 8.549999999999922551, 2.500000000000000000, -6.248780366869526759 ) ) ;
#22685 = DIRECTION ( 'NONE',  ( 0.000000000000000000, 0.000000000000000000, 1.000000000000000000 ) ) ;
#22686 = ORIENTED_EDGE ( 'NONE', *, *, #115771, .T. ) ;
#22687 = AXIS2_PLACEMENT_3D ( 'NONE', #3326, #32809, #51793 ) ;
#22688 = CIRCLE ( 'NONE', #85365, 0.06509327318403745899 ) ;
#22689 = AXIS2_PLACEMENT_3D ( 'NONE', #55441, #35177, #75712 ) ;
#22690 = CARTESIAN_POINT ( 'NONE',  ( 12.09999999999990550, 12.50000000000000000, 3.637306695894644726 ) ) ;
#22692 = VERTEX_POINT ( 'NONE', #23400 ) ;
#22691 = LINE ( 'NONE', #102518, #102240 ) ;
#22693 = CARTESIAN_POINT ( 'NONE',  ( -8.300000000000011369, 12.50000000000000000, -0.06509327318403970719 ) ) ;
#22694 = DIRECTION ( 'NONE',  ( 0.000000000000000000, 1.000000000000000000, 0.000000000000000000 ) ) ;
#22695 = VECTOR ( 'NONE', #54450, 1000.000000000000000 ) ;
#22696 = VERTEX_POINT ( 'NONE', #63342 ) ;
#22697 = AXIS2_PLACEMENT_3D ( 'NONE', #123680, #64773, #24220 ) ;
#22698 = AXIS2_PLACEMENT_3D ( 'NONE', #84486, #34100, #55012 ) ;
#22699 = ORIENTED_EDGE ( 'NONE', *, *, #118271, .F. ) ;
#22700 = VERTEX_POINT ( 'NONE', #1831 ) ;
#22701 = ORIENTED_EDGE ( 'NONE', *, *, #36244, .T. ) ;
#22702 = DIRECTION ( 'NONE',  ( 0.000000000000000000, 0.000000000000000000, 1.000000000000000000 ) ) ;
#22703 = CARTESIAN_POINT ( 'NONE',  ( 13.12246079397621124, 2.499999999999999556, 7.156134182876439098 ) ) ;
#22704 = CARTESIAN_POINT ( 'NONE',  ( -12.09999999999999609, 12.50000000000000000, -0.7579135962115876035 ) ) ;
#22705 = FACE_BOUND ( 'NONE', #81587, .T. ) ;
#22706 = ORIENTED_EDGE ( 'NONE', *, *, #42342, .T. ) ;
#22707 = CARTESIAN_POINT ( 'NONE',  ( 185.7812500006828031, 0.000000000000000000, 7.700000000000000178 ) ) ;
#22708 = DIRECTION ( 'NONE',  ( -0.000000000000000000, -1.000000000000000000, -0.000000000000000000 ) ) ;
#22709 = CARTESIAN_POINT ( 'NONE',  ( -8.150000000000014566, 2.500000000000000000, -6.841600689897073373 ) ) ;
#22710 = CIRCLE ( 'NONE', #116770, 0.1000000000000000056 ) ;
#22712 = EDGE_CURVE ( 'NONE', #42689, #27189, #81685, .T. ) ;
#22711 = CARTESIAN_POINT ( 'NONE',  ( -4.800000000000026468, 12.50000000000000000, -4.676537180435978769 ) ) ;
#22713 = DIRECTION ( 'NONE',  ( 0.000000000000000000, 0.000000000000000000, -1.000000000000000000 ) ) ;
#22714 = EDGE_CURVE ( 'NONE', #92990, #51042, #13579, .T. ) ;
#22715 = DIRECTION ( 'NONE',  ( 0.000000000000000000, 0.000000000000000000, -1.000000000000000000 ) ) ;
#22716 = ADVANCED_FACE ( 'NONE', ( #11657 ), #103245, .T. ) ;
#22717 = DIRECTION ( 'NONE',  ( 0.000000000000000000, -0.000000000000000000, 1.000000000000000000 ) ) ;
#22718 = ADVANCED_FACE ( 'NONE', ( #62067 ), #15386, .T. ) ;
#22719 = EDGE_LOOP ( 'NONE', ( #125222, #124182 ) ) ;
#22720 = ORIENTED_EDGE ( 'NONE', *, *, #126690, .T. ) ;
#22721 = VERTEX_POINT ( 'NONE', #82997 ) ;
#22722 = VECTOR ( 'NONE', #127223, 1000.000000000000000 ) ;
#22723 = ORIENTED_EDGE ( 'NONE', *, *, #128803, .T. ) ;
#22724 = ORIENTED_EDGE ( 'NONE', *, *, #70364, .T. ) ;
#22725 = AXIS2_PLACEMENT_3D ( 'NONE', #21681, #2021, #120524 ) ;
#22726 = CARTESIAN_POINT ( 'NONE',  ( 7.099999999999927702, 2.500000000000000000, 4.922947341949748257 ) ) ;
#22727 = CARTESIAN_POINT ( 'NONE',  ( -2.100000000000033396, 12.50000000000000000, 0.6928203230275494784 ) ) ;
#22729 = EDGE_CURVE ( 'NONE', #5978, #121861, #34300, .T. ) ;
#22728 = EDGE_LOOP ( 'NONE', ( #24457, #122386, #106916, #121313 ) ) ;
#22730 = FACE_BOUND ( 'NONE', #92334, .T. ) ;
#22731 = CARTESIAN_POINT ( 'NONE',  ( 3.149999999999942624, 12.50000000000000000, 6.083687093685483660 ) ) ;
#22732 = EDGE_CURVE ( 'NONE', #97422, #51891, #103911, .T. ) ;
#22733 = EDGE_CURVE ( 'NONE', #21325, #71846, #105295, .T. ) ;
#22734 = ADVANCED_FACE ( 'NONE', ( #122913 ), #122025, .T. ) ;
#22735 = PRESENTATION_LAYER_ASSIGNMENT (  '', '', ( #91668 ) ) ;
#22736 = ORIENTED_EDGE ( 'NONE', *, *, #117043, .F. ) ;
#22737 = DIRECTION ( 'NONE',  ( -0.000000000000000000, -1.000000000000000000, -0.000000000000000000 ) ) ;
#22738 = CARTESIAN_POINT ( 'NONE',  ( -0.8500000000000395017, 2.500000000000000000, 6.495190528383297135 ) ) ;
#22739 = CARTESIAN_POINT ( 'NONE',  ( -5.600000000000023626, 2.500000000000000000, -4.676537180435977881 ) ) ;
#22740 = ORIENTED_EDGE ( 'NONE', *, *, #108916, .T. ) ;
#22741 = AXIS2_PLACEMENT_3D ( 'NONE', #86987, #115803, #36625 ) ;
#22742 = CARTESIAN_POINT ( 'NONE',  ( 15.59999999999988951, 2.500000000000000000, 0.3464101615137735735 ) ) ;
#22743 = EDGE_CURVE ( 'NONE', #16412, #51103, #113708, .T. ) ;
#22745 = ORIENTED_EDGE ( 'NONE', *, *, #42167, .T. ) ;
#22744 = CIRCLE ( 'NONE', #8134, 0.06509327318403745899 ) ;
#22746 = ORIENTED_EDGE ( 'NONE', *, *, #42174, .T. ) ;
#22747 = ORIENTED_EDGE ( 'NONE', *, *, #122767, .T. ) ;
#22748 = CARTESIAN_POINT ( 'NONE',  ( 11.84999999999990372, 2.500000000000000000, -6.841600689897078702 ) ) ;
#22749 = DIRECTION ( 'NONE',  ( 1.000000000000000000, -0.000000000000000000, -0.000000000000000000 ) ) ;
#22750 = DIRECTION ( 'NONE',  ( -0.000000000000000000, 1.000000000000000000, -0.000000000000000000 ) ) ;
#22751 = VECTOR ( 'NONE', #65543, 1000.000000000000000 ) ;
#22752 = EDGE_LOOP ( 'NONE', ( #110963, #37650 ) ) ;
#22753 = DIRECTION ( 'NONE',  ( 0.000000000000000000, 0.000000000000000000, 1.000000000000000000 ) ) ;
#22754 = CARTESIAN_POINT ( 'NONE',  ( 3.549999999999941203, 2.500000000000000000, 6.148780366869520897 ) ) ;
#22756 = AXIS2_PLACEMENT_3D ( 'NONE', #15072, #3357, #73374 ) ;
#22755 = DIRECTION ( 'NONE',  ( -0.000000000000000000, -1.000000000000000000, -0.000000000000000000 ) ) ;
#22757 = DIRECTION ( 'NONE',  ( 0.000000000000000000, -0.000000000000000000, 1.000000000000000000 ) ) ;
#22758 = ORIENTED_EDGE ( 'NONE', *, *, #80459, .T. ) ;
#22759 = AXIS2_PLACEMENT_3D ( 'NONE', #14786, #82932, #34482 ) ;
#22760 = DIRECTION ( 'NONE',  ( -4.274815082592931898E-19, -0.9999939076577903929, -0.003490651415223739937 ) ) ;
#22761 = EDGE_CURVE ( 'NONE', #105604, #51184, #61428, .T. ) ;
#22762 = ORIENTED_EDGE ( 'NONE', *, *, #96682, .F. ) ;
#22763 = CARTESIAN_POINT ( 'NONE',  ( 11.44999999999990514, 2.500000000000000000, 2.511473670974873507 ) ) ;
#22765 = CIRCLE ( 'NONE', #83389, 0.1000000000000002554 ) ;
#22764 = AXIS2_PLACEMENT_3D ( 'NONE', #55459, #116294, #67174 ) ;
#22766 = ORIENTED_EDGE ( 'NONE', *, *, #2043, .T. ) ;
#22767 = ORIENTED_EDGE ( 'NONE', *, *, #47594, .T. ) ;
#22768 = DIRECTION ( 'NONE',  ( 0.000000000000000000, -0.000000000000000000, 1.000000000000000000 ) ) ;
#22769 = DIRECTION ( 'NONE',  ( 0.000000000000000000, 1.000000000000000000, 0.000000000000000000 ) ) ;
#22770 = FACE_OUTER_BOUND ( 'NONE', #96068, .T. ) ;
#22771 = CARTESIAN_POINT ( 'NONE',  ( 12.69999999999990159, 2.500000000000000000, -4.083716857408426826 ) ) ;
#22772 = PLANE ( 'NONE',  #103979 ) ;
#22773 = ORIENTED_EDGE ( 'NONE', *, *, #8325, .T. ) ;
#22774 = ORIENTED_EDGE ( 'NONE', *, *, #3079, .T. ) ;
#22775 = DIRECTION ( 'NONE',  ( 0.000000000000000000, 0.000000000000000000, -1.000000000000000000 ) ) ;
#22776 = ADVANCED_FACE ( 'NONE', ( #22793 ), #83635, .T. ) ;
#22777 = CARTESIAN_POINT ( 'NONE',  ( 10.64999999999991331, 12.50000000000000000, -2.576566944158915184 ) ) ;
#22778 = FACE_OUTER_BOUND ( 'NONE', #68996, .T. ) ;
#22780 = VERTEX_POINT ( 'NONE', #71885 ) ;
#22779 = VECTOR ( 'NONE', #52977, 1000.000000000000000 ) ;
#22781 = ORIENTED_EDGE ( 'NONE', *, *, #124815, .F. ) ;
#22782 = CARTESIAN_POINT ( 'NONE',  ( -9.400000000000007461, 12.50000000000000000, 4.676537180435972552 ) ) ;
#22783 = VERTEX_POINT ( 'NONE', #111807 ) ;
#22784 = CARTESIAN_POINT ( 'NONE',  ( -4.350000000000023626, 12.50000000000000000, -2.511473670974877948 ) ) ;
#22785 = FACE_OUTER_BOUND ( 'NONE', #47548, .T. ) ;
#22786 = VECTOR ( 'NONE', #125655, 1000.000000000000000 ) ;
#22788 = DIRECTION ( 'NONE',  ( -4.274815082592931898E-19, -0.9999939076577903929, -0.003490651415223739937 ) ) ;
#22787 = AXIS2_PLACEMENT_3D ( 'NONE', #127910, #38252, #78174 ) ;
#22789 = ORIENTED_EDGE ( 'NONE', *, *, #77206, .T. ) ;
#22790 = CARTESIAN_POINT ( 'NONE',  ( 13.34999999999990017, 12.50000000000000000, 2.099970236277060032 ) ) ;
#22791 = CARTESIAN_POINT ( 'NONE',  ( -4.150000000000028777, 12.50000000000000000, -5.867463478539787225 ) ) ;
#22792 = CARTESIAN_POINT ( 'NONE',  ( -1.250000000000035749, 2.500000000000000000, -2.857883832488653741 ) ) ;
#22793 = FACE_OUTER_BOUND ( 'NONE', #30913, .T. ) ;
#22794 = ADVANCED_FACE ( 'NONE', ( #22151 ), #2464, .T. ) ;
#22795 = LINE ( 'NONE', #94726, #41579 ) ;
#22796 = VECTOR ( 'NONE', #17289, 1000.000000000000227 ) ;
#22797 = ORIENTED_EDGE ( 'NONE', *, *, #79968, .F. ) ;
#22798 = VECTOR ( 'NONE', #49031, 1000.000000000000000 ) ;
#22800 = DIRECTION ( 'NONE',  ( -0.000000000000000000, 1.000000000000000000, -0.000000000000000000 ) ) ;
#22799 = AXIS2_PLACEMENT_3D ( 'NONE', #118230, #98564, #77649 ) ;
#22801 = DIRECTION ( 'NONE',  ( 0.000000000000000000, 0.000000000000000000, -1.000000000000000000 ) ) ;
#22802 = ORIENTED_EDGE ( 'NONE', *, *, #6834, .T. ) ;
#22803 = VERTEX_POINT ( 'NONE', #106484 ) ;
#22804 = CARTESIAN_POINT ( 'NONE',  ( 187.3802083336747444, 4.367472073101515306, 7.564683531250000925 ) ) ;
#22805 = CARTESIAN_POINT ( 'NONE',  ( 0.8499999999999553468, 12.50000000000000000, 1.472243186433545459 ) ) ;
#22806 = LINE ( 'NONE', #1843, #116726 ) ;
#22807 = DIRECTION ( 'NONE',  ( 0.000000000000000000, 0.000000000000000000, 1.000000000000000000 ) ) ;
#22808 = CARTESIAN_POINT ( 'NONE',  ( -12.89999999999999147, 12.50000000000000000, 5.022947341949748790 ) ) ;
#22809 = AXIS2_PLACEMENT_3D ( 'NONE', #2495, #32654, #42461 ) ;
#22810 = CARTESIAN_POINT ( 'NONE',  ( 4.149999999999936406, 2.500000000000000000, 6.495190528383297135 ) ) ;
#22811 = CARTESIAN_POINT ( 'NONE',  ( 9.149999999999920419, 12.50000000000000000, -5.737276932171712751 ) ) ;
#22812 = LINE ( 'NONE', #11675, #74947 ) ;
#22813 = DIRECTION ( 'NONE',  ( -0.000000000000000000, 1.000000000000000000, -0.000000000000000000 ) ) ;
#22814 = VECTOR ( 'NONE', #50583, 1000.000000000000000 ) ;
#22815 = ORIENTED_EDGE ( 'NONE', *, *, #63182, .T. ) ;
#22816 = EDGE_LOOP ( 'NONE', ( #35394, #27622 ) ) ;
#22817 = EDGE_CURVE ( 'NONE', #12562, #10727, #73998, .T. ) ;
#22818 = ORIENTED_EDGE ( 'NONE', *, *, #120326, .F. ) ;
#22819 = CIRCLE ( 'NONE', #56140, 0.09999999999999982514 ) ;
#22820 = ORIENTED_EDGE ( 'NONE', *, *, #37937, .T. ) ;
#22821 = PLANE ( 'NONE',  #88122 ) ;
#22822 = CARTESIAN_POINT ( 'NONE',  ( -4.550000000000022915, 12.50000000000000000, 2.165063509461097713 ) ) ;
#22823 = ORIENTED_EDGE ( 'NONE', *, *, #118392, .F. ) ;
#22824 = DIRECTION ( 'NONE',  ( 0.000000000000000000, 0.000000000000000000, -1.000000000000000000 ) ) ;
#22825 = CARTESIAN_POINT ( 'NONE',  ( 9.149999999999918643, 2.500000000000000000, -6.395190528383301931 ) ) ;
#22827 = ORIENTED_EDGE ( 'NONE', *, *, #82224, .T. ) ;
#22826 = CARTESIAN_POINT ( 'NONE',  ( 12.29999999999990656, 2.500000000000000000, -4.576537180435977348 ) ) ;
#22828 = ADVANCED_FACE ( 'NONE', ( #6320 ), #74451, .T. ) ;
#22829 = EDGE_CURVE ( 'NONE', #31342, #70284, #51028, .T. ) ;
#22830 = ADVANCED_FACE ( 'NONE', ( #44999 ), #9149, .T. ) ;
#22831 = CARTESIAN_POINT ( 'NONE',  ( -12.29999999999999538, 2.500000000000000000, 4.676537180435972552 ) ) ;
#22832 = EDGE_CURVE ( 'NONE', #69735, #87864, #32159, .T. ) ;
#22833 = CIRCLE ( 'NONE', #104289, 0.06509327318403745899 ) ;
#22834 = CARTESIAN_POINT ( 'NONE',  ( -0.4500000000000402012, 2.500000000000000000, 6.595190528383296780 ) ) ;
#22835 = VERTEX_POINT ( 'NONE', #37112 ) ;
#22836 = CIRCLE ( 'NONE', #83472, 0.1000000000000002554 ) ;
#22837 = ORIENTED_EDGE ( 'NONE', *, *, #109988, .F. ) ;
#22838 = VERTEX_POINT ( 'NONE', #107111 ) ;
#22839 = VERTEX_POINT ( 'NONE', #45645 ) ;
#22840 = DIRECTION ( 'NONE',  ( -0.000000000000000000, -1.000000000000000000, -0.000000000000000000 ) ) ;
#22841 = AXIS2_PLACEMENT_3D ( 'NONE', #110943, #80224, #110320 ) ;
#22842 = EDGE_CURVE ( 'NONE', #123328, #100183, #38419, .T. ) ;
#22843 = DIRECTION ( 'NONE',  ( 0.000000000000000000, 1.000000000000000000, 0.000000000000000000 ) ) ;
#22844 = DIRECTION ( 'NONE',  ( 0.000000000000000000, 0.000000000000000000, -1.000000000000000000 ) ) ;
#22845 = EDGE_CURVE ( 'NONE', #117628, #16039, #7624, .T. ) ;
#22846 = DIRECTION ( 'NONE',  ( -0.000000000000000000, 1.000000000000000000, -0.000000000000000000 ) ) ;
#22848 = EDGE_LOOP ( 'NONE', ( #98458, #84799, #16524, #36367 ) ) ;
#22847 = ADVANCED_FACE ( 'NONE', ( #75093 ), #101189, .T. ) ;
#22850 = AXIS2_PLACEMENT_3D ( 'NONE', #102681, #54869, #75171 ) ;
#22849 = AXIS2_PLACEMENT_3D ( 'NONE', #33447, #111999, #122467 ) ;
#22851 = CARTESIAN_POINT ( 'NONE',  ( -4.350000000000023626, 2.500000000000000000, 1.718653347947321386 ) ) ;
#22852 = ORIENTED_EDGE ( 'NONE', *, *, #52462, .T. ) ;
#22853 = LINE ( 'NONE', #53589, #91456 ) ;
#22854 = AXIS2_PLACEMENT_3D ( 'NONE', #67107, #76968, #97246 ) ;
#22855 = FACE_OUTER_BOUND ( 'NONE', #123452, .T. ) ;
#22856 = CARTESIAN_POINT ( 'NONE',  ( 179.5000000000000000, 1.375000000000002442, -6.000000000000000888 ) ) ;
#22857 = ORIENTED_EDGE ( 'NONE', *, *, #99591, .F. ) ;
#22859 = CONICAL_SURFACE ( 'NONE', #66738, 0.1000000000000000472, 0.003490658503988666988 ) ;
#22858 = CIRCLE ( 'NONE', #110566, 0.06509327318403745899 ) ;
#22860 = ORIENTED_EDGE ( 'NONE', *, *, #12365, .F. ) ;
#22861 = ORIENTED_EDGE ( 'NONE', *, *, #13016, .F. ) ;
#22862 = DIRECTION ( 'NONE',  ( 0.000000000000000000, 1.000000000000000000, 0.000000000000000000 ) ) ;
#22863 = DIRECTION ( 'NONE',  ( 0.000000000000000000, 0.000000000000000000, 1.000000000000000000 ) ) ;
#22864 = DIRECTION ( 'NONE',  ( 0.000000000000000000, 0.000000000000000000, 1.000000000000000000 ) ) ;
#22865 = FACE_BOUND ( 'NONE', #65182, .T. ) ;
#22866 = DIRECTION ( 'NONE',  ( 0.000000000000000000, 0.000000000000000000, 1.000000000000000000 ) ) ;
#22867 = DIRECTION ( 'NONE',  ( 0.000000000000000000, 0.000000000000000000, -1.000000000000000000 ) ) ;
#22868 = DIRECTION ( 'NONE',  ( -0.000000000000000000, -1.000000000000000000, -0.000000000000000000 ) ) ;
#22869 = AXIS2_PLACEMENT_3D ( 'NONE', #4183, #126563, #25773 ) ;
#22870 = CYLINDRICAL_SURFACE ( 'NONE', #88086, 7.700000000000000178 ) ;
#22871 = CARTESIAN_POINT ( 'NONE',  ( -6.250000000000017764, 12.50000000000000000, 2.857883832488649301 ) ) ;
#22872 = LINE ( 'NONE', #43163, #97119 ) ;
#22873 = EDGE_LOOP ( 'NONE', ( #56439, #75412, #6916, #106820 ) ) ;
#22874 = DIRECTION ( 'NONE',  ( 0.000000000000000000, 0.000000000000000000, 1.000000000000000000 ) ) ;
#22875 = ORIENTED_EDGE ( 'NONE', *, *, #46174, .F. ) ;
#22876 = VERTEX_POINT ( 'NONE', #35185 ) ;
#22877 = DIRECTION ( 'NONE',  ( 0.000000000000000000, 0.000000000000000000, 1.000000000000000000 ) ) ;
#22878 = FACE_OUTER_BOUND ( 'NONE', #48524, .T. ) ;
#22879 = FACE_BOUND ( 'NONE', #1916, .T. ) ;
#22880 = CARTESIAN_POINT ( 'NONE',  ( 2.699999999999944666, 2.500000000000000000, 4.676537180435972552 ) ) ;
#22881 = EDGE_CURVE ( 'NONE', #16084, #92620, #124195, .T. ) ;
#22882 = ADVANCED_FACE ( 'NONE', ( #65250 ), #78211, .T. ) ;
#22883 = ORIENTED_EDGE ( 'NONE', *, *, #60052, .T. ) ;
#22884 = CARTESIAN_POINT ( 'NONE',  ( 179.5000000000000000, 0.9999999999999985567, 7.634788798650556707 ) ) ;
#22885 = DIRECTION ( 'NONE',  ( -4.274815082592931898E-19, -0.9999939076577903929, -0.003490651415223739937 ) ) ;
#22886 = CONICAL_SURFACE ( 'NONE', #119019, 0.09999999999999982514, 0.003490658503988666988 ) ;
#22887 = ORIENTED_EDGE ( 'NONE', *, *, #42173, .F. ) ;
#22888 = DIRECTION ( 'NONE',  ( 0.000000000000000000, 1.000000000000000000, 0.000000000000000000 ) ) ;
#22889 = DIRECTION ( 'NONE',  ( 0.000000000000000000, 0.000000000000000000, 1.000000000000000000 ) ) ;
#22890 = EDGE_CURVE ( 'NONE', #17735, #98528, #24707, .T. ) ;
#22891 = VECTOR ( 'NONE', #49391, 1000.000000000000000 ) ;
#22892 = CIRCLE ( 'NONE', #96037, 0.06509327318403745899 ) ;
#22893 = EDGE_LOOP ( 'NONE', ( #114673, #125285, #102383, #111829 ) ) ;
#22894 = LINE ( 'NONE', #51703, #29792 ) ;
#22895 = DIRECTION ( 'NONE',  ( -0.000000000000000000, -1.000000000000000000, -0.000000000000000000 ) ) ;
#22896 = EDGE_LOOP ( 'NONE', ( #1937, #124710, #118087, #98008 ) ) ;
#22897 = DIRECTION ( 'NONE',  ( 0.000000000000000000, 1.000000000000000000, 0.000000000000000000 ) ) ;
#22898 = CARTESIAN_POINT ( 'NONE',  ( -4.200000000000029488, 12.50000000000000000, -4.395220292106239768 ) ) ;
#22899 = CARTESIAN_POINT ( 'NONE',  ( -4.800000000000022915, 2.500000000000000000, -0.4464101615137783252 ) ) ;
#22900 = AXIS2_PLACEMENT_3D ( 'NONE', #55898, #56539, #85986 ) ;
#22901 = ORIENTED_EDGE ( 'NONE', *, *, #26548, .T. ) ;
#22902 = EDGE_LOOP ( 'NONE', ( #29509, #125078, #19093, #116108 ) ) ;
#22903 = DIRECTION ( 'NONE',  ( 0.000000000000000000, 0.000000000000000000, 1.000000000000000000 ) ) ;
#22904 = ORIENTED_EDGE ( 'NONE', *, *, #49435, .T. ) ;
#22905 = DIRECTION ( 'NONE',  ( 0.000000000000000000, -0.000000000000000000, 1.000000000000000000 ) ) ;
#22906 = PLANE ( 'NONE',  #93298 ) ;
#22907 = VERTEX_POINT ( 'NONE', #85551 ) ;
#22908 = DIRECTION ( 'NONE',  ( -0.000000000000000000, -1.000000000000000000, -0.000000000000000000 ) ) ;
#22909 = CARTESIAN_POINT ( 'NONE',  ( -3.950000000000029932, 2.500000000000000000, -6.248780366869526759 ) ) ;
#22910 = CARTESIAN_POINT ( 'NONE',  ( -6.249999999999984901, 2.500000000000000000, -6.595190528383302109 ) ) ;
#22911 = LINE ( 'NONE', #51092, #50709 ) ;
#22912 = AXIS2_PLACEMENT_3D ( 'NONE', #3455, #92473, #54478 ) ;
#22913 = LINE ( 'NONE', #62831, #59996 ) ;
#22914 = ORIENTED_EDGE ( 'NONE', *, *, #110875, .T. ) ;
#22915 = ORIENTED_EDGE ( 'NONE', *, *, #43968, .T. ) ;
#22916 = CARTESIAN_POINT ( 'NONE',  ( -8.350000000000008527, 12.50000000000000000, 7.253104124594885960 ) ) ;
#22917 = ORIENTED_EDGE ( 'NONE', *, *, #91845, .F. ) ;
#22918 = EDGE_CURVE ( 'NONE', #56262, #103079, #77022, .T. ) ;
#22919 = FACE_OUTER_BOUND ( 'NONE', #43789, .T. ) ;
#22921 = ORIENTED_EDGE ( 'NONE', *, *, #124956, .F. ) ;
#22920 = ORIENTED_EDGE ( 'NONE', *, *, #119566, .F. ) ;
#22922 = ORIENTED_EDGE ( 'NONE', *, *, #102325, .F. ) ;
#22923 = CIRCLE ( 'NONE', #12435, 0.06509327318403741736 ) ;
#22924 = CARTESIAN_POINT ( 'NONE',  ( 5.799999999999933209, 12.50000000000000000, -2.385244779468109755E-15 ) ) ;
#22925 = CARTESIAN_POINT ( 'NONE',  ( -13.09999999999999254, 2.500000000000000000, 0.3464101615137777923 ) ) ;
#22926 = FACE_OUTER_BOUND ( 'NONE', #33681, .T. ) ;
#22928 = AXIS2_PLACEMENT_3D ( 'NONE', #65988, #127500, #7050 ) ;
#22927 = CONICAL_SURFACE ( 'NONE', #129557, 0.1000000000000002554, 0.003490658503988666988 ) ;
#22929 = CARTESIAN_POINT ( 'NONE',  ( -2.900000000000029221, 12.50000000000000000, -2.276824562219559311E-15 ) ) ;
#22930 = CARTESIAN_POINT ( 'NONE',  ( 184.7812500006828031, 0.000000000000000000, 7.700000000000000178 ) ) ;
#22931 = CARTESIAN_POINT ( 'NONE',  ( -7.100000000000013856, 2.500000000000000000, 3.737306695894644371 ) ) ;
#22932 = ADVANCED_FACE ( 'NONE', ( #105189 ), #21780, .T. ) ;
#22933 = DIRECTION ( 'NONE',  ( 0.000000000000000000, 1.000000000000000000, 0.000000000000000000 ) ) ;
#22934 = DIRECTION ( 'NONE',  ( -0.000000000000000000, -1.000000000000000000, -0.000000000000000000 ) ) ;
#22935 = AXIS2_PLACEMENT_3D ( 'NONE', #72316, #33045, #123337 ) ;
#22936 = ADVANCED_FACE ( 'NONE', ( #116929 ), #94926, .T. ) ;
#22937 = LINE ( 'NONE', #119836, #108354 ) ;
#22938 = AXIS2_PLACEMENT_3D ( 'NONE', #2693, #82576, #50512 ) ;
#22939 = ORIENTED_EDGE ( 'NONE', *, *, #74667, .F. ) ;
#22940 = CARTESIAN_POINT ( 'NONE',  ( -4.550000000000022915, 2.500000000000000000, 6.395190528383296602 ) ) ;
#22941 = ORIENTED_EDGE ( 'NONE', *, *, #80921, .F. ) ;
#22942 = EDGE_CURVE ( 'NONE', #26576, #80133, #71954, .T. ) ;
#22943 = ORIENTED_EDGE ( 'NONE', *, *, #125058, .T. ) ;
#22944 = DIRECTION ( 'NONE',  ( 0.000000000000000000, 0.000000000000000000, 1.000000000000000000 ) ) ;
#22945 = FACE_OUTER_BOUND ( 'NONE', #26772, .T. ) ;
#22946 = DIRECTION ( 'NONE',  ( 0.000000000000000000, 1.000000000000000000, 0.000000000000000000 ) ) ;
#22947 = DIRECTION ( 'NONE',  ( -0.000000000000000000, -1.000000000000000000, -0.000000000000000000 ) ) ;
#22948 = CARTESIAN_POINT ( 'NONE',  ( -14.39999999999998614, 12.50000000000000000, -0.3464101615137760715 ) ) ;
#22949 = CARTESIAN_POINT ( 'NONE',  ( 6.449999999999931788, 2.500000000000000000, -6.048780366869526581 ) ) ;
#22950 = LINE ( 'NONE', #94254, #96899 ) ;
#22951 = EDGE_LOOP ( 'NONE', ( #127397, #59746, #19976, #20206 ) ) ;
#22952 = ORIENTED_EDGE ( 'NONE', *, *, #68195, .T. ) ;
#22953 = AXIS2_PLACEMENT_3D ( 'NONE', #20348, #40000, #79907 ) ;
#22955 = ORIENTED_EDGE ( 'NONE', *, *, #96702, .T. ) ;
#22954 = AXIS2_PLACEMENT_3D ( 'NONE', #35836, #95402, #122935 ) ;
#22956 = ADVANCED_FACE ( 'NONE', ( #65906 ), #928, .T. ) ;
#22957 = VERTEX_POINT ( 'NONE', #59992 ) ;
#22958 = ORIENTED_EDGE ( 'NONE', *, *, #20919, .T. ) ;
#22960 = AXIS2_PLACEMENT_3D ( 'NONE', #103465, #102179, #72084 ) ;
#22959 = DIRECTION ( 'NONE',  ( 0.000000000000000000, -0.000000000000000000, 1.000000000000000000 ) ) ;
#22961 = LINE ( 'NONE', #72704, #104166 ) ;
#22962 = VECTOR ( 'NONE', #67686, 1000.000000000000000 ) ;
#22963 = EDGE_CURVE ( 'NONE', #59055, #74808, #67843, .T. ) ;
#22964 = DIRECTION ( 'NONE',  ( 0.000000000000000000, 0.000000000000000000, -1.000000000000000000 ) ) ;
#22965 = CARTESIAN_POINT ( 'NONE',  ( 4.349999999999937472, 12.50000000000000000, 6.841600689897072485 ) ) ;
#22966 = CARTESIAN_POINT ( 'NONE',  ( 17.50000000000000000, -0.8333333333333350357, 4.000000000000001776 ) ) ;
#22967 = ORIENTED_EDGE ( 'NONE', *, *, #101603, .F. ) ;
#22968 = CARTESIAN_POINT ( 'NONE',  ( 129.5000000000000000, -1.500000000000000000, 2.598076211353316900 ) ) ;
#22969 = EDGE_CURVE ( 'NONE', #59797, #40211, #113805, .T. ) ;
#22970 = ADVANCED_FACE ( 'NONE', ( #100521, #58040 ), #29860, .F. ) ;
#22971 = CARTESIAN_POINT ( 'NONE',  ( -2.100000000000033840, 2.500000000000000000, 5.022947341949748790 ) ) ;
#22972 = ADVANCED_FACE ( 'NONE', ( #129377 ), #15487, .T. ) ;
#22973 = CARTESIAN_POINT ( 'NONE',  ( -9.150000000000009237, 12.50000000000000000, -2.792790559304616504 ) ) ;
#22974 = ADVANCED_FACE ( 'NONE', ( #117559 ), #21875, .T. ) ;
#22975 = DIRECTION ( 'NONE',  ( -0.000000000000000000, 1.000000000000000000, -0.000000000000000000 ) ) ;
#22976 = CONICAL_SURFACE ( 'NONE', #56408, 0.09999999999999982514, 0.003490658503988666988 ) ;
#22977 = EDGE_LOOP ( 'NONE', ( #16230, #17688, #111061, #123092 ) ) ;
#22978 = CONICAL_SURFACE ( 'NONE', #68933, 0.09999999999999982514, 0.003490658503988666988 ) ;
#22979 = VERTEX_POINT ( 'NONE', #118884 ) ;
#22981 = EDGE_LOOP ( 'NONE', ( #69784, #102780 ) ) ;
#22980 = EDGE_CURVE ( 'NONE', #101321, #22212, #74091, .T. ) ;
#22982 = CARTESIAN_POINT ( 'NONE',  ( -0.8500000000000390576, 2.500000000000000000, -2.165063509461101710 ) ) ;
#22983 = ADVANCED_FACE ( 'NONE', ( #87471 ), #9577, .T. ) ;
#22984 = AXIS2_PLACEMENT_3D ( 'NONE', #97523, #16364, #67388 ) ;
#22985 = DIRECTION ( 'NONE',  ( 0.000000000000000000, 0.000000000000000000, 1.000000000000000000 ) ) ;
#22986 = DIRECTION ( 'NONE',  ( -4.274815082592931898E-19, -0.9999939076577903929, -0.003490651415223739937 ) ) ;
#22987 = EDGE_CURVE ( 'NONE', #99389, #81036, #107772, .T. ) ;
#22988 = ADVANCED_FACE ( 'NONE', ( #89421 ), #9248, .T. ) ;
#22989 = CIRCLE ( 'NONE', #98188, 0.06509327318403745899 ) ;
#22990 = ORIENTED_EDGE ( 'NONE', *, *, #50638, .F. ) ;
#22991 = DIRECTION ( 'NONE',  ( 0.000000000000000000, 0.000000000000000000, 1.000000000000000000 ) ) ;
#22992 = DIRECTION ( 'NONE',  ( 0.000000000000000000, 0.000000000000000000, 1.000000000000000000 ) ) ;
#22993 = ADVANCED_FACE ( 'NONE', ( #40336 ), #92883, .T. ) ;
#22994 = DIRECTION ( 'NONE',  ( -4.274815082592931898E-19, -0.9999939076577903929, -0.003490651415223739937 ) ) ;
#22995 = CARTESIAN_POINT ( 'NONE',  ( -7.500000000000011546, 12.50000000000000000, 3.637306695894644726 ) ) ;
#22996 = EDGE_CURVE ( 'NONE', #65538, #75669, #32257, .T. ) ;
#22997 = DIRECTION ( 'NONE',  ( 1.000000000000000000, 0.000000000000000000, 0.000000000000000000 ) ) ;
#22998 = EDGE_LOOP ( 'NONE', ( #68868, #118580, #95255, #90367 ) ) ;
#22999 = VERTEX_POINT ( 'NONE', #48208 ) ;
#23000 = CARTESIAN_POINT ( 'NONE',  ( 3.949999999999938893, 2.500000000000000000, 6.048780366869520364 ) ) ;
#23001 = DIRECTION ( 'NONE',  ( -0.000000000000000000, 1.000000000000000000, -0.000000000000000000 ) ) ;
#23002 = CARTESIAN_POINT ( 'NONE',  ( 0.8499999999999527933, 2.500000000000000000, 7.188010851410848723 ) ) ;
#23003 = CARTESIAN_POINT ( 'NONE',  ( -12.89999999999999147, 12.50000000000000000, 5.022947341949748790 ) ) ;
#23004 = EDGE_LOOP ( 'NONE', ( #124572, #104293, #39056, #89225 ) ) ;
#23005 = ORIENTED_EDGE ( 'NONE', *, *, #45210, .F. ) ;
#23007 = VECTOR ( 'NONE', #108561, 1000.000000000000000 ) ;
#23006 = CARTESIAN_POINT ( 'NONE',  ( 3.949999999999940670, 2.500000000000000000, 1.718653347947321386 ) ) ;
#23008 = CARTESIAN_POINT ( 'NONE',  ( 11.84999999999990372, 2.500000000000000000, -6.841600689897078702 ) ) ;
#23009 = LINE ( 'NONE', #18171, #7940 ) ;
#23010 = DIRECTION ( 'NONE',  ( 0.000000000000000000, 0.000000000000000000, 1.000000000000000000 ) ) ;
#23011 = ORIENTED_EDGE ( 'NONE', *, *, #111641, .F. ) ;
#23012 = CARTESIAN_POINT ( 'NONE',  ( 14.59999999999989484, 2.500000000000000000, 0.5928203230275495006 ) ) ;
#23013 = VECTOR ( 'NONE', #46192, 1000.000000000000000 ) ;
#23014 = DIRECTION ( 'NONE',  ( 0.000000000000000000, 0.000000000000000000, -1.000000000000000000 ) ) ;
#23015 = ORIENTED_EDGE ( 'NONE', *, *, #121374, .T. ) ;
#23016 = CARTESIAN_POINT ( 'NONE',  ( -4.600000000000024514, 2.500000000000000000, 0.5928203230275495006 ) ) ;
#23017 = ORIENTED_EDGE ( 'NONE', *, *, #56331, .F. ) ;
#23018 = DIRECTION ( 'NONE',  ( 0.000000000000000000, 0.000000000000000000, 1.000000000000000000 ) ) ;
#23020 = CIRCLE ( 'NONE', #87752, 0.06509327318403745899 ) ;
#23019 = VECTOR ( 'NONE', #101036, 1000.000000000000000 ) ;
#23021 = ADVANCED_FACE ( 'NONE', ( #128062, #28573 ), #38412, .T. ) ;
#23022 = EDGE_LOOP ( 'NONE', ( #38633, #25283, #75350 ) ) ;
#23023 = FACE_OUTER_BOUND ( 'NONE', #17482, .T. ) ;
#23024 = CARTESIAN_POINT ( 'NONE',  ( 12.04999999999990479, 2.500000000000000000, 2.165063509461097713 ) ) ;
#23025 = EDGE_CURVE ( 'NONE', #113580, #111172, #18742, .T. ) ;
#23026 = ORIENTED_EDGE ( 'NONE', *, *, #61421, .T. ) ;
#23027 = ORIENTED_EDGE ( 'NONE', *, *, #23953, .F. ) ;
#23028 = CARTESIAN_POINT ( 'NONE',  ( 186.7968750003414300, 8.734944146203032389, 5.348610694689227483E-16 ) ) ;
#23029 = CARTESIAN_POINT ( 'NONE',  ( 11.44999999999990514, 2.500000000000000000, 2.611473670974873151 ) ) ;
#23030 = CARTESIAN_POINT ( 'NONE',  ( 186.7135416670080872, 4.367472073101518859, -7.564683531249999149 ) ) ;
#23031 = FACE_OUTER_BOUND ( 'NONE', #48661, .T. ) ;
#23032 = CARTESIAN_POINT ( 'NONE',  ( 5.849999999999935696, 12.50000000000000000, -7.188010851410854052 ) ) ;
#23033 = FACE_OUTER_BOUND ( 'NONE', #123843, .T. ) ;
#23034 = CARTESIAN_POINT ( 'NONE',  ( -2.100000000000033396, 12.50000000000000000, -5.022947341949754119 ) ) ;
#23035 = DIRECTION ( 'NONE',  ( 0.000000000000000000, 1.000000000000000000, 0.000000000000000000 ) ) ;
#23036 = DIRECTION ( 'NONE',  ( 0.000000000000000000, 0.000000000000000000, 1.000000000000000000 ) ) ;
#23037 = AXIS2_PLACEMENT_3D ( 'NONE', #65412, #105350, #43228 ) ;
#23038 = AXIS2_PLACEMENT_3D ( 'NONE', #75518, #26442, #74896 ) ;
#23039 = VERTEX_POINT ( 'NONE', #58680 ) ;
#23040 = EDGE_LOOP ( 'NONE', ( #9289, #126682, #50987, #36598 ) ) ;
#23041 = LINE ( 'NONE', #81320, #125980 ) ;
#23042 = ORIENTED_EDGE ( 'NONE', *, *, #1122, .F. ) ;
#23043 = CARTESIAN_POINT ( 'NONE',  ( -9.150000000000005684, 2.500000000000000000, 5.902370205355745192 ) ) ;
#23044 = CARTESIAN_POINT ( 'NONE',  ( -12.89999999999999147, 2.500000000000000000, 4.230127018922196669 ) ) ;
#23045 = CARTESIAN_POINT ( 'NONE',  ( -4.350000000000023626, 2.500000000000000000, 2.411473670974873862 ) ) ;
#23047 = ORIENTED_EDGE ( 'NONE', *, *, #50173, .T. ) ;
#23046 = EDGE_LOOP ( 'NONE', ( #50099, #6005, #100450, #13536 ) ) ;
#23048 = FACE_BOUND ( 'NONE', #47718, .T. ) ;
#23049 = EDGE_LOOP ( 'NONE', ( #48460, #8594 ) ) ;
#23050 = DIRECTION ( 'NONE',  ( 0.000000000000000000, 0.000000000000000000, 1.000000000000000000 ) ) ;
#23051 = DIRECTION ( 'NONE',  ( 0.000000000000000000, 1.000000000000000000, 0.000000000000000000 ) ) ;
#23052 = VECTOR ( 'NONE', #84320, 1000.000000000000000 ) ;
#23053 = DIRECTION ( 'NONE',  ( -4.274815082592931898E-19, -0.9999939076577903929, -0.003490651415223739937 ) ) ;
#23054 = LINE ( 'NONE', #61704, #84881 ) ;
#23055 = DIRECTION ( 'NONE',  ( -0.000000000000000000, -1.000000000000000000, -0.000000000000000000 ) ) ;
#23056 = FACE_OUTER_BOUND ( 'NONE', #70508, .T. ) ;
#23057 = CARTESIAN_POINT ( 'NONE',  ( 7.499999999999923617, 2.500000000000000000, 0.6928203230275494784 ) ) ;
#23058 = DIRECTION ( 'NONE',  ( 0.000000000000000000, 1.000000000000000000, 0.000000000000000000 ) ) ;
#23059 = DIRECTION ( 'NONE',  ( 0.000000000000000000, 1.000000000000000000, 0.000000000000000000 ) ) ;
#23060 = CARTESIAN_POINT ( 'NONE',  ( -3.749999999999991118, 2.500000000000000000, -2.065063509461102065 ) ) ;
#23061 = AXIS2_PLACEMENT_3D ( 'NONE', #9004, #109133, #105453 ) ;
#23062 = CARTESIAN_POINT ( 'NONE',  ( 2.099999999999949463, 2.500000000000000000, 0.6928203230275494784 ) ) ;
#23064 = EDGE_CURVE ( 'NONE', #73230, #40852, #95027, .T. ) ;
#23063 = AXIS2_PLACEMENT_3D ( 'NONE', #117943, #19082, #120537 ) ;
#23065 = ORIENTED_EDGE ( 'NONE', *, *, #46746, .T. ) ;
#23066 = EDGE_LOOP ( 'NONE', ( #118791, #35039, #81595, #79372 ) ) ;
#23067 = AXIS2_PLACEMENT_3D ( 'NONE', #69186, #79667, #8983 ) ;
#23068 = EDGE_LOOP ( 'NONE', ( #44440, #51233 ) ) ;
#23069 = CARTESIAN_POINT ( 'NONE',  ( 7.949999999999925571, 2.500000000000000000, 2.265063509461097357 ) ) ;
#23070 = EDGE_LOOP ( 'NONE', ( #76319, #6008, #32438, #115294 ) ) ;
#23071 = DIRECTION ( 'NONE',  ( -0.000000000000000000, -1.000000000000000000, -0.000000000000000000 ) ) ;
#23073 = ORIENTED_EDGE ( 'NONE', *, *, #113819, .T. ) ;
#23072 = VERTEX_POINT ( 'NONE', #29230 ) ;
#23074 = EDGE_LOOP ( 'NONE', ( #116389, #113374 ) ) ;
#23075 = CARTESIAN_POINT ( 'NONE',  ( 10.64999999999991331, 2.500000000000000000, -1.818653347947325916 ) ) ;
#23076 = CONICAL_SURFACE ( 'NONE', #74, 0.1000000000000002554, 0.003490658503988666988 ) ;
#23077 = DIRECTION ( 'NONE',  ( -0.000000000000000000, 1.000000000000000000, -0.000000000000000000 ) ) ;
#23078 = DIRECTION ( 'NONE',  ( -0.000000000000000000, -1.000000000000000000, -0.000000000000000000 ) ) ;
#23079 = AXIS2_PLACEMENT_3D ( 'NONE', #76628, #116538, #28172 ) ;
#23080 = CARTESIAN_POINT ( 'NONE',  ( 185.4062500006828031, -8.891194145520236347, -1.633285867636356299E-15 ) ) ;
#23081 = EDGE_CURVE ( 'NONE', #105515, #87409, #90807, .T. ) ;
#23082 = DIRECTION ( 'NONE',  ( -0.000000000000000000, 1.000000000000000000, -0.000000000000000000 ) ) ;
#23083 = EDGE_CURVE ( 'NONE', #4176, #10639, #30528, .T. ) ;
#23084 = VERTEX_POINT ( 'NONE', #11505 ) ;
#23085 = PLANE ( 'NONE',  #41384 ) ;
#23086 = ORIENTED_EDGE ( 'NONE', *, *, #109411, .F. ) ;
#23087 = VERTEX_POINT ( 'NONE', #50789 ) ;
#23088 = EDGE_LOOP ( 'NONE', ( #27769, #59468, #101312, #83603 ) ) ;
#23089 = CARTESIAN_POINT ( 'NONE',  ( -4.800000000000024691, 2.500000000000000000, 0.4464101615137735513 ) ) ;
#23090 = VERTEX_POINT ( 'NONE', #102466 ) ;
#23091 = ADVANCED_FACE ( 'NONE', ( #21992 ), #67819, .T. ) ;
#23092 = ORIENTED_EDGE ( 'NONE', *, *, #113086, .F. ) ;
#23093 = ORIENTED_EDGE ( 'NONE', *, *, #105284, .F. ) ;
#23094 = SURFACE_STYLE_FILL_AREA ( #64931 ) ;
#23095 = CARTESIAN_POINT ( 'NONE',  ( -9.200000000000009948, 2.500000000000000000, -4.230127018922197557 ) ) ;
#23096 = CARTESIAN_POINT ( 'NONE',  ( 186.2812500006828031, 0.000000000000000000, 7.700000000000000178 ) ) ;
#23097 = CARTESIAN_POINT ( 'NONE',  ( -12.09999999999999609, 12.50000000000000000, 4.330127018922196314 ) ) ;
#23098 = DIRECTION ( 'NONE',  ( 0.000000000000000000, 0.000000000000000000, -1.000000000000000000 ) ) ;
#23099 = AXIS2_PLACEMENT_3D ( 'NONE', #19363, #59985, #59337 ) ;
#23100 = CARTESIAN_POINT ( 'NONE',  ( -12.49999999999995914, 12.50000000000000000, 0.06509327318403926310 ) ) ;
#23101 = CIRCLE ( 'NONE', #102, 0.06509327318403745899 ) ;
#23102 = DIRECTION ( 'NONE',  ( 0.000000000000000000, 0.000000000000000000, 1.000000000000000000 ) ) ;
#23103 = EDGE_LOOP ( 'NONE', ( #36300, #59458 ) ) ;
#23104 = DIRECTION ( 'NONE',  ( 0.000000000000000000, 0.000000000000000000, 1.000000000000000000 ) ) ;
#23105 = CIRCLE ( 'NONE', #81584, 0.06509327318403745899 ) ;
#23106 = ORIENTED_EDGE ( 'NONE', *, *, #104554, .T. ) ;
#23107 = ORIENTED_EDGE ( 'NONE', *, *, #1972, .T. ) ;
#23108 = EDGE_LOOP ( 'NONE', ( #101575, #116612, #60474, #14758 ) ) ;
#23109 = DIRECTION ( 'NONE',  ( -0.000000000000000000, -1.000000000000000000, -0.000000000000000000 ) ) ;
#23110 = ADVANCED_FACE ( 'NONE', ( #12775 ), #25977, .T. ) ;
#23111 = CARTESIAN_POINT ( 'NONE',  ( -14.59999999999998366, 12.50000000000000000, 0.6277270498435143509 ) ) ;
#23112 = EDGE_LOOP ( 'NONE', ( #42039, #58868, #36116, #76853 ) ) ;
#23113 = ORIENTED_EDGE ( 'NONE', *, *, #9371, .F. ) ;
#23114 = LINE ( 'NONE', #61772, #20472 ) ;
#23115 = CARTESIAN_POINT ( 'NONE',  ( 195.0435778713738557, 0.000000000000000000, 0.000000000000000000 ) ) ;
#23116 = ADVANCED_FACE ( 'NONE', ( #33103 ), #111646, .T. ) ;
#23117 = DIRECTION ( 'NONE',  ( 0.000000000000000000, 0.000000000000000000, -1.000000000000000000 ) ) ;
#23118 = CARTESIAN_POINT ( 'NONE',  ( 0.7999999999999612976, 2.500000000000000000, -1.084202172485504434E-16 ) ) ;
#23119 = EDGE_CURVE ( 'NONE', #6508, #77652, #121447, .T. ) ;
#23120 = CARTESIAN_POINT ( 'NONE',  ( -8.350000000000012079, 2.500000000000000000, 1.572243186433545548 ) ) ;
#23121 = VERTEX_POINT ( 'NONE', #122114 ) ;
#23122 = CARTESIAN_POINT ( 'NONE',  ( 2.049999999999948308, 2.500000000000000000, 6.495190528383297135 ) ) ;
#23123 = EDGE_CURVE ( 'NONE', #116790, #105625, #126324, .T. ) ;
#23124 = EDGE_CURVE ( 'NONE', #110412, #90838, #69884, .T. ) ;
#23125 = EDGE_CURVE ( 'NONE', #57799, #7472, #40991, .T. ) ;
#23126 = EDGE_LOOP ( 'NONE', ( #67609, #87770 ) ) ;
#23127 = FACE_OUTER_BOUND ( 'NONE', #69021, .T. ) ;
#23128 = AXIS2_PLACEMENT_3D ( 'NONE', #126473, #106809, #17786 ) ;
#23129 = DIRECTION ( 'NONE',  ( -0.000000000000000000, -1.000000000000000000, -0.000000000000000000 ) ) ;
#23130 = AXIS2_PLACEMENT_3D ( 'NONE', #33868, #6317, #38410 ) ;
#23131 = EDGE_CURVE ( 'NONE', #109488, #19106, #92643, .T. ) ;
#23132 = CARTESIAN_POINT ( 'NONE',  ( 187.0833333333333144, -6.668395609140180369, 3.849999999999994760 ) ) ;
#23133 = CARTESIAN_POINT ( 'NONE',  ( 3.749999999999940492, 2.500000000000000000, 2.857883832488649301 ) ) ;
#23134 = CARTESIAN_POINT ( 'NONE',  ( -0.8500000000000382805, 2.500000000000000000, -7.288010851410854585 ) ) ;
#23135 = CARTESIAN_POINT ( 'NONE',  ( 12.49999999999990052, 12.50000000000000000, 0.7579135962115869374 ) ) ;
#23136 = LINE ( 'NONE', #126500, #20356 ) ;
#23137 = EDGE_LOOP ( 'NONE', ( #125394, #108303, #81718, #61051 ) ) ;
#23139 = EDGE_CURVE ( 'NONE', #90522, #99720, #122748, .T. ) ;
#23138 = AXIS2_PLACEMENT_3D ( 'NONE', #122173, #59401, #90101 ) ;
#23140 = DIRECTION ( 'NONE',  ( 0.000000000000000000, 1.000000000000000000, 0.000000000000000000 ) ) ;
#23141 = CARTESIAN_POINT ( 'NONE',  ( -11.64999999999999858, 2.500000000000000000, -1.472243186433546125 ) ) ;
#23142 = DIRECTION ( 'NONE',  ( 0.000000000000000000, -0.000000000000000000, 1.000000000000000000 ) ) ;
#23143 = EDGE_LOOP ( 'NONE', ( #32782, #35104 ) ) ;
#23144 = DIRECTION ( 'NONE',  ( -4.274815082592931898E-19, -0.9999939076577903929, -0.003490651415223739937 ) ) ;
#23145 = CIRCLE ( 'NONE', #37821, 0.06509327318403743123 ) ;
#23146 = VECTOR ( 'NONE', #62623, 1000.000000000000000 ) ;
#23147 = ORIENTED_EDGE ( 'NONE', *, *, #16123, .T. ) ;
#23148 = ORIENTED_EDGE ( 'NONE', *, *, #23886, .T. ) ;
#23149 = DIRECTION ( 'NONE',  ( 0.000000000000000000, 0.000000000000000000, -1.000000000000000000 ) ) ;
#23150 = EDGE_LOOP ( 'NONE', ( #26321, #107768 ) ) ;
#23151 = CARTESIAN_POINT ( 'NONE',  ( 21.15177371151418839, -2.593223176056361545, -4.151029080743455779 ) ) ;
#23152 = CARTESIAN_POINT ( 'NONE',  ( 9.799999999999915445, 12.50000000000000000, -4.611443907251939756 ) ) ;
#23153 = CARTESIAN_POINT ( 'NONE',  ( 13.74999999999989519, 2.500000000000000000, -2.857883832488653741 ) ) ;
#23154 = ORIENTED_EDGE ( 'NONE', *, *, #53439, .T. ) ;
#23155 = DIRECTION ( 'NONE',  ( 0.000000000000000000, 0.000000000000000000, 1.000000000000000000 ) ) ;
#23156 = CARTESIAN_POINT ( 'NONE',  ( 6.449999999999930012, 2.500000000000000000, 1.818653347947321475 ) ) ;
#23157 = CIRCLE ( 'NONE', #90051, 0.09999999999999982514 ) ;
#23158 = ORIENTED_EDGE ( 'NONE', *, *, #71138, .F. ) ;
#23160 = VERTEX_POINT ( 'NONE', #1671 ) ;
#23159 = EDGE_CURVE ( 'NONE', #251, #51891, #13435, .T. ) ;
#23161 = ORIENTED_EDGE ( 'NONE', *, *, #96226, .F. ) ;
#23162 = CARTESIAN_POINT ( 'NONE',  ( 0.3999999999999628852, 12.50000000000000000, 0.6928203230275518099 ) ) ;
#23163 = CARTESIAN_POINT ( 'NONE',  ( 14.79999999999989235, 2.500000000000000000, 0.4464101615137735513 ) ) ;
#23164 = DIRECTION ( 'NONE',  ( 0.000000000000000000, 0.000000000000000000, 1.000000000000000000 ) ) ;
#23165 = VERTEX_POINT ( 'NONE', #63185 ) ;
#23166 = CARTESIAN_POINT ( 'NONE',  ( -13.29999999999999005, 12.50000000000000000, 0.06509327318403926310 ) ) ;
#23167 = DIRECTION ( 'NONE',  ( 0.000000000000000000, 0.000000000000000000, -1.000000000000000000 ) ) ;
#23168 = EDGE_LOOP ( 'NONE', ( #95211, #5511, #51101, #79071 ) ) ;
#23169 = EDGE_CURVE ( 'NONE', #38948, #32144, #101824, .T. ) ;
#23170 = DIRECTION ( 'NONE',  ( 0.000000000000000000, -0.000000000000000000, 1.000000000000000000 ) ) ;
#23171 = CARTESIAN_POINT ( 'NONE',  ( 6.049999999999934097, 2.500000000000000000, -2.511473670974877948 ) ) ;
#23173 = CARTESIAN_POINT ( 'NONE',  ( 5.399999999999932854, 2.500000000000000000, 3.537306695894645081 ) ) ;
#23172 = CIRCLE ( 'NONE', #79622, 0.1000000000000002554 ) ;
#23174 = DIRECTION ( 'NONE',  ( 0.000000000000000000, 0.000000000000000000, 1.000000000000000000 ) ) ;
#23175 = CARTESIAN_POINT ( 'NONE',  ( 10.39999999999991154, 2.500000000000000000, 5.122947341949749323 ) ) ;
#23176 = AXIS2_PLACEMENT_3D ( 'NONE', #25676, #25041, #26337 ) ;
#23177 = AXIS2_PLACEMENT_3D ( 'NONE', #122104, #120802, #32458 ) ;
#23178 = DIRECTION ( 'NONE',  ( 0.000000000000000000, 0.000000000000000000, -1.000000000000000000 ) ) ;
#23179 = CARTESIAN_POINT ( 'NONE',  ( 0.5999999999999555689, 2.500000000000000000, 4.776537180435972196 ) ) ;
#23180 = AXIS2_PLACEMENT_3D ( 'NONE', #37487, #65632, #116022 ) ;
#23181 = ORIENTED_EDGE ( 'NONE', *, *, #10603, .T. ) ;
#23182 = EDGE_LOOP ( 'NONE', ( #64573, #106870, #82671, #84405 ) ) ;
#23183 = VERTEX_POINT ( 'NONE', #3619 ) ;
#23184 = ORIENTED_EDGE ( 'NONE', *, *, #66351, .T. ) ;
#23185 = CARTESIAN_POINT ( 'NONE',  ( -12.04999999999999538, 2.500000000000000000, 6.495190528383297135 ) ) ;
#23186 = FACE_OUTER_BOUND ( 'NONE', #70334, .T. ) ;
#23187 = CONICAL_SURFACE ( 'NONE', #127751, 0.1000000000000002554, 0.003490658503988666988 ) ;
#23188 = CARTESIAN_POINT ( 'NONE',  ( -12.09999999999999609, 2.500000000000000000, -0.7928203230275502333 ) ) ;
#23189 = EDGE_LOOP ( 'NONE', ( #108998, #125554 ) ) ;
#23190 = FACE_BOUND ( 'NONE', #73569, .T. ) ;
#23191 = FACE_OUTER_BOUND ( 'NONE', #127704, .T. ) ;
#23192 = CARTESIAN_POINT ( 'NONE',  ( -11.64999999999999680, 2.500000000000000000, 1.572243186433545548 ) ) ;
#23193 = DIRECTION ( 'NONE',  ( -0.000000000000000000, 1.000000000000000000, -0.000000000000000000 ) ) ;
#23194 = LINE ( 'NONE', #50729, #120221 ) ;
#23195 = CARTESIAN_POINT ( 'NONE',  ( 2.099999999999949463, 2.500000000000000000, -3.737306695894649700 ) ) ;
#23196 = CARTESIAN_POINT ( 'NONE',  ( 7.299999999999926104, 2.500000000000000000, -0.4464101615137782142 ) ) ;
#23197 = CARTESIAN_POINT ( 'NONE',  ( 6.249999999999932498, 12.50000000000000000, -2.857883832488653741 ) ) ;
#23198 = DIRECTION ( 'NONE',  ( 0.000000000000000000, 1.000000000000000000, 0.000000000000000000 ) ) ;
#23199 = CARTESIAN_POINT ( 'NONE',  ( -11.89999999999999680, 2.500000000000000000, 0.4464101615137776591 ) ) ;
#23200 = VERTEX_POINT ( 'NONE', #93290 ) ;
#23201 = EDGE_CURVE ( 'NONE', #49883, #34238, #30193, .T. ) ;
#23202 = CIRCLE ( 'NONE', #35736, 0.09999999999999982514 ) ;
#23203 = ORIENTED_EDGE ( 'NONE', *, *, #114857, .F. ) ;
#23204 = EDGE_LOOP ( 'NONE', ( #83516, #95039, #70400, #15803 ) ) ;
#23205 = ORIENTED_EDGE ( 'NONE', *, *, #22113, .F. ) ;
#23206 = ORIENTED_EDGE ( 'NONE', *, *, #113177, .T. ) ;
#23207 = ORIENTED_EDGE ( 'NONE', *, *, #66433, .F. ) ;
#23208 = CARTESIAN_POINT ( 'NONE',  ( 9.399999999999915090, 12.50000000000000000, 3.983716857408420964 ) ) ;
#23209 = ORIENTED_EDGE ( 'NONE', *, *, #9792, .F. ) ;
#23210 = EDGE_LOOP ( 'NONE', ( #52948, #5984 ) ) ;
#23211 = AXIS2_PLACEMENT_3D ( 'NONE', #43259, #125647, #73330 ) ;
#23212 = EDGE_CURVE ( 'NONE', #33523, #91737, #103344, .T. ) ;
#23213 = CIRCLE ( 'NONE', #27406, 0.1000000000000000472 ) ;
#23214 = DIRECTION ( 'NONE',  ( -0.000000000000000000, 1.000000000000000000, -0.000000000000000000 ) ) ;
#23215 = LINE ( 'NONE', #44153, #85513 ) ;
#23216 = DIRECTION ( 'NONE',  ( -0.000000000000000000, -1.000000000000000000, -0.000000000000000000 ) ) ;
#23217 = ADVANCED_FACE ( 'NONE', ( #113576 ), #23915, .T. ) ;
#23218 = EDGE_CURVE ( 'NONE', #71153, #79916, #76144, .T. ) ;
#23219 = ORIENTED_EDGE ( 'NONE', *, *, #102902, .T. ) ;
#23220 = DIRECTION ( 'NONE',  ( 0.000000000000000000, 1.000000000000000000, 0.000000000000000000 ) ) ;
#23221 = VECTOR ( 'NONE', #116509, 1000.000000000000000 ) ;
#23222 = AXIS2_PLACEMENT_3D ( 'NONE', #15839, #45969, #85859 ) ;
#23223 = VERTEX_POINT ( 'NONE', #41639 ) ;
#23224 = ORIENTED_EDGE ( 'NONE', *, *, #1260, .T. ) ;
#23225 = PLANE ( 'NONE',  #59363 ) ;
#23226 = EDGE_CURVE ( 'NONE', #23494, #87229, #120062, .T. ) ;
#23227 = DIRECTION ( 'NONE',  ( 0.000000000000000000, 0.000000000000000000, 1.000000000000000000 ) ) ;
#23228 = EDGE_CURVE ( 'NONE', #114181, #69451, #63723, .T. ) ;
#23229 = EDGE_LOOP ( 'NONE', ( #64461, #111297 ) ) ;
#23230 = ORIENTED_EDGE ( 'NONE', *, *, #63892, .F. ) ;
#23231 = AXIS2_PLACEMENT_3D ( 'NONE', #97994, #99943, #50209 ) ;
#23232 = CARTESIAN_POINT ( 'NONE',  ( -2.499999999999996447, 12.50000000000000000, 4.395220292106234439 ) ) ;
#23233 = VECTOR ( 'NONE', #118147, 1000.000000000000000 ) ;
#23234 = DIRECTION ( 'NONE',  ( 0.000000000000000000, 0.000000000000000000, 1.000000000000000000 ) ) ;
#23235 = CARTESIAN_POINT ( 'NONE',  ( 9.149999999999916866, 2.500000000000000000, 7.288010851410849256 ) ) ;
#23236 = DIRECTION ( 'NONE',  ( -0.000000000000000000, -1.000000000000000000, -0.000000000000000000 ) ) ;
#23237 = DIRECTION ( 'NONE',  ( -4.274815082592931898E-19, -0.9999939076577903929, -0.003490651415223739937 ) ) ;
#23238 = CIRCLE ( 'NONE', #98625, 0.06509327318403745899 ) ;
#23239 = ORIENTED_EDGE ( 'NONE', *, *, #30549, .F. ) ;
#23240 = CARTESIAN_POINT ( 'NONE',  ( 3.677302434130775843, -2.499999999999999556, 9.000000000000007105 ) ) ;
#23241 = VERTEX_POINT ( 'NONE', #76875 ) ;
#23242 = CARTESIAN_POINT ( 'NONE',  ( 1.249999999999988454, 12.50000000000000000, -2.230156782645139391 ) ) ;
#23243 = VERTEX_POINT ( 'NONE', #15998 ) ;
#23244 = CARTESIAN_POINT ( 'NONE',  ( 8.349999999999923261, 2.500000000000000000, 2.957883832488649389 ) ) ;
#23245 = CIRCLE ( 'NONE', #96399, 0.06509327318403745899 ) ;
#23246 = CARTESIAN_POINT ( 'NONE',  ( -8.150000000000012790, 12.50000000000000000, 1.818653347947321475 ) ) ;
#23247 = LINE ( 'NONE', #73636, #21561 ) ;
#23248 = CARTESIAN_POINT ( 'NONE',  ( -10.45000000000000107, 12.50000000000000000, 6.495190528383297135 ) ) ;
#23249 = ORIENTED_EDGE ( 'NONE', *, *, #21896, .F. ) ;
#23250 = DIRECTION ( 'NONE',  ( -0.000000000000000000, 1.000000000000000000, -0.000000000000000000 ) ) ;
#23251 = CARTESIAN_POINT ( 'NONE',  ( -3.749999999999994671, 2.500000000000000000, -6.395190528383301931 ) ) ;
#23252 = ORIENTED_EDGE ( 'NONE', *, *, #13615, .F. ) ;
#23253 = VERTEX_POINT ( 'NONE', #114221 ) ;
#23254 = ORIENTED_EDGE ( 'NONE', *, *, #63387, .F. ) ;
#23255 = CARTESIAN_POINT ( 'NONE',  ( -7.050000000000016698, 12.50000000000000000, -6.495190528383302464 ) ) ;
#23256 = CARTESIAN_POINT ( 'NONE',  ( 2.949999999999946887, 12.50000000000000000, -2.099970236277064473 ) ) ;
#23257 = CARTESIAN_POINT ( 'NONE',  ( 185.9843750003414016, -8.734944146203032389, -1.604583208406768146E-15 ) ) ;
#23258 = DIRECTION ( 'NONE',  ( -0.000000000000000000, -1.000000000000000000, -0.000000000000000000 ) ) ;
#23260 = EDGE_CURVE ( 'NONE', #16038, #39771, #92971, .T. ) ;
#23259 = DIRECTION ( 'NONE',  ( 0.000000000000000000, -0.000000000000000000, 1.000000000000000000 ) ) ;
#23261 = DIRECTION ( 'NONE',  ( 0.000000000000000000, 0.000000000000000000, 1.000000000000000000 ) ) ;
#23262 = DIRECTION ( 'NONE',  ( -0.000000000000000000, -1.000000000000000000, -0.000000000000000000 ) ) ;
#23264 = ADVANCED_FACE ( 'NONE', ( #105694 ), #76245, .T. ) ;
#23263 = AXIS2_PLACEMENT_3D ( 'NONE', #128896, #50311, #18265 ) ;
#23265 = AXIS2_PLACEMENT_3D ( 'NONE', #111302, #80591, #93467 ) ;
#23266 = EDGE_CURVE ( 'NONE', #21207, #49328, #51206, .T. ) ;
#23267 = CIRCLE ( 'NONE', #27461, 0.06509327318403745899 ) ;
#23268 = ADVANCED_FACE ( 'NONE', ( #56568 ), #116781, .T. ) ;
#23269 = ADVANCED_FACE ( 'NONE', ( #125326 ), #86699, .T. ) ;
#23270 = ORIENTED_EDGE ( 'NONE', *, *, #45543, .F. ) ;
#23271 = DIRECTION ( 'NONE',  ( 0.000000000000000000, 1.000000000000000000, 0.000000000000000000 ) ) ;
#23272 = CONICAL_SURFACE ( 'NONE', #110995, 0.1000000000000002554, 0.003490658503988666988 ) ;
#23273 = AXIS2_PLACEMENT_3D ( 'NONE', #78948, #88751, #27894 ) ;
#23274 = ORIENTED_EDGE ( 'NONE', *, *, #126373, .T. ) ;
#23275 = ADVANCED_FACE ( 'NONE', ( #96488 ), #116141, .T. ) ;
#23276 = DIRECTION ( 'NONE',  ( 0.000000000000000000, 1.000000000000000000, 0.000000000000000000 ) ) ;
#23277 = AXIS2_PLACEMENT_3D ( 'NONE', #37585, #8102, #88606 ) ;
#23278 = CARTESIAN_POINT ( 'NONE',  ( 3.749999999999978684, 12.50000000000000000, -6.495190528383302464 ) ) ;
#23279 = CARTESIAN_POINT ( 'NONE',  ( 15.59999999999988951, 12.50000000000000000, 0.3464101615137735735 ) ) ;
#23280 = CARTESIAN_POINT ( 'NONE',  ( -12.04999999999999538, 2.500000000000000000, 6.395190528383296602 ) ) ;
#23281 = ORIENTED_EDGE ( 'NONE', *, *, #57066, .F. ) ;
#23282 = ADVANCED_FACE ( 'NONE', ( #6178 ), #85399, .T. ) ;
#23283 = DIRECTION ( 'NONE',  ( 0.000000000000000000, 0.000000000000000000, -1.000000000000000000 ) ) ;
#23284 = EDGE_CURVE ( 'NONE', #22957, #52516, #75571, .T. ) ;
#23285 = DIRECTION ( 'NONE',  ( 0.000000000000000000, 0.000000000000000000, 1.000000000000000000 ) ) ;
#23287 = ORIENTED_EDGE ( 'NONE', *, *, #97921, .T. ) ;
#23286 = CARTESIAN_POINT ( 'NONE',  ( -13.09999999999999076, 2.500000000000000000, 4.676537180435972552 ) ) ;
#23288 = EDGE_LOOP ( 'NONE', ( #25190, #124669 ) ) ;
#23289 = CARTESIAN_POINT ( 'NONE',  ( -11.05000000000000071, 12.50000000000000000, -6.841600689897075149 ) ) ;
#23290 = ORIENTED_EDGE ( 'NONE', *, *, #27220, .F. ) ;
#23291 = ORIENTED_EDGE ( 'NONE', *, *, #25058, .T. ) ;
#23292 = CARTESIAN_POINT ( 'NONE',  ( 4.149999999999939959, 2.500000000000000000, -6.595190528383302109 ) ) ;
#23293 = EDGE_LOOP ( 'NONE', ( #89900, #105828 ) ) ;
#23294 = FACE_OUTER_BOUND ( 'NONE', #91185, .T. ) ;
#23295 = LINE ( 'NONE', #110392, #33797 ) ;
#23296 = DIRECTION ( 'NONE',  ( -0.000000000000000000, 1.000000000000000000, -0.000000000000000000 ) ) ;
#23297 = AXIS2_PLACEMENT_3D ( 'NONE', #107804, #57422, #58073 ) ;
#23298 = ORIENTED_EDGE ( 'NONE', *, *, #47184, .F. ) ;
#23299 = CIRCLE ( 'NONE', #67189, 0.06509327318403741736 ) ;
#23300 = CARTESIAN_POINT ( 'NONE',  ( -12.69999999999999396, 2.500000000000000000, -3.983716857408423628 ) ) ;
#23302 = ORIENTED_EDGE ( 'NONE', *, *, #62126, .F. ) ;
#23301 = CARTESIAN_POINT ( 'NONE',  ( 187.3333333333333144, 6.668395609140177704, -3.849999999999998312 ) ) ;
#23303 = DIRECTION ( 'NONE',  ( 0.000000000000000000, 0.000000000000000000, -1.000000000000000000 ) ) ;
#23304 = CARTESIAN_POINT ( 'NONE',  ( 13.09999999999990195, 12.50000000000000000, -4.676537180435978769 ) ) ;
#23305 = AXIS2_PLACEMENT_3D ( 'NONE', #100110, #78550, #117781 ) ;
#23306 = VERTEX_POINT ( 'NONE', #4887 ) ;
#23307 = CIRCLE ( 'NONE', #58835, 0.1000000000000002554 ) ;
#23308 = ORIENTED_EDGE ( 'NONE', *, *, #16745, .T. ) ;
#23309 = ORIENTED_EDGE ( 'NONE', *, *, #117179, .F. ) ;
#23310 = VERTEX_POINT ( 'NONE', #84761 ) ;
#23311 = CARTESIAN_POINT ( 'NONE',  ( 9.599999999999917932, 12.50000000000000000, 0.6928203230275494784 ) ) ;
#23312 = DIRECTION ( 'NONE',  ( -0.000000000000000000, 1.000000000000000000, -0.000000000000000000 ) ) ;
#23313 = FACE_OUTER_BOUND ( 'NONE', #97924, .T. ) ;
#23314 = FACE_BOUND ( 'NONE', #99131, .T. ) ;
#23315 = ORIENTED_EDGE ( 'NONE', *, *, #39993, .T. ) ;
#23316 = CARTESIAN_POINT ( 'NONE',  ( 185.6145833340161175, 6.668395609140177704, -3.849999999999998312 ) ) ;
#23317 = DIRECTION ( 'NONE',  ( -0.000000000000000000, -1.000000000000000000, -0.000000000000000000 ) ) ;
#23318 = DIRECTION ( 'NONE',  ( -0.000000000000000000, -1.000000000000000000, -0.000000000000000000 ) ) ;
#23319 = AXIS2_PLACEMENT_3D ( 'NONE', #95279, #84150, #4937 ) ;
#23320 = CIRCLE ( 'NONE', #121618, 0.06509327318403745899 ) ;
#23321 = ADVANCED_FACE ( 'NONE', ( #115480 ), #126415, .T. ) ;
#23322 = AXIS2_PLACEMENT_3D ( 'NONE', #23286, #33756, #2341 ) ;
#23323 = DIRECTION ( 'NONE',  ( -0.000000000000000000, 1.000000000000000000, -0.000000000000000000 ) ) ;
#23324 = CARTESIAN_POINT ( 'NONE',  ( 1.449999999999951328, 2.500000000000000000, -1.918653347947326004 ) ) ;
#23325 = DIRECTION ( 'NONE',  ( 0.000000000000000000, 0.000000000000000000, 1.000000000000000000 ) ) ;
#23326 = FACE_OUTER_BOUND ( 'NONE', #112588, .T. ) ;
#23327 = EDGE_LOOP ( 'NONE', ( #83420, #115432 ) ) ;
#23328 = CONICAL_SURFACE ( 'NONE', #56765, 0.1000000000000002554, 0.003490658503988666988 ) ;
#23329 = EDGE_LOOP ( 'NONE', ( #95494, #74256, #109179, #105615 ) ) ;
#23330 = ORIENTED_EDGE ( 'NONE', *, *, #124898, .F. ) ;
#23331 = ORIENTED_EDGE ( 'NONE', *, *, #58709, .F. ) ;
#23332 = ORIENTED_EDGE ( 'NONE', *, *, #100635, .T. ) ;
#23333 = CARTESIAN_POINT ( 'NONE',  ( 13.74999999999993427, 2.500000000000000000, 2.265063509461097357 ) ) ;
#23334 = DIRECTION ( 'NONE',  ( 0.000000000000000000, 0.000000000000000000, 1.000000000000000000 ) ) ;
#23335 = ORIENTED_EDGE ( 'NONE', *, *, #53121, .T. ) ;
#23336 = FACE_BOUND ( 'NONE', #66947, .T. ) ;
#23337 = DIRECTION ( 'NONE',  ( 0.000000000000000000, 1.000000000000000000, 0.000000000000000000 ) ) ;
#23338 = ORIENTED_EDGE ( 'NONE', *, *, #108181, .F. ) ;
#23339 = DIRECTION ( 'NONE',  ( 0.000000000000000000, 0.000000000000000000, -1.000000000000000000 ) ) ;
#23340 = DIRECTION ( 'NONE',  ( 0.000000000000000000, 1.000000000000000000, 0.000000000000000000 ) ) ;
#23341 = DIRECTION ( 'NONE',  ( 0.000000000000000000, 0.000000000000000000, -1.000000000000000000 ) ) ;
#23342 = ORIENTED_EDGE ( 'NONE', *, *, #46304, .F. ) ;
#23343 = CARTESIAN_POINT ( 'NONE',  ( 10.39999999999991509, 2.500000000000000000, 0.5928203230275495006 ) ) ;
#23344 = VERTEX_POINT ( 'NONE', #93937 ) ;
#23345 = ORIENTED_EDGE ( 'NONE', *, *, #2690, .F. ) ;
#23346 = AXIS2_PLACEMENT_3D ( 'NONE', #18964, #28160, #128962 ) ;
#23347 = EDGE_LOOP ( 'NONE', ( #15918, #42975, #86221, #120946 ) ) ;
#23348 = VECTOR ( 'NONE', #46957, 1000.000000000000000 ) ;
#23349 = LINE ( 'NONE', #35771, #35954 ) ;
#23350 = CIRCLE ( 'NONE', #21306, 0.09999999999999982514 ) ;
#23351 = CARTESIAN_POINT ( 'NONE',  ( -9.600000000000006750, 2.500000000000000000, 4.922947341949748257 ) ) ;
#23352 = CARTESIAN_POINT ( 'NONE',  ( 127.5000000000000000, 2.000000000000000000, 5.000000000000001776 ) ) ;
#23353 = VERTEX_POINT ( 'NONE', #74939 ) ;
#23354 = DIRECTION ( 'NONE',  ( -0.000000000000000000, 1.000000000000000000, -0.000000000000000000 ) ) ;
#23355 = EDGE_CURVE ( 'NONE', #15344, #60734, #4242, .T. ) ;
#23356 = DIRECTION ( 'NONE',  ( -0.000000000000000000, -1.000000000000000000, -0.000000000000000000 ) ) ;
#23357 = AXIS2_PLACEMENT_3D ( 'NONE', #79189, #60197, #99471 ) ;
#23358 = CIRCLE ( 'NONE', #12885, 0.1000000000000002554 ) ;
#23359 = DIRECTION ( 'NONE',  ( 0.000000000000000000, 0.000000000000000000, 1.000000000000000000 ) ) ;
#23360 = CARTESIAN_POINT ( 'NONE',  ( 187.1979166673494603, 6.668395609140176816, 3.850000000000000977 ) ) ;
#23361 = ORIENTED_EDGE ( 'NONE', *, *, #19073, .T. ) ;
#23362 = CONICAL_SURFACE ( 'NONE', #100726, 0.1000000000000000472, 0.003490658503988666988 ) ;
#23363 = AXIS2_PLACEMENT_3D ( 'NONE', #53258, #93188, #3510 ) ;
#23364 = ADVANCED_FACE ( 'NONE', ( #86021 ), #55935, .T. ) ;
#23365 = DIRECTION ( 'NONE',  ( 0.000000000000000000, 0.000000000000000000, 1.000000000000000000 ) ) ;
#23366 = EDGE_CURVE ( 'NONE', #70798, #126487, #24006, .T. ) ;
#23367 = EDGE_LOOP ( 'NONE', ( #97280, #15394 ) ) ;
#23368 = PLANE ( 'NONE',  #72243 ) ;
#23369 = AXIS2_PLACEMENT_3D ( 'NONE', #46207, #45578, #5621 ) ;
#23370 = ORIENTED_EDGE ( 'NONE', *, *, #70830, .F. ) ;
#23371 = ORIENTED_EDGE ( 'NONE', *, *, #89317, .T. ) ;
#23372 = DIRECTION ( 'NONE',  ( 0.000000000000000000, -0.9999939076577903929, 0.003490651415223739937 ) ) ;
#23373 = CARTESIAN_POINT ( 'NONE',  ( -7.100000000000017408, 12.50000000000000000, -5.022947341949754119 ) ) ;
#23374 = ADVANCED_FACE ( 'NONE', ( #66398 ), #99231, .T. ) ;
#23375 = EDGE_CURVE ( 'NONE', #55123, #89861, #6806, .T. ) ;
#23376 = FACE_OUTER_BOUND ( 'NONE', #126189, .T. ) ;
#23377 = EDGE_CURVE ( 'NONE', #38438, #48905, #32356, .T. ) ;
#23378 = CARTESIAN_POINT ( 'NONE',  ( 1.649999999999951505, 12.50000000000000000, 2.857883832488649301 ) ) ;
#23379 = EDGE_CURVE ( 'NONE', #128651, #86983, #124360, .T. ) ;
#23380 = CARTESIAN_POINT ( 'NONE',  ( 9.399999999999915090, 2.500000000000000000, -3.983716857408426293 ) ) ;
#23381 = EDGE_LOOP ( 'NONE', ( #57032, #88761 ) ) ;
#23382 = ORIENTED_EDGE ( 'NONE', *, *, #115865, .F. ) ;
#23383 = DIRECTION ( 'NONE',  ( 0.000000000000000000, -0.9999939076577903929, 0.003490651415223739937 ) ) ;
#23384 = DIRECTION ( 'NONE',  ( 0.000000000000000000, 1.000000000000000000, 0.000000000000000000 ) ) ;
#23385 = CARTESIAN_POINT ( 'NONE',  ( -3.350000000000028511, 2.500000000000000000, 2.757883832488649656 ) ) ;
#23386 = ORIENTED_EDGE ( 'NONE', *, *, #101180, .F. ) ;
#23387 = ORIENTED_EDGE ( 'NONE', *, *, #19703, .F. ) ;
#23388 = EDGE_CURVE ( 'NONE', #30668, #76885, #46784, .T. ) ;
#23389 = CARTESIAN_POINT ( 'NONE',  ( -2.950000000000029932, 12.50000000000000000, -2.165063509461101710 ) ) ;
#23391 = EDGE_LOOP ( 'NONE', ( #65181, #54268 ) ) ;
#23390 = VECTOR ( 'NONE', #125504, 1000.000000000000000 ) ;
#23392 = DIRECTION ( 'NONE',  ( -0.000000000000000000, -1.000000000000000000, -0.000000000000000000 ) ) ;
#23393 = DIRECTION ( 'NONE',  ( 0.000000000000000000, 0.000000000000000000, 1.000000000000000000 ) ) ;
#23394 = CIRCLE ( 'NONE', #398, 0.09999999999999982514 ) ;
#23395 = CARTESIAN_POINT ( 'NONE',  ( -6.650000000000014566, 12.50000000000000000, 1.537336459617582918 ) ) ;
#23396 = ORIENTED_EDGE ( 'NONE', *, *, #100691, .F. ) ;
#23397 = CARTESIAN_POINT ( 'NONE',  ( 12.04999999999990479, 2.500000000000000000, -6.595190528383302109 ) ) ;
#23398 = DIRECTION ( 'NONE',  ( 0.000000000000000000, 0.000000000000000000, -1.000000000000000000 ) ) ;
#23399 = DIRECTION ( 'NONE',  ( 0.000000000000000000, 1.000000000000000000, 0.000000000000000000 ) ) ;
#23400 = CARTESIAN_POINT ( 'NONE',  ( 12.29999999999990656, 12.50000000000000000, -4.611443907251939756 ) ) ;
#23401 = DIRECTION ( 'NONE',  ( -0.000000000000000000, 1.000000000000000000, -0.000000000000000000 ) ) ;
#23402 = EDGE_LOOP ( 'NONE', ( #83292, #114661, #61802, #110059 ) ) ;
#23403 = VECTOR ( 'NONE', #109701, 1000.000000000000000 ) ;
#23404 = AXIS2_PLACEMENT_3D ( 'NONE', #46611, #126474, #27598 ) ;
#23405 = DIRECTION ( 'NONE',  ( -4.274815082592931898E-19, -0.9999939076577903929, -0.003490651415223739937 ) ) ;
#23406 = AXIS2_PLACEMENT_3D ( 'NONE', #116655, #103134, #82865 ) ;
#23407 = CARTESIAN_POINT ( 'NONE',  ( 2.899999999999946620, 2.500000000000000000, -5.022947341949754119 ) ) ;
#23408 = ORIENTED_EDGE ( 'NONE', *, *, #65533, .F. ) ;
#23409 =( BOUNDED_SURFACE ( )  B_SPLINE_SURFACE ( 3, 2, ( 
 ( #5069, #120508, #30853 ),
 ( #37762, #67184, #86193 ),
 ( #96659, #58061, #76406 ),
 ( #97328, #108427, #106502 ) ),
 .UNSPECIFIED., .F., .F., .F. ) 
 B_SPLINE_SURFACE_WITH_KNOTS ( ( 4, 4 ),
 ( 3, 3 ),
 ( 0.000000000000000000, 0.002140783231465596091 ),
 ( 0.000000000000000000, 1.000000000000000000 ),
 .UNSPECIFIED. ) 
 GEOMETRIC_REPRESENTATION_ITEM ( )  RATIONAL_B_SPLINE_SURFACE ( (
 ( 1.000000000000000000, 0.7071067811865471286, 1.000000000000000000),
 ( 1.000000000000000000, 0.7083221553718337393, 1.000000000000000000),
 ( 1.000000000000000000, 0.7095583407460066550, 1.000000000000000000),
 ( 1.000000000000000000, 0.7108129114090289136, 1.000000000000000000) ) ) 
 REPRESENTATION_ITEM ( '' )  SURFACE ( )  );
#23410 = ORIENTED_EDGE ( 'NONE', *, *, #30634, .F. ) ;
#23411 = ADVANCED_FACE ( 'NONE', ( #98424 ), #59843, .T. ) ;
#23412 = CARTESIAN_POINT ( 'NONE',  ( 186.5885416670080872, -6.551208109652273848, -3.782341765625003571 ) ) ;
#23413 = CARTESIAN_POINT ( 'NONE',  ( 6.899999999999928413, 12.50000000000000000, 3.983716857408420964 ) ) ;
#23414 = DIRECTION ( 'NONE',  ( 0.000000000000000000, 1.000000000000000000, 0.000000000000000000 ) ) ;
#23415 = CONICAL_SURFACE ( 'NONE', #127974, 0.1000000000000002554, 0.003490658503988666988 ) ;
#23416 = DIRECTION ( 'NONE',  ( 0.000000000000000000, -0.000000000000000000, 1.000000000000000000 ) ) ;
#23417 = CARTESIAN_POINT ( 'NONE',  ( 2.049999999999950084, 12.50000000000000000, 2.099970236277060032 ) ) ;
#23418 = CIRCLE ( 'NONE', #48569, 2.750000000000002665 ) ;
#23419 = CARTESIAN_POINT ( 'NONE',  ( -5.650000000000019895, 2.500000000000000000, 6.841600689897072485 ) ) ;
#23420 = CARTESIAN_POINT ( 'NONE',  ( 1.899999999999951283, 12.50000000000000000, -0.3464101615137782364 ) ) ;
#23421 = DIRECTION ( 'NONE',  ( 0.000000000000000000, 1.000000000000000000, 0.000000000000000000 ) ) ;
#23422 = CIRCLE ( 'NONE', #113306, 0.1000000000000000472 ) ;
#23423 = DIRECTION ( 'NONE',  ( 1.084202172485504434E-16, -0.000000000000000000, 1.000000000000000000 ) ) ;
#23424 = AXIS2_PLACEMENT_3D ( 'NONE', #87760, #47867, #90329 ) ;
#23425 = PLANE ( 'NONE',  #4462 ) ;
#23426 = EDGE_CURVE ( 'NONE', #80635, #96252, #39560, .T. ) ;
#23427 = EDGE_CURVE ( 'NONE', #25583, #114104, #107630, .T. ) ;
#23428 = AXIS2_PLACEMENT_3D ( 'NONE', #100141, #39937, #120421 ) ;
#23429 = ADVANCED_FACE ( 'NONE', ( #109559 ), #65759, .T. ) ;
#23430 = DIRECTION ( 'NONE',  ( 0.000000000000000000, 1.000000000000000000, 0.000000000000000000 ) ) ;
#23431 = VERTEX_POINT ( 'NONE', #68335 ) ;
#23432 = ORIENTED_EDGE ( 'NONE', *, *, #114616, .F. ) ;
#23433 = ADVANCED_FACE ( 'NONE', ( #88624 ), #10066, .T. ) ;
#23434 = AXIS2_PLACEMENT_3D ( 'NONE', #128996, #68099, #9833 ) ;
#23435 = ORIENTED_EDGE ( 'NONE', *, *, #99087, .T. ) ;
#23436 = ADVANCED_FACE ( 'NONE', ( #58538 ), #115944, .T. ) ;
#23437 = ORIENTED_EDGE ( 'NONE', *, *, #64224, .T. ) ;
#23438 = ADVANCED_FACE ( 'NONE', ( #128581 ), #34487, .T. ) ;
#23439 = FACE_OUTER_BOUND ( 'NONE', #98727, .T. ) ;
#23440 = DIRECTION ( 'NONE',  ( 0.000000000000000000, -0.9999939076577903929, 0.003490651415223739937 ) ) ;
#23441 = EDGE_CURVE ( 'NONE', #49455, #98528, #82512, .T. ) ;
#23442 = ORIENTED_EDGE ( 'NONE', *, *, #124974, .T. ) ;
#23443 = EDGE_CURVE ( 'NONE', #72025, #92653, #109694, .T. ) ;
#23444 = DIRECTION ( 'NONE',  ( 0.000000000000000000, 0.000000000000000000, 1.000000000000000000 ) ) ;
#23445 = EDGE_CURVE ( 'NONE', #119499, #75029, #29706, .T. ) ;
#23446 = CARTESIAN_POINT ( 'NONE',  ( -5.000000000000023093, 2.500000000000000000, 0.6928203230275494784 ) ) ;
#23448 = ORIENTED_EDGE ( 'NONE', *, *, #69788, .T. ) ;
#23447 = DIRECTION ( 'NONE',  ( -0.000000000000000000, 1.000000000000000000, -0.000000000000000000 ) ) ;
#23449 = DIRECTION ( 'NONE',  ( 0.000000000000000000, 0.000000000000000000, -1.000000000000000000 ) ) ;
#23450 = ADVANCED_FACE ( 'NONE', ( #106959 ), #7474, .T. ) ;
#23451 = DIRECTION ( 'NONE',  ( -0.000000000000000000, -1.000000000000000000, -0.000000000000000000 ) ) ;
#23452 = VERTEX_POINT ( 'NONE', #127272 ) ;
#23453 = ORIENTED_EDGE ( 'NONE', *, *, #30215, .F. ) ;
#23454 = ORIENTED_EDGE ( 'NONE', *, *, #13602, .T. ) ;
#23455 = CIRCLE ( 'NONE', #128011, 0.09999999999999999167 ) ;
#23456 = EDGE_LOOP ( 'NONE', ( #113429, #28230, #86482, #24508 ) ) ;
#23457 = DIRECTION ( 'NONE',  ( 0.000000000000000000, 0.000000000000000000, 1.000000000000000000 ) ) ;
#23458 = AXIS2_PLACEMENT_3D ( 'NONE', #95116, #27020, #117959 ) ;
#23459 = AXIS2_PLACEMENT_3D ( 'NONE', #109382, #19728, #60313 ) ;
#23460 = CARTESIAN_POINT ( 'NONE',  ( -5.400000000000023448, 12.50000000000000000, -4.330127018922201643 ) ) ;
#23461 = CARTESIAN_POINT ( 'NONE',  ( -4.400000000000025224, 2.500000000000000000, 4.576537180435972019 ) ) ;
#23462 = LINE ( 'NONE', #32675, #62468 ) ;
#23464 = ORIENTED_EDGE ( 'NONE', *, *, #44603, .F. ) ;
#23463 = AXIS2_PLACEMENT_3D ( 'NONE', #105903, #46329, #19442 ) ;
#23465 = AXIS2_PLACEMENT_3D ( 'NONE', #53702, #34736, #22964 ) ;
#23466 = AXIS2_PLACEMENT_3D ( 'NONE', #55824, #5423, #45377 ) ;
#23467 = LINE ( 'NONE', #24767, #127604 ) ;
#23469 = ORIENTED_EDGE ( 'NONE', *, *, #56624, .F. ) ;
#23468 = CIRCLE ( 'NONE', #117531, 0.09999999999999982514 ) ;
#23470 = CARTESIAN_POINT ( 'NONE',  ( 1.849999999999949019, 2.500000000000000000, 6.741600689897071952 ) ) ;
#23471 = CARTESIAN_POINT ( 'NONE',  ( -0.4000000000000331624, 2.500000000000000000, -0.6928203230275519209 ) ) ;
#23472 = AXIS2_PLACEMENT_3D ( 'NONE', #96793, #65406, #86330 ) ;
#23473 = CARTESIAN_POINT ( 'NONE',  ( -10.40000000000000213, 2.500000000000000000, 5.022947341949748790 ) ) ;
#23474 = CARTESIAN_POINT ( 'NONE',  ( 10.19999999999991225, 2.500000000000000000, 3.983716857408420076 ) ) ;
#23475 = AXIS2_PLACEMENT_3D ( 'NONE', #91530, #73177, #81697 ) ;
#23476 = ORIENTED_EDGE ( 'NONE', *, *, #32708, .T. ) ;
#23477 = ORIENTED_EDGE ( 'NONE', *, *, #43555, .T. ) ;
#23478 = ORIENTED_EDGE ( 'NONE', *, *, #34, .T. ) ;
#23479 = CARTESIAN_POINT ( 'NONE',  ( 0.8499999999999553468, 12.50000000000000000, -2.857883832488653741 ) ) ;
#23480 = DIRECTION ( 'NONE',  ( -0.000000000000000000, 1.000000000000000000, -0.000000000000000000 ) ) ;
#23481 = FACE_OUTER_BOUND ( 'NONE', #104236, .T. ) ;
#23482 = FACE_BOUND ( 'NONE', #47507, .T. ) ;
#23483 = PLANE ( 'NONE',  #45097 ) ;
#23484 = CARTESIAN_POINT ( 'NONE',  ( -2.050000000000033129, 2.500000000000000000, 6.395190528383296602 ) ) ;
#23485 = CARTESIAN_POINT ( 'NONE',  ( 13.14999999999989733, 2.500000000000000000, -1.918653347947325782 ) ) ;
#23486 = ADVANCED_FACE ( 'NONE', ( #57227 ), #83817, .T. ) ;
#23487 = DIRECTION ( 'NONE',  ( 0.000000000000000000, 0.000000000000000000, 1.000000000000000000 ) ) ;
#23488 = CARTESIAN_POINT ( 'NONE',  ( 7.099999999999925926, 2.500000000000000000, 0.7928203230275495672 ) ) ;
#23489 = DIRECTION ( 'NONE',  ( 0.000000000000000000, -0.9999939076577903929, 0.003490651415223739937 ) ) ;
#23490 = ORIENTED_EDGE ( 'NONE', *, *, #15292, .F. ) ;
#23491 = AXIS2_PLACEMENT_3D ( 'NONE', #110229, #112167, #24425 ) ;
#23492 = DIRECTION ( 'NONE',  ( -0.000000000000000000, -1.000000000000000000, -0.000000000000000000 ) ) ;
#23493 = ORIENTED_EDGE ( 'NONE', *, *, #123129, .T. ) ;
#23494 = VERTEX_POINT ( 'NONE', #108889 ) ;
#23495 = EDGE_CURVE ( 'NONE', #949, #4124, #81674, .T. ) ;
#23496 = CARTESIAN_POINT ( 'NONE',  ( -6.050000000000020250, 12.50000000000000000, -6.841600689897078702 ) ) ;
#23497 = FACE_BOUND ( 'NONE', #93532, .T. ) ;
#23498 = VECTOR ( 'NONE', #18644, 1000.000000000000000 ) ;
#23499 = DIRECTION ( 'NONE',  ( -0.000000000000000000, 1.000000000000000000, -0.000000000000000000 ) ) ;
#23500 = AXIS2_PLACEMENT_3D ( 'NONE', #62975, #14500, #112085 ) ;
#23501 = CIRCLE ( 'NONE', #107117, 0.06509327318403745899 ) ;
#23502 = ORIENTED_EDGE ( 'NONE', *, *, #119914, .F. ) ;
#23503 = CARTESIAN_POINT ( 'NONE',  ( 32.15727368888380511, 2.842525632570505500, 4.549395963655256558 ) ) ;
#23504 = DIRECTION ( 'NONE',  ( 0.000000000000000000, 0.000000000000000000, -1.000000000000000000 ) ) ;
#23505 = ORIENTED_EDGE ( 'NONE', *, *, #103490, .F. ) ;
#23507 = DIRECTION ( 'NONE',  ( -0.000000000000000000, -1.000000000000000000, -0.000000000000000000 ) ) ;
#23506 = AXIS2_PLACEMENT_3D ( 'NONE', #1270, #41219, #89013 ) ;
#23508 = CARTESIAN_POINT ( 'NONE',  ( 186.6145833340161175, 6.668395609140177704, -3.849999999999998312 ) ) ;
#23509 = CIRCLE ( 'NONE', #128080, 0.1000000000000000472 ) ;
#23510 = CIRCLE ( 'NONE', #36046, 0.09999999999999999167 ) ;
#23511 = AXIS2_PLACEMENT_3D ( 'NONE', #109376, #40008, #50451 ) ;
#23512 = CIRCLE ( 'NONE', #52760, 0.1000000000000002554 ) ;
#23513 = EDGE_LOOP ( 'NONE', ( #50334, #96768, #73208, #68702 ) ) ;
#23514 = CARTESIAN_POINT ( 'NONE',  ( -5.650000000000023448, 12.50000000000000000, -6.841600689897078702 ) ) ;
#23515 = DIRECTION ( 'NONE',  ( 0.000000000000000000, -0.9999939076577903929, 0.003490651415223739937 ) ) ;
#23516 = AXIS2_PLACEMENT_3D ( 'NONE', #107213, #66002, #105932 ) ;
#23517 = VERTEX_POINT ( 'NONE', #78171 ) ;
#23518 = EDGE_CURVE ( 'NONE', #128651, #124598, #59180, .T. ) ;
#23519 = DIRECTION ( 'NONE',  ( -4.274815082592931898E-19, -0.9999939076577903929, -0.003490651415223739937 ) ) ;
#23520 = CIRCLE ( 'NONE', #88259, 0.1000000000000002554 ) ;
#23521 = CARTESIAN_POINT ( 'NONE',  ( 106.0514428414850272, 8.500000000000000000, 1.125000000000000444 ) ) ;
#23522 = CARTESIAN_POINT ( 'NONE',  ( -9.350000000000006750, 12.50000000000000000, -1.883746621131363375 ) ) ;
#23523 = EDGE_LOOP ( 'NONE', ( #52518, #118582 ) ) ;
#23524 = ORIENTED_EDGE ( 'NONE', *, *, #116275, .T. ) ;
#23525 = CARTESIAN_POINT ( 'NONE',  ( -11.64999999999999858, 2.500000000000000000, -1.372243186433546036 ) ) ;
#23526 = EDGE_CURVE ( 'NONE', #26624, #45516, #101019, .T. ) ;
#23527 = ORIENTED_EDGE ( 'NONE', *, *, #32590, .T. ) ;
#23528 = DIRECTION ( 'NONE',  ( 0.000000000000000000, 0.000000000000000000, 1.000000000000000000 ) ) ;
#23529 = FACE_OUTER_BOUND ( 'NONE', #34211, .T. ) ;
#23530 = EDGE_LOOP ( 'NONE', ( #12873, #46701, #60165, #53480 ) ) ;
#23531 = CARTESIAN_POINT ( 'NONE',  ( 2.299999999999946976, 2.500000000000000000, 4.576537180435972019 ) ) ;
#23532 = CARTESIAN_POINT ( 'NONE',  ( 11.24999999999994316, 12.50000000000000000, 2.165063509461097713 ) ) ;
#23533 = DIRECTION ( 'NONE',  ( 0.000000000000000000, 0.000000000000000000, 1.000000000000000000 ) ) ;
#23534 = ADVANCED_FACE ( 'NONE', ( #62400 ), #64940, .T. ) ;
#23535 = EDGE_CURVE ( 'NONE', #7221, #85421, #120667, .T. ) ;
#23536 = DIRECTION ( 'NONE',  ( 0.000000000000000000, 1.000000000000000000, 0.000000000000000000 ) ) ;
#23537 = CIRCLE ( 'NONE', #29811, 0.06509327318403745899 ) ;
#23538 = EDGE_CURVE ( 'NONE', #31627, #41779, #42108, .T. ) ;
#23539 = ADVANCED_FACE ( 'NONE', ( #101676 ), #21165, .T. ) ;
#23540 = EDGE_CURVE ( 'NONE', #109349, #11815, #100545, .T. ) ;
#23541 = FACE_OUTER_BOUND ( 'NONE', #1777, .T. ) ;
#23542 = VERTEX_POINT ( 'NONE', #52561 ) ;
#23543 = ORIENTED_EDGE ( 'NONE', *, *, #39690, .F. ) ;
#23544 = CARTESIAN_POINT ( 'NONE',  ( -6.850000000000013856, 2.500000000000000000, 1.818653347947321475 ) ) ;
#23545 = AXIS2_PLACEMENT_3D ( 'NONE', #91927, #54557, #84022 ) ;
#23546 = CARTESIAN_POINT ( 'NONE',  ( 104.6974693483957282, 6.720082114647700777, -3.767527145165660674 ) ) ;
#23547 = AXIS2_PLACEMENT_3D ( 'NONE', #11783, #67297, #64749 ) ;
#23548 = AXIS2_PLACEMENT_3D ( 'NONE', #50800, #93299, #111654 ) ;
#23550 = ORIENTED_EDGE ( 'NONE', *, *, #103067, .T. ) ;
#23549 = ORIENTED_EDGE ( 'NONE', *, *, #105961, .T. ) ;
#23551 = ORIENTED_EDGE ( 'NONE', *, *, #77075, .T. ) ;
#23552 = ADVANCED_FACE ( 'NONE', ( #112140 ), #25220, .T. ) ;
#23553 = CARTESIAN_POINT ( 'NONE',  ( 1.249999999999988454, 12.50000000000000000, -2.165063509461101710 ) ) ;
#23554 = ADVANCED_FACE ( 'NONE', ( #32952 ), #39924, .T. ) ;
#23555 = DIRECTION ( 'NONE',  ( 1.000000000000000000, 0.000000000000000000, -1.445602896647339656E-16 ) ) ;
#23557 = ADVANCED_FACE ( 'NONE', ( #22488 ), #127641, .T. ) ;
#23556 = VECTOR ( 'NONE', #11171, 1000.000000000000000 ) ;
#23559 = CARTESIAN_POINT ( 'NONE',  ( 10.59999999999991260, 2.500000000000000000, -0.4464101615137783252 ) ) ;
#23558 = CIRCLE ( 'NONE', #96700, 0.06509327318403745899 ) ;
#23560 = AXIS2_PLACEMENT_3D ( 'NONE', #22014, #61932, #3003 ) ;
#23561 = CARTESIAN_POINT ( 'NONE',  ( -0.4000000000000401013, 2.500000000000000000, -3.737306695894649700 ) ) ;
#23562 = DIRECTION ( 'NONE',  ( -0.000000000000000000, 1.000000000000000000, -0.000000000000000000 ) ) ;
#23563 = CARTESIAN_POINT ( 'NONE',  ( 4.799999999999937650, 2.500000000000000000, -0.3464101615137782364 ) ) ;
#23564 = AXIS2_PLACEMENT_3D ( 'NONE', #10027, #40131, #1482 ) ;
#23565 = DIRECTION ( 'NONE',  ( -0.000000000000000000, 1.000000000000000000, -0.000000000000000000 ) ) ;
#23566 = DIRECTION ( 'NONE',  ( 0.000000000000000000, 1.000000000000000000, 0.000000000000000000 ) ) ;
#23567 = AXIS2_PLACEMENT_3D ( 'NONE', #39631, #50092, #59912 ) ;
#23568 = CONICAL_SURFACE ( 'NONE', #7107, 0.1000000000000002554, 0.003490658503988666988 ) ;
#23569 = CARTESIAN_POINT ( 'NONE',  ( 108.0000000000000142, 9.000000000000001776, 0.000000000000000000 ) ) ;
#23570 = VERTEX_POINT ( 'NONE', #100382 ) ;
#23571 = LINE ( 'NONE', #65423, #111232 ) ;
#23572 = VERTEX_POINT ( 'NONE', #60478 ) ;
#23573 = ORIENTED_EDGE ( 'NONE', *, *, #76617, .F. ) ;
#23574 = FACE_OUTER_BOUND ( 'NONE', #76915, .T. ) ;
#23575 = CARTESIAN_POINT ( 'NONE',  ( 187.5000000000000000, 0.000000000000000000, 0.000000000000000000 ) ) ;
#23576 = CARTESIAN_POINT ( 'NONE',  ( -5.850000000000018296, 2.500000000000000000, 2.857883832488649301 ) ) ;
#23577 = CARTESIAN_POINT ( 'NONE',  ( 186.5833333333333144, -6.668395609140180369, 3.849999999999994760 ) ) ;
#23578 = DIRECTION ( 'NONE',  ( 0.000000000000000000, 1.000000000000000000, 0.000000000000000000 ) ) ;
#23579 = CARTESIAN_POINT ( 'NONE',  ( 185.9062500006827747, -8.891194145520236347, -1.633285867636356299E-15 ) ) ;
#23580 = DIRECTION ( 'NONE',  ( 0.000000000000000000, 0.000000000000000000, 1.000000000000000000 ) ) ;
#23581 = EDGE_LOOP ( 'NONE', ( #8847, #481 ) ) ;
#23582 = CARTESIAN_POINT ( 'NONE',  ( -3.300000000000028244, 2.500000000000000000, 4.430127018922196847 ) ) ;
#23584 = AXIS2_PLACEMENT_3D ( 'NONE', #299, #120106, #118161 ) ;
#23583 = LINE ( 'NONE', #25504, #10152 ) ;
#23585 = ORIENTED_EDGE ( 'NONE', *, *, #32175, .T. ) ;
#23586 = CONICAL_SURFACE ( 'NONE', #113470, 0.1000000000000002554, 0.003490658503988666988 ) ;
#23587 = ORIENTED_EDGE ( 'NONE', *, *, #77347, .T. ) ;
#23588 = VERTEX_POINT ( 'NONE', #50630 ) ;
#23589 = EDGE_CURVE ( 'NONE', #114788, #114154, #51301, .T. ) ;
#23590 = VERTEX_POINT ( 'NONE', #112783 ) ;
#23591 = CONICAL_SURFACE ( 'NONE', #38277, 0.09999999999999982514, 0.003490658503988666988 ) ;
#23592 = DIRECTION ( 'NONE',  ( 0.000000000000000000, 0.000000000000000000, 1.000000000000000000 ) ) ;
#23593 = CARTESIAN_POINT ( 'NONE',  ( 7.699999999999925571, 2.500000000000000000, 3.983716857408420076 ) ) ;
#23594 = VECTOR ( 'NONE', #15836, 1000.000000000000000 ) ;
#23595 = ADVANCED_FACE ( 'NONE', ( #43413 ), #119321, .T. ) ;
#23596 = CIRCLE ( 'NONE', #57036, 0.06509327318403745899 ) ;
#23597 = DIRECTION ( 'NONE',  ( -0.000000000000000000, 1.000000000000000000, -0.000000000000000000 ) ) ;
#23598 = CIRCLE ( 'NONE', #44528, 0.1000000000000002554 ) ;
#23599 = DIRECTION ( 'NONE',  ( -0.000000000000000000, 1.000000000000000000, -0.000000000000000000 ) ) ;
#23600 = ADVANCED_FACE ( 'NONE', ( #10680 ), #41485, .T. ) ;
#23601 = DIRECTION ( 'NONE',  ( 0.000000000000000000, -0.9999939076577903929, 0.003490651415223739937 ) ) ;
#23602 = VERTEX_POINT ( 'NONE', #102948 ) ;
#23603 = DIRECTION ( 'NONE',  ( 0.000000000000000000, 1.000000000000000000, 0.000000000000000000 ) ) ;
#23604 = CARTESIAN_POINT ( 'NONE',  ( 8.749999999999957367, 2.500000000000000000, 2.065063509461097624 ) ) ;
#23605 = DIRECTION ( 'NONE',  ( -0.000000000000000000, -1.000000000000000000, -0.000000000000000000 ) ) ;
#23606 = CIRCLE ( 'NONE', #90397, 0.09999999999999999167 ) ;
#23607 = EDGE_CURVE ( 'NONE', #54302, #13172, #48230, .T. ) ;
#23608 = CONICAL_SURFACE ( 'NONE', #90398, 0.1000000000000002554, 0.003490658503988666988 ) ;
#23609 = CARTESIAN_POINT ( 'NONE',  ( 8.749999999999957367, 2.500000000000000000, -6.495190528383302464 ) ) ;
#23610 = ORIENTED_EDGE ( 'NONE', *, *, #69313, .F. ) ;
#23611 = AXIS2_PLACEMENT_3D ( 'NONE', #88704, #101101, #59267 ) ;
#23612 = AXIS2_PLACEMENT_3D ( 'NONE', #107930, #6469, #77818 ) ;
#23613 = CIRCLE ( 'NONE', #38203, 0.09999999999999982514 ) ;
#23614 = ORIENTED_EDGE ( 'NONE', *, *, #67559, .T. ) ;
#23615 = ORIENTED_EDGE ( 'NONE', *, *, #63499, .F. ) ;
#23616 = DIRECTION ( 'NONE',  ( 0.000000000000000000, 0.000000000000000000, 1.000000000000000000 ) ) ;
#23617 = AXIS2_PLACEMENT_3D ( 'NONE', #103850, #101266, #3075 ) ;
#23618 = DIRECTION ( 'NONE',  ( -0.000000000000000000, -1.000000000000000000, -0.000000000000000000 ) ) ;
#23619 = CARTESIAN_POINT ( 'NONE',  ( 13.09999999999989839, 2.500000000000000000, 0.4464101615137735513 ) ) ;
#23620 = AXIS2_PLACEMENT_3D ( 'NONE', #90151, #70530, #100623 ) ;
#23621 = ORIENTED_EDGE ( 'NONE', *, *, #50028, .T. ) ;
#23622 = DIRECTION ( 'NONE',  ( 0.000000000000000000, 0.000000000000000000, 1.000000000000000000 ) ) ;
#23623 = FACE_OUTER_BOUND ( 'NONE', #101793, .T. ) ;
#23624 = CARTESIAN_POINT ( 'NONE',  ( 11.64999999999990798, 2.500000000000000000, 5.802370205355744659 ) ) ;
#23625 = EDGE_CURVE ( 'NONE', #121663, #50143, #96054, .T. ) ;
#23626 = DIRECTION ( 'NONE',  ( 0.000000000000000000, 0.000000000000000000, 1.000000000000000000 ) ) ;
#23627 = DIRECTION ( 'NONE',  ( 0.000000000000000000, 0.000000000000000000, 1.000000000000000000 ) ) ;
#23628 = VERTEX_POINT ( 'NONE', #76077 ) ;
#23629 = CIRCLE ( 'NONE', #128101, 0.09999999999999982514 ) ;
#23630 = ORIENTED_EDGE ( 'NONE', *, *, #114163, .T. ) ;
#23631 = AXIS2_PLACEMENT_3D ( 'NONE', #51146, #91054, #13116 ) ;
#23632 = LINE ( 'NONE', #13147, #43919 ) ;
#23633 = DIRECTION ( 'NONE',  ( 0.000000000000000000, 0.000000000000000000, 1.000000000000000000 ) ) ;
#23634 = CARTESIAN_POINT ( 'NONE',  ( 4.549999999999939426, 2.500000000000000000, -6.395190528383301931 ) ) ;
#23635 = CARTESIAN_POINT ( 'NONE',  ( -5.650000000000019895, 2.500000000000000000, 1.818653347947321475 ) ) ;
#23636 = FACE_OUTER_BOUND ( 'NONE', #71058, .T. ) ;
#23637 = EDGE_LOOP ( 'NONE', ( #94774, #24639 ) ) ;
#23638 = CONICAL_SURFACE ( 'NONE', #36472, 0.1000000000000002554, 0.003490658503988666988 ) ;
#23639 = EDGE_CURVE ( 'NONE', #33187, #50793, #6419, .T. ) ;
#23640 = AXIS2_PLACEMENT_3D ( 'NONE', #74220, #33652, #112860 ) ;
#23641 = VECTOR ( 'NONE', #114493, 1000.000000000000000 ) ;
#23642 = VECTOR ( 'NONE', #46786, 1000.000000000000000 ) ;
#23643 = ORIENTED_EDGE ( 'NONE', *, *, #47093, .F. ) ;
#23644 = FACE_OUTER_BOUND ( 'NONE', #47514, .T. ) ;
#23645 = DIRECTION ( 'NONE',  ( 0.000000000000000000, 0.000000000000000000, 1.000000000000000000 ) ) ;
#23646 = DIRECTION ( 'NONE',  ( 0.000000000000000000, 1.000000000000000000, 0.000000000000000000 ) ) ;
#23647 = CARTESIAN_POINT ( 'NONE',  ( -8.100000000000010303, 12.50000000000000000, 3.983716857408420964 ) ) ;
#23648 = ORIENTED_EDGE ( 'NONE', *, *, #11420, .T. ) ;
#23650 = CARTESIAN_POINT ( 'NONE',  ( -6.050000000000020250, 12.50000000000000000, -2.511473670974877948 ) ) ;
#23649 = AXIS2_PLACEMENT_3D ( 'NONE', #97663, #9288, #68194 ) ;
#23651 = CIRCLE ( 'NONE', #15217, 0.06509327318403745899 ) ;
#23652 = VECTOR ( 'NONE', #101693, 1000.000000000000000 ) ;
#23653 = DIRECTION ( 'NONE',  ( -0.000000000000000000, -1.000000000000000000, -0.000000000000000000 ) ) ;
#23654 = CIRCLE ( 'NONE', #119795, 0.06509327318403745899 ) ;
#23655 = ORIENTED_EDGE ( 'NONE', *, *, #4301, .F. ) ;
#23656 = CIRCLE ( 'NONE', #69723, 0.1000000000000000472 ) ;
#23657 = DIRECTION ( 'NONE',  ( 0.000000000000000000, 0.000000000000000000, 1.000000000000000000 ) ) ;
#23658 = EDGE_CURVE ( 'NONE', #37153, #72458, #94279, .T. ) ;
#23659 = ORIENTED_EDGE ( 'NONE', *, *, #19271, .T. ) ;
#23660 = CONICAL_SURFACE ( 'NONE', #25713, 0.1000000000000002554, 0.003490658503988666988 ) ;
#23661 = CARTESIAN_POINT ( 'NONE',  ( 0.8499999999999553468, 2.500000000000000000, -2.857883832488653741 ) ) ;
#23662 = ORIENTED_EDGE ( 'NONE', *, *, #11996, .F. ) ;
#23663 = CARTESIAN_POINT ( 'NONE',  ( 1.249999999999952038, 2.500000000000000000, 5.802370205355744659 ) ) ;
#23664 = CARTESIAN_POINT ( 'NONE',  ( -5.650000000000019895, 12.50000000000000000, 6.148780366869520009 ) ) ;
#23665 = EDGE_LOOP ( 'NONE', ( #111851, #108256 ) ) ;
#23666 = ORIENTED_EDGE ( 'NONE', *, *, #92992, .T. ) ;
#23667 = CARTESIAN_POINT ( 'NONE',  ( 186.0468750003414300, -8.734944146203032389, -1.604583208406768146E-15 ) ) ;
#23668 = CARTESIAN_POINT ( 'NONE',  ( -13.09999999999999254, 2.500000000000000000, -3.983716857408423628 ) ) ;
#23669 = CONICAL_SURFACE ( 'NONE', #36206, 0.1000000000000000472, 0.003490658503988666988 ) ;
#23670 = CARTESIAN_POINT ( 'NONE',  ( 186.4218750003414016, 0.000000000000000000, 7.564683531250000925 ) ) ;
#23671 = CARTESIAN_POINT ( 'NONE',  ( 185.2343750003414016, 8.734944146203032389, 5.348610694689227483E-16 ) ) ;
#23672 = DIRECTION ( 'NONE',  ( -0.000000000000000000, 1.000000000000000000, -0.000000000000000000 ) ) ;
#23673 = DIRECTION ( 'NONE',  ( 0.000000000000000000, 0.000000000000000000, -1.000000000000000000 ) ) ;
#23674 = DIRECTION ( 'NONE',  ( 0.000000000000000000, 0.000000000000000000, -1.000000000000000000 ) ) ;
#23675 = LINE ( 'NONE', #92408, #42132 ) ;
#23676 = AXIS2_PLACEMENT_3D ( 'NONE', #124889, #75145, #65302 ) ;
#23677 = AXIS2_PLACEMENT_3D ( 'NONE', #46695, #73557, #14628 ) ;
#23678 = ORIENTED_EDGE ( 'NONE', *, *, #78567, .T. ) ;
#23680 = ORIENTED_EDGE ( 'NONE', *, *, #69786, .F. ) ;
#23679 = ADVANCED_FACE ( 'NONE', ( #56421 ), #125572, .T. ) ;
#23681 = DIRECTION ( 'NONE',  ( -0.000000000000000000, 1.000000000000000000, -0.000000000000000000 ) ) ;
#23682 = ORIENTED_EDGE ( 'NONE', *, *, #120243, .F. ) ;
#23683 = DIRECTION ( 'NONE',  ( 0.000000000000000000, 0.000000000000000000, 1.000000000000000000 ) ) ;
#23684 = DIRECTION ( 'NONE',  ( 0.000000000000000000, 1.000000000000000000, 0.000000000000000000 ) ) ;
#23685 = DIRECTION ( 'NONE',  ( -0.000000000000000000, -1.000000000000000000, -0.000000000000000000 ) ) ;
#23687 = ORIENTED_EDGE ( 'NONE', *, *, #3504, .F. ) ;
#23686 = ORIENTED_EDGE ( 'NONE', *, *, #58152, .T. ) ;
#23688 = CARTESIAN_POINT ( 'NONE',  ( 0.000000000000000000, 2.500000000000000000, 0.000000000000000000 ) ) ;
#23689 = ORIENTED_EDGE ( 'NONE', *, *, #10255, .F. ) ;
#23690 = EDGE_CURVE ( 'NONE', #76936, #30682, #63686, .T. ) ;
#23691 = CIRCLE ( 'NONE', #122086, 0.1000000000000002554 ) ;
#23692 = FACE_OUTER_BOUND ( 'NONE', #99651, .T. ) ;
#23693 = CARTESIAN_POINT ( 'NONE',  ( 184.7500000000000000, 9.429780353434619030E-16, -7.700000000000000178 ) ) ;
#23694 = AXIS2_PLACEMENT_3D ( 'NONE', #56088, #86842, #16788 ) ;
#23697 = EDGE_CURVE ( 'NONE', #1010, #104091, #79623, .T. ) ;
#23696 = DIRECTION ( 'NONE',  ( 0.000000000000000000, -0.9999939076577903929, 0.003490651415223739937 ) ) ;
#23695 = AXIS2_PLACEMENT_3D ( 'NONE', #65877, #1950, #122395 ) ;
#23698 = DIRECTION ( 'NONE',  ( -4.274815082592931898E-19, -0.9999939076577903929, -0.003490651415223739937 ) ) ;
#23699 = CARTESIAN_POINT ( 'NONE',  ( 0.8499999999999545697, 2.500000000000000000, -1.572243186433550211 ) ) ;
#23700 = CARTESIAN_POINT ( 'NONE',  ( -0.8500000000000382805, 12.50000000000000000, -7.122917578226816815 ) ) ;
#23701 = CARTESIAN_POINT ( 'NONE',  ( 2.899999999999946620, 2.500000000000000000, -3.637306695894650055 ) ) ;
#23702 = CARTESIAN_POINT ( 'NONE',  ( 9.999999999999952038, 2.500000000000000000, -2.276824562219559311E-15 ) ) ;
#23703 = EDGE_CURVE ( 'NONE', #117167, #12607, #92131, .T. ) ;
#23704 = EDGE_CURVE ( 'NONE', #18200, #55354, #60841, .T. ) ;
#23705 = DIRECTION ( 'NONE',  ( -0.000000000000000000, -1.000000000000000000, -0.000000000000000000 ) ) ;
#23706 = CARTESIAN_POINT ( 'NONE',  ( -1.650000000000034328, 12.50000000000000000, -2.792790559304616504 ) ) ;
#23707 = EDGE_CURVE ( 'NONE', #99701, #103573, #113062, .T. ) ;
#23708 = EDGE_CURVE ( 'NONE', #107893, #23087, #56609, .T. ) ;
#23709 = FACE_OUTER_BOUND ( 'NONE', #112006, .T. ) ;
#23710 = ORIENTED_EDGE ( 'NONE', *, *, #74240, .F. ) ;
#23711 = EDGE_LOOP ( 'NONE', ( #54915, #51897 ) ) ;
#23712 = ORIENTED_EDGE ( 'NONE', *, *, #54768, .T. ) ;
#23713 = FACE_OUTER_BOUND ( 'NONE', #118735, .T. ) ;
#23715 = ORIENTED_EDGE ( 'NONE', *, *, #110048, .F. ) ;
#23714 = VECTOR ( 'NONE', #80154, 1000.000000000000000 ) ;
#23716 = AXIS2_PLACEMENT_3D ( 'NONE', #107900, #98711, #77158 ) ;
#23717 = ADVANCED_FACE ( 'NONE', ( #104868 ), #65603, .T. ) ;
#23718 = CARTESIAN_POINT ( 'NONE',  ( -6.850000000000017408, 2.500000000000000000, -6.048780366869526581 ) ) ;
#23721 = ORIENTED_EDGE ( 'NONE', *, *, #102567, .F. ) ;
#23720 = ORIENTED_EDGE ( 'NONE', *, *, #56536, .T. ) ;
#23719 = EDGE_CURVE ( 'NONE', #25933, #77313, #2238, .T. ) ;
#23722 = EDGE_LOOP ( 'NONE', ( #101682, #99818 ) ) ;
#23723 = CIRCLE ( 'NONE', #55113, 0.06509327318403745899 ) ;
#23724 = EDGE_CURVE ( 'NONE', #93103, #80552, #73351, .T. ) ;
#23725 = CARTESIAN_POINT ( 'NONE',  ( 129.5000000000000000, 1.375000000000000000, 7.634788798650556707 ) ) ;
#23726 = EDGE_CURVE ( 'NONE', #70184, #91613, #15764, .T. ) ;
#23727 = EDGE_CURVE ( 'NONE', #16935, #82756, #67064, .T. ) ;
#23728 = LINE ( 'NONE', #24366, #101206 ) ;
#23729 = DIRECTION ( 'NONE',  ( 0.000000000000000000, 1.000000000000000000, 0.000000000000000000 ) ) ;
#23730 = DIRECTION ( 'NONE',  ( -0.000000000000000000, 1.000000000000000000, -0.000000000000000000 ) ) ;
#23731 = CARTESIAN_POINT ( 'NONE',  ( 12.29999999999990123, 12.50000000000000000, 0.4115034346978109769 ) ) ;
#23732 = CARTESIAN_POINT ( 'NONE',  ( 7.299999999999926104, 2.500000000000000000, -0.2464101615137782308 ) ) ;
#23733 = ORIENTED_EDGE ( 'NONE', *, *, #120506, .T. ) ;
#23734 = ADVANCED_FACE ( 'NONE', ( #44687 ), #106798, .T. ) ;
#23735 = CARTESIAN_POINT ( 'NONE',  ( 12.49999999999990585, 2.500000000000000000, -5.122947341949753763 ) ) ;
#23736 = ORIENTED_EDGE ( 'NONE', *, *, #126407, .F. ) ;
#23737 = ORIENTED_EDGE ( 'NONE', *, *, #116754, .F. ) ;
#23738 = ORIENTED_EDGE ( 'NONE', *, *, #112201, .F. ) ;
#23739 = CARTESIAN_POINT ( 'NONE',  ( -4.350000000000023626, 2.500000000000000000, 2.611473670974873151 ) ) ;
#23740 = AXIS2_PLACEMENT_3D ( 'NONE', #66704, #45158, #86339 ) ;
#23741 = CONICAL_SURFACE ( 'NONE', #44567, 0.1000000000000002554, 0.003490658503988666988 ) ;
#23742 = ORIENTED_EDGE ( 'NONE', *, *, #101030, .T. ) ;
#23743 = VERTEX_POINT ( 'NONE', #124538 ) ;
#23744 = VERTEX_POINT ( 'NONE', #34884 ) ;
#23745 = DIRECTION ( 'NONE',  ( -0.000000000000000000, 1.000000000000000000, -0.000000000000000000 ) ) ;
#23747 = CARTESIAN_POINT ( 'NONE',  ( 3.149999999999946176, 12.50000000000000000, -1.818653347947325916 ) ) ;
#23746 = CIRCLE ( 'NONE', #34115, 0.06509327318403745899 ) ;
#23748 = CIRCLE ( 'NONE', #44673, 0.1000000000000002554 ) ;
#23749 = CARTESIAN_POINT ( 'NONE',  ( 9.999999999999952038, 2.500000000000000000, -2.276824562219559311E-15 ) ) ;
#23751 = DIRECTION ( 'NONE',  ( -0.000000000000000000, -1.000000000000000000, -0.000000000000000000 ) ) ;
#23750 = CIRCLE ( 'NONE', #32167, 0.06509327318403745899 ) ;
#23752 = DIRECTION ( 'NONE',  ( -0.000000000000000000, -1.000000000000000000, -0.000000000000000000 ) ) ;
#23753 = AXIS2_PLACEMENT_3D ( 'NONE', #14195, #46244, #16118 ) ;
#23754 = CIRCLE ( 'NONE', #42540, 0.06509327318403745899 ) ;
#23755 = DIRECTION ( 'NONE',  ( 0.000000000000000000, 0.000000000000000000, 1.000000000000000000 ) ) ;
#23756 = LINE ( 'NONE', #44681, #38805 ) ;
#23758 = ORIENTED_EDGE ( 'NONE', *, *, #91626, .F. ) ;
#23757 = CIRCLE ( 'NONE', #113629, 0.09999999999999982514 ) ;
#23759 = CARTESIAN_POINT ( 'NONE',  ( 11.44999999999990870, 2.500000000000000000, 6.941600689897073018 ) ) ;
#23760 = AXIS2_PLACEMENT_3D ( 'NONE', #8666, #119941, #128494 ) ;
#23761 = ORIENTED_EDGE ( 'NONE', *, *, #120335, .T. ) ;
#23762 = CARTESIAN_POINT ( 'NONE',  ( 7.299999999999926104, 12.50000000000000000, 4.676537180435972552 ) ) ;
#23763 = AXIS2_PLACEMENT_3D ( 'NONE', #116271, #14197, #63965 ) ;
#23764 = ORIENTED_EDGE ( 'NONE', *, *, #12608, .T. ) ;
#23765 = ORIENTED_EDGE ( 'NONE', *, *, #102720, .F. ) ;
#23766 = CARTESIAN_POINT ( 'NONE',  ( -5.850000000000021849, 12.50000000000000000, -7.188010851410854052 ) ) ;
#23767 = LINE ( 'NONE', #71561, #100759 ) ;
#23768 = EDGE_CURVE ( 'NONE', #107010, #3741, #33655, .T. ) ;
#23769 = DIRECTION ( 'NONE',  ( -0.000000000000000000, 1.000000000000000000, -0.000000000000000000 ) ) ;
#23770 = EDGE_CURVE ( 'NONE', #39659, #107424, #10636, .T. ) ;
#23771 = VERTEX_POINT ( 'NONE', #77366 ) ;
#23772 = EDGE_LOOP ( 'NONE', ( #127601, #46441 ) ) ;
#23773 = DIRECTION ( 'NONE',  ( 0.000000000000000000, 0.000000000000000000, 1.000000000000000000 ) ) ;
#23774 = CARTESIAN_POINT ( 'NONE',  ( 10.84999999999991260, 2.500000000000000000, 7.188010851410848723 ) ) ;
#23775 = DIRECTION ( 'NONE',  ( 0.000000000000000000, 0.000000000000000000, 1.000000000000000000 ) ) ;
#23776 = CARTESIAN_POINT ( 'NONE',  ( -6.650000000000019007, 2.500000000000000000, -5.702370205355749455 ) ) ;
#23777 = CONICAL_SURFACE ( 'NONE', #122068, 0.09999999999999982514, 0.003490658503988666988 ) ;
#23778 = EDGE_CURVE ( 'NONE', #129312, #128693, #57733, .T. ) ;
#23779 = CARTESIAN_POINT ( 'NONE',  ( -6.900000000000019007, 2.500000000000000000, -4.676537180435978769 ) ) ;
#23780 = ORIENTED_EDGE ( 'NONE', *, *, #46249, .F. ) ;
#23781 = AXIS2_PLACEMENT_3D ( 'NONE', #31213, #41685, #101874 ) ;
#23782 = EDGE_LOOP ( 'NONE', ( #36675, #103451, #104354, #55718 ) ) ;
#23783 = AXIS2_PLACEMENT_3D ( 'NONE', #8042, #127823, #108816 ) ;
#23784 = CARTESIAN_POINT ( 'NONE',  ( 12.49999999999993960, 2.500000000000000000, -4.330127018922201643 ) ) ;
#23785 = DIRECTION ( 'NONE',  ( -0.000000000000000000, -1.000000000000000000, -0.000000000000000000 ) ) ;
#23786 = CIRCLE ( 'NONE', #7024, 0.06509327318403743123 ) ;
#23787 = CARTESIAN_POINT ( 'NONE',  ( 184.0468750003414300, -8.734944146203032389, -1.604583208406768146E-15 ) ) ;
#23788 = DIRECTION ( 'NONE',  ( 0.000000000000000000, -0.9999939076577903929, 0.003490651415223739937 ) ) ;
#23789 = DIRECTION ( 'NONE',  ( 0.000000000000000000, 0.000000000000000000, 1.000000000000000000 ) ) ;
#23790 = DIRECTION ( 'NONE',  ( -0.000000000000000000, -1.000000000000000000, -0.000000000000000000 ) ) ;
#23791 = CONICAL_SURFACE ( 'NONE', #40532, 0.09999999999999982514, 0.003490658503988666988 ) ;
#23793 = CIRCLE ( 'NONE', #57233, 0.09999999999999982514 ) ;
#23792 = CARTESIAN_POINT ( 'NONE',  ( 1.322875655532295136, -1.500000000000000222, -5.000000000000004441 ) ) ;
#23794 = VERTEX_POINT ( 'NONE', #8593 ) ;
#23795 = CIRCLE ( 'NONE', #42683, 0.06509327318403745899 ) ;
#23796 = CONICAL_SURFACE ( 'NONE', #21735, 0.1000000000000002554, 0.003490658503988666988 ) ;
#23797 = CARTESIAN_POINT ( 'NONE',  ( 7.299999999999924327, 2.500000000000000000, 0.3464101615137735735 ) ) ;
#23798 = CARTESIAN_POINT ( 'NONE',  ( -11.05000000000000071, 12.50000000000000000, -2.511473670974873951 ) ) ;
#23799 = DIRECTION ( 'NONE',  ( 0.000000000000000000, 0.000000000000000000, 1.000000000000000000 ) ) ;
#23800 = EDGE_LOOP ( 'NONE', ( #87413, #106530 ) ) ;
#23801 = DIRECTION ( 'NONE',  ( 0.000000000000000000, 1.000000000000000000, 0.000000000000000000 ) ) ;
#23802 = EDGE_CURVE ( 'NONE', #55739, #36661, #62989, .T. ) ;
#23803 = VERTEX_POINT ( 'NONE', #67514 ) ;
#23804 = CIRCLE ( 'NONE', #57250, 0.09999999999999982514 ) ;
#23805 = CIRCLE ( 'NONE', #90699, 0.1000000000000000472 ) ;
#23806 = AXIS2_PLACEMENT_3D ( 'NONE', #65232, #5663, #45625 ) ;
#23807 = DIRECTION ( 'NONE',  ( -4.274815082592931898E-19, -0.9999939076577903929, -0.003490651415223739937 ) ) ;
#23809 = EDGE_LOOP ( 'NONE', ( #33744, #122302, #85066, #61673 ) ) ;
#23808 = VECTOR ( 'NONE', #44785, 1000.000000000000000 ) ;
#23810 = DIRECTION ( 'NONE',  ( 0.000000000000000000, 0.000000000000000000, 1.000000000000000000 ) ) ;
#23811 = CARTESIAN_POINT ( 'NONE',  ( -3.350000000000028955, 2.500000000000000000, 5.902370205355745192 ) ) ;
#23812 = CARTESIAN_POINT ( 'NONE',  ( 8.949999999999915801, 12.50000000000000000, -1.818653347947326138 ) ) ;
#23813 = CIRCLE ( 'NONE', #115734, 0.1000000000000002554 ) ;
#23814 = ORIENTED_EDGE ( 'NONE', *, *, #50107, .T. ) ;
#23815 = DIRECTION ( 'NONE',  ( -4.274815082592931898E-19, -0.9999939076577903929, -0.003490651415223739937 ) ) ;
#23816 = CARTESIAN_POINT ( 'NONE',  ( 186.5833333333333144, -6.668395609140180369, 3.849999999999994760 ) ) ;
#23817 = ADVANCED_FACE ( 'NONE', ( #78665 ), #127738, .T. ) ;
#23818 = ADVANCED_FACE ( 'NONE', ( #87167 ), #104733, .T. ) ;
#23819 = VERTEX_POINT ( 'NONE', #28263 ) ;
#23820 = ORIENTED_EDGE ( 'NONE', *, *, #42016, .T. ) ;
#23821 = EDGE_LOOP ( 'NONE', ( #62367, #67228 ) ) ;
#23822 = DIRECTION ( 'NONE',  ( 0.000000000000000000, -0.000000000000000000, 1.000000000000000000 ) ) ;
#23823 = PLANE ( 'NONE',  #33360 ) ;
#23825 = CARTESIAN_POINT ( 'NONE',  ( 10.84999999999991260, 2.500000000000000000, -1.572243186433550211 ) ) ;
#23824 = CIRCLE ( 'NONE', #124166, 0.06509327318403741736 ) ;
#23826 = CIRCLE ( 'NONE', #94830, 0.1000000000000002554 ) ;
#23827 = EDGE_CURVE ( 'NONE', #51156, #4055, #2328, .T. ) ;
#23828 = ORIENTED_EDGE ( 'NONE', *, *, #73366, .T. ) ;
#23829 = DIRECTION ( 'NONE',  ( -0.000000000000000000, 1.000000000000000000, -0.000000000000000000 ) ) ;
#23830 = DIRECTION ( 'NONE',  ( -0.000000000000000000, 1.000000000000000000, -0.000000000000000000 ) ) ;
#23831 = ORIENTED_EDGE ( 'NONE', *, *, #59367, .T. ) ;
#23832 = DIRECTION ( 'NONE',  ( 0.000000000000000000, 0.000000000000000000, 1.000000000000000000 ) ) ;
#23834 = CARTESIAN_POINT ( 'NONE',  ( 0.8499999999999545697, 2.500000000000000000, 2.957883832488649389 ) ) ;
#23833 = VECTOR ( 'NONE', #120711, 1000.000000000000000 ) ;
#23835 = AXIS2_PLACEMENT_3D ( 'NONE', #22651, #84777, #44194 ) ;
#23836 = AXIS2_PLACEMENT_3D ( 'NONE', #121986, #12016, #62433 ) ;
#23837 = CIRCLE ( 'NONE', #80076, 0.06509327318403745899 ) ;
#23839 = CONICAL_SURFACE ( 'NONE', #86219, 0.1000000000000002554, 0.003490658503988666988 ) ;
#23838 = DIRECTION ( 'NONE',  ( 0.000000000000000000, 0.000000000000000000, 1.000000000000000000 ) ) ;
#23840 = DIRECTION ( 'NONE',  ( 0.000000000000000000, 0.000000000000000000, 1.000000000000000000 ) ) ;
#23841 = DIRECTION ( 'NONE',  ( 0.000000000000000000, 0.000000000000000000, 1.000000000000000000 ) ) ;
#23842 = DIRECTION ( 'NONE',  ( 0.000000000000000000, 1.000000000000000000, 0.000000000000000000 ) ) ;
#23843 = DIRECTION ( 'NONE',  ( -0.000000000000000000, 1.000000000000000000, -0.000000000000000000 ) ) ;
#23844 = CIRCLE ( 'NONE', #76071, 0.1000000000000002554 ) ;
#23845 = VECTOR ( 'NONE', #114521, 1000.000000000000000 ) ;
#23846 = AXIS2_PLACEMENT_3D ( 'NONE', #43964, #110750, #61008 ) ;
#23847 = EDGE_LOOP ( 'NONE', ( #48447, #20004 ) ) ;
#23848 = ORIENTED_EDGE ( 'NONE', *, *, #36355, .F. ) ;
#23849 = EDGE_LOOP ( 'NONE', ( #6645, #126955, #127097, #19229 ) ) ;
#23850 = ORIENTED_EDGE ( 'NONE', *, *, #19014, .T. ) ;
#23851 = FACE_OUTER_BOUND ( 'NONE', #90131, .T. ) ;
#23852 = CARTESIAN_POINT ( 'NONE',  ( -12.29999999999999716, 2.500000000000000000, 0.2464101615137776757 ) ) ;
#23853 = CIRCLE ( 'NONE', #67751, 0.06509327318403745899 ) ;
#23854 = CARTESIAN_POINT ( 'NONE',  ( 3.099999999999943245, 2.500000000000000000, 3.883716857408420431 ) ) ;
#23855 = ORIENTED_EDGE ( 'NONE', *, *, #22969, .T. ) ;
#23856 = FACE_BOUND ( 'NONE', #47833, .T. ) ;
#23857 = CARTESIAN_POINT ( 'NONE',  ( 2.699999999999944666, 2.500000000000000000, 4.776537180435972196 ) ) ;
#23858 = CARTESIAN_POINT ( 'NONE',  ( 2.899999999999945732, 12.50000000000000000, -0.06509327318403980434 ) ) ;
#23860 = ADVANCED_FACE ( 'NONE', ( #47268 ), #8587, .T. ) ;
#23859 = DIRECTION ( 'NONE',  ( 0.000000000000000000, 0.000000000000000000, 1.000000000000000000 ) ) ;
#23861 = DIRECTION ( 'NONE',  ( 0.000000000000000000, 0.000000000000000000, 1.000000000000000000 ) ) ;
#23862 = DIRECTION ( 'NONE',  ( 0.000000000000000000, 0.000000000000000000, 1.000000000000000000 ) ) ;
#23863 = CIRCLE ( 'NONE', #101219, 0.09999999999999982514 ) ;
#23864 = DIRECTION ( 'NONE',  ( 0.000000000000000000, 1.000000000000000000, 0.000000000000000000 ) ) ;
#23865 = DIRECTION ( 'NONE',  ( -0.000000000000000000, -1.000000000000000000, -0.000000000000000000 ) ) ;
#23866 = DIRECTION ( 'NONE',  ( 0.000000000000000000, 0.000000000000000000, 1.000000000000000000 ) ) ;
#23867 = EDGE_CURVE ( 'NONE', #41297, #32010, #38756, .T. ) ;
#23868 = FACE_OUTER_BOUND ( 'NONE', #86326, .T. ) ;
#23869 = EDGE_CURVE ( 'NONE', #29869, #67997, #52523, .T. ) ;
#23870 = CIRCLE ( 'NONE', #97014, 0.06509327318403745899 ) ;
#23871 = LINE ( 'NONE', #85352, #100410 ) ;
#23872 = ORIENTED_EDGE ( 'NONE', *, *, #116127, .F. ) ;
#23873 = ORIENTED_EDGE ( 'NONE', *, *, #93295, .F. ) ;
#23874 = ORIENTED_EDGE ( 'NONE', *, *, #82182, .T. ) ;
#23875 = ORIENTED_EDGE ( 'NONE', *, *, #25692, .T. ) ;
#23876 = ORIENTED_EDGE ( 'NONE', *, *, #44116, .T. ) ;
#23877 = EDGE_CURVE ( 'NONE', #39515, #6261, #81755, .T. ) ;
#23878 = ORIENTED_EDGE ( 'NONE', *, *, #121367, .F. ) ;
#23880 = EDGE_CURVE ( 'NONE', #56128, #4802, #98936, .T. ) ;
#23879 = DIRECTION ( 'NONE',  ( -0.000000000000000000, -1.000000000000000000, -0.000000000000000000 ) ) ;
#23882 = ORIENTED_EDGE ( 'NONE', *, *, #33497, .T. ) ;
#23881 = EDGE_CURVE ( 'NONE', #100348, #26373, #69229, .T. ) ;
#23883 = ORIENTED_EDGE ( 'NONE', *, *, #23639, .T. ) ;
#23884 = AXIS2_PLACEMENT_3D ( 'NONE', #53143, #80362, #10932 ) ;
#23885 = VECTOR ( 'NONE', #85137, 1000.000000000000000 ) ;
#23886 = EDGE_CURVE ( 'NONE', #79541, #57283, #47912, .T. ) ;
#23887 = CARTESIAN_POINT ( 'NONE',  ( 15.22989033483591470, -1.499999999999968470, 7.180069493258844915 ) ) ;
#23888 = CARTESIAN_POINT ( 'NONE',  ( 175.5000000000000000, 6.123233995736768501E-17, -1.500000000000000000 ) ) ;
#23889 = LINE ( 'NONE', #103734, #96933 ) ;
#23890 = EDGE_LOOP ( 'NONE', ( #113371, #44265 ) ) ;
#23891 = DIRECTION ( 'NONE',  ( -0.000000000000000000, 1.000000000000000000, -0.000000000000000000 ) ) ;
#23892 = EDGE_CURVE ( 'NONE', #19348, #117873, #36805, .T. ) ;
#23893 = ORIENTED_EDGE ( 'NONE', *, *, #45187, .F. ) ;
#23894 = CIRCLE ( 'NONE', #44821, 0.1000000000000002554 ) ;
#23895 = ORIENTED_EDGE ( 'NONE', *, *, #94026, .T. ) ;
#23897 = ORIENTED_EDGE ( 'NONE', *, *, #71898, .T. ) ;
#23896 = CARTESIAN_POINT ( 'NONE',  ( 2.899999999999945732, 2.500000000000000000, -4.430127018922202176 ) ) ;
#23898 = CARTESIAN_POINT ( 'NONE',  ( 184.5833333333333144, -6.668395609140180369, 3.849999999999994760 ) ) ;
#23899 = VERTEX_POINT ( 'NONE', #78002 ) ;
#23900 = DIRECTION ( 'NONE',  ( 0.000000000000000000, 1.000000000000000000, 0.000000000000000000 ) ) ;
#23902 = AXIS2_PLACEMENT_3D ( 'NONE', #102838, #53120, #3366 ) ;
#23901 = DIRECTION ( 'NONE',  ( -0.000000000000000000, 1.000000000000000000, -0.000000000000000000 ) ) ;
#23903 = CARTESIAN_POINT ( 'NONE',  ( -1.900000000000034994, 2.500000000000000000, -0.4464101615137783252 ) ) ;
#23904 = AXIS2_PLACEMENT_3D ( 'NONE', #58441, #39461, #68881 ) ;
#23905 = CARTESIAN_POINT ( 'NONE',  ( 1.649999999999950617, 2.500000000000000000, 2.065063509461097624 ) ) ;
#23906 = LINE ( 'NONE', #116131, #94190 ) ;
#23907 = VECTOR ( 'NONE', #113347, 1000.000000000000000 ) ;
#23908 = ORIENTED_EDGE ( 'NONE', *, *, #111178, .F. ) ;
#23909 = AXIS2_PLACEMENT_3D ( 'NONE', #22063, #13498, #112368 ) ;
#23910 = DIRECTION ( 'NONE',  ( -1.000000000000000000, -0.000000000000000000, -0.000000000000000000 ) ) ;
#23911 = ORIENTED_EDGE ( 'NONE', *, *, #33062, .T. ) ;
#23912 = CARTESIAN_POINT ( 'NONE',  ( 87.50000000000002842, 4.871203238224194543, 5.733266569811710234 ) ) ;
#23913 = EDGE_LOOP ( 'NONE', ( #7529, #121263 ) ) ;
#23914 = DIRECTION ( 'NONE',  ( 0.000000000000000000, -0.9999939076577903929, 0.003490651415223739937 ) ) ;
#23915 = PLANE ( 'NONE',  #115846 ) ;
#23916 = FACE_OUTER_BOUND ( 'NONE', #70140, .T. ) ;
#23917 = DIRECTION ( 'NONE',  ( 0.000000000000000000, 0.000000000000000000, 1.000000000000000000 ) ) ;
#23918 = ORIENTED_EDGE ( 'NONE', *, *, #58639, .F. ) ;
#23919 = DIRECTION ( 'NONE',  ( 0.000000000000000000, 1.000000000000000000, 0.000000000000000000 ) ) ;
#23920 = ADVANCED_FACE ( 'NONE', ( #79311 ), #44197, .T. ) ;
#23922 = DIRECTION ( 'NONE',  ( 0.000000000000000000, 1.000000000000000000, 0.000000000000000000 ) ) ;
#23921 = CIRCLE ( 'NONE', #42723, 0.06509327318403745899 ) ;
#23923 = ORIENTED_EDGE ( 'NONE', *, *, #125004, .F. ) ;
#23924 = EDGE_LOOP ( 'NONE', ( #122711, #47616 ) ) ;
#23925 = AXIS2_PLACEMENT_3D ( 'NONE', #98571, #110347, #39061 ) ;
#23926 = AXIS2_PLACEMENT_3D ( 'NONE', #22112, #92104, #32579 ) ;
#23927 = VERTEX_POINT ( 'NONE', #48551 ) ;
#23928 = DIRECTION ( 'NONE',  ( -0.000000000000000000, 1.000000000000000000, -0.000000000000000000 ) ) ;
#23929 = DIRECTION ( 'NONE',  ( 0.000000000000000000, 1.000000000000000000, 0.000000000000000000 ) ) ;
#23930 = CARTESIAN_POINT ( 'NONE',  ( 184.8177083336747160, 4.367472073101515306, 7.564683531250000925 ) ) ;
#23931 = DIRECTION ( 'NONE',  ( -1.000000000000000000, -0.000000000000000000, -0.000000000000000000 ) ) ;
#23932 = EDGE_CURVE ( 'NONE', #125419, #43068, #21213, .T. ) ;
#23933 = AXIS2_PLACEMENT_3D ( 'NONE', #87853, #106849, #27025 ) ;
#23934 = AXIS2_PLACEMENT_3D ( 'NONE', #60139, #20837, #99404 ) ;
#23935 = CARTESIAN_POINT ( 'NONE',  ( 17.34778429999903082, 2.317753570193296309, -4.873671836816706460 ) ) ;
#23936 = CONICAL_SURFACE ( 'NONE', #55325, 0.1000000000000000472, 0.003490658503988666988 ) ;
#23937 = DIRECTION ( 'NONE',  ( 0.000000000000000000, -0.000000000000000000, 1.000000000000000000 ) ) ;
#23938 = ORIENTED_EDGE ( 'NONE', *, *, #52943, .F. ) ;
#23939 = CIRCLE ( 'NONE', #55329, 0.06509327318403745899 ) ;
#23940 = DIRECTION ( 'NONE',  ( -4.274815082592931898E-19, -0.9999939076577903929, -0.003490651415223739937 ) ) ;
#23941 = EDGE_LOOP ( 'NONE', ( #37812, #32547 ) ) ;
#23942 = DIRECTION ( 'NONE',  ( 0.000000000000000000, 1.000000000000000000, 0.000000000000000000 ) ) ;
#23943 = CARTESIAN_POINT ( 'NONE',  ( -7.499999999999976907, 2.500000000000000000, 4.230127018922196669 ) ) ;
#23944 = FACE_OUTER_BOUND ( 'NONE', #125431, .T. ) ;
#23945 = DIRECTION ( 'NONE',  ( 0.000000000000000000, 0.000000000000000000, -1.000000000000000000 ) ) ;
#23946 = ORIENTED_EDGE ( 'NONE', *, *, #101432, .F. ) ;
#23947 = FACE_OUTER_BOUND ( 'NONE', #98465, .T. ) ;
#23949 = ORIENTED_EDGE ( 'NONE', *, *, #123992, .T. ) ;
#23948 = CARTESIAN_POINT ( 'NONE',  ( -12.04999999999999538, 2.500000000000000000, 2.165063509461097713 ) ) ;
#23950 = VECTOR ( 'NONE', #56426, 1000.000000000000000 ) ;
#23951 = ORIENTED_EDGE ( 'NONE', *, *, #45296, .T. ) ;
#23952 = FACE_OUTER_BOUND ( 'NONE', #1428, .T. ) ;
#23953 = EDGE_CURVE ( 'NONE', #109941, #13735, #106883, .T. ) ;
#23954 = VERTEX_POINT ( 'NONE', #128422 ) ;
#23955 = ORIENTED_EDGE ( 'NONE', *, *, #54605, .F. ) ;
#23956 = DIRECTION ( 'NONE',  ( -4.274815082592931898E-19, -0.9999939076577903929, -0.003490651415223739937 ) ) ;
#23957 = VERTEX_POINT ( 'NONE', #69456 ) ;
#23958 = CARTESIAN_POINT ( 'NONE',  ( 15.05551045036142277, 2.483581587658090672, -4.666934263335500432 ) ) ;
#23959 = LINE ( 'NONE', #54060, #109080 ) ;
#23960 = CIRCLE ( 'NONE', #86652, 0.06509327318403745899 ) ;
#23961 = DIRECTION ( 'NONE',  ( -0.000000000000000000, 1.000000000000000000, -0.000000000000000000 ) ) ;
#23962 = ADVANCED_FACE ( 'NONE', ( #26981, #109391 ), #99589, .T. ) ;
#23963 = VECTOR ( 'NONE', #129610, 1000.000000000000000 ) ;
#23964 = EDGE_LOOP ( 'NONE', ( #18882, #706 ) ) ;
#23965 = CARTESIAN_POINT ( 'NONE',  ( -8.550000000000011369, 2.500000000000000000, -2.411473670974877859 ) ) ;
#23967 = VERTEX_POINT ( 'NONE', #14868 ) ;
#23966 = LINE ( 'NONE', #14123, #50033 ) ;
#23968 = EDGE_CURVE ( 'NONE', #79506, #51796, #25316, .T. ) ;
#23969 = DIRECTION ( 'NONE',  ( -4.274815082592931898E-19, -0.9999939076577903929, -0.003490651415223739937 ) ) ;
#23970 = CARTESIAN_POINT ( 'NONE',  ( -1.650000000000035660, 12.50000000000000000, 2.857883832488649301 ) ) ;
#23971 = ADVANCED_FACE ( 'NONE', ( #100225 ), #110993, .T. ) ;
#23972 = ORIENTED_EDGE ( 'NONE', *, *, #102582, .T. ) ;
#23973 = VECTOR ( 'NONE', #125848, 1000.000000000000000 ) ;
#23974 = VERTEX_POINT ( 'NONE', #79 ) ;
#23975 = EDGE_CURVE ( 'NONE', #50117, #38386, #42563, .T. ) ;
#23977 = EDGE_LOOP ( 'NONE', ( #57395, #111708, #20440, #108121 ) ) ;
#23976 = VECTOR ( 'NONE', #57650, 1000.000000000000000 ) ;
#23978 = EDGE_LOOP ( 'NONE', ( #75175, #27062 ) ) ;
#23979 = CARTESIAN_POINT ( 'NONE',  ( -11.24999999999996447, 2.500000000000000000, -6.495190528383298911 ) ) ;
#23980 = DIRECTION ( 'NONE',  ( 0.000000000000000000, 0.000000000000000000, 1.000000000000000000 ) ) ;
#23981 = DIRECTION ( 'NONE',  ( 0.000000000000000000, 1.000000000000000000, 0.000000000000000000 ) ) ;
#23982 = ADVANCED_FACE ( 'NONE', ( #1362 ), #14838, .T. ) ;
#23983 = FACE_BOUND ( 'NONE', #36376, .T. ) ;
#23984 = ORIENTED_EDGE ( 'NONE', *, *, #28127, .F. ) ;
#23985 = CARTESIAN_POINT ( 'NONE',  ( 185.8229166673494319, -4.445597072760122614, 7.699999999999998401 ) ) ;
#23986 = DIRECTION ( 'NONE',  ( 0.000000000000000000, 0.000000000000000000, -1.000000000000000000 ) ) ;
#23987 = FACE_OUTER_BOUND ( 'NONE', #6956, .T. ) ;
#23988 = FACE_OUTER_BOUND ( 'NONE', #12036, .T. ) ;
#23989 = CARTESIAN_POINT ( 'NONE',  ( -3.750000000000027978, 2.500000000000000000, 7.088010851410848190 ) ) ;
#23990 = CIRCLE ( 'NONE', #61364, 0.1000000000000000472 ) ;
#23991 = CARTESIAN_POINT ( 'NONE',  ( -6.900000000000015454, 2.500000000000000000, 3.983716857408420076 ) ) ;
#23992 = CIRCLE ( 'NONE', #72030, 0.1000000000000002554 ) ;
#23993 = DIRECTION ( 'NONE',  ( 0.000000000000000000, 1.000000000000000000, 0.000000000000000000 ) ) ;
#23994 = ORIENTED_EDGE ( 'NONE', *, *, #59202, .T. ) ;
#23995 = ORIENTED_EDGE ( 'NONE', *, *, #53424, .T. ) ;
#23996 = ORIENTED_EDGE ( 'NONE', *, *, #85012, .F. ) ;
#23997 = ORIENTED_EDGE ( 'NONE', *, *, #95400, .F. ) ;
#23998 = EDGE_LOOP ( 'NONE', ( #23938, #26795 ) ) ;
#23999 = FACE_OUTER_BOUND ( 'NONE', #26931, .T. ) ;
#24000 = CARTESIAN_POINT ( 'NONE',  ( 8.549999999999920774, 2.500000000000000000, -2.611473670974877592 ) ) ;
#24001 = VERTEX_POINT ( 'NONE', #124214 ) ;
#24002 = FACE_BOUND ( 'NONE', #41213, .T. ) ;
#24003 = DIRECTION ( 'NONE',  ( 0.000000000000000000, 1.000000000000000000, 0.000000000000000000 ) ) ;
#24004 = EDGE_CURVE ( 'NONE', #41537, #95313, #83653, .T. ) ;
#24005 = CIRCLE ( 'NONE', #7255, 0.06509327318403745899 ) ;
#24007 = VERTEX_POINT ( 'NONE', #120511 ) ;
#24006 = CIRCLE ( 'NONE', #122212, 0.09999999999999982514 ) ;
#24008 = AXIS2_PLACEMENT_3D ( 'NONE', #103231, #105146, #13545 ) ;
#24009 = CARTESIAN_POINT ( 'NONE',  ( 105.5000000000000142, 0.000000000000000000, 0.000000000000000000 ) ) ;
#24010 = CARTESIAN_POINT ( 'NONE',  ( -10.40000000000000391, 12.50000000000000000, -3.637306695894645614 ) ) ;
#24011 = DIRECTION ( 'NONE',  ( 0.000000000000000000, 0.000000000000000000, 1.000000000000000000 ) ) ;
#24012 = ORIENTED_EDGE ( 'NONE', *, *, #50547, .T. ) ;
#24013 = CARTESIAN_POINT ( 'NONE',  ( -4.200000000000025935, 2.500000000000000000, -2.385244779468109755E-15 ) ) ;
#24014 = ADVANCED_FACE ( 'NONE', ( #113760 ), #50463, .T. ) ;
#24015 = AXIS2_PLACEMENT_3D ( 'NONE', #100373, #50615, #90539 ) ;
#24016 = ORIENTED_EDGE ( 'NONE', *, *, #51526, .T. ) ;
#24017 = AXIS2_PLACEMENT_3D ( 'NONE', #126250, #45120, #55577 ) ;
#24018 = ORIENTED_EDGE ( 'NONE', *, *, #126087, .F. ) ;
#24019 = VERTEX_POINT ( 'NONE', #33902 ) ;
#24020 = ADVANCED_FACE ( 'NONE', ( #121147 ), #54193, .T. ) ;
#24021 = CARTESIAN_POINT ( 'NONE',  ( 5.399999999999936406, 2.500000000000000000, -3.637306695894650055 ) ) ;
#24022 = CIRCLE ( 'NONE', #82610, 0.09999999999999982514 ) ;
#24023 = DIRECTION ( 'NONE',  ( -0.000000000000000000, -1.000000000000000000, -0.000000000000000000 ) ) ;
#24024 = CARTESIAN_POINT ( 'NONE',  ( 10.39999999999991154, 12.50000000000000000, 3.572213422710607489 ) ) ;
#24026 = ORIENTED_EDGE ( 'NONE', *, *, #44976, .F. ) ;
#24025 = EDGE_CURVE ( 'NONE', #81317, #72217, #21009, .T. ) ;
#24027 = CARTESIAN_POINT ( 'NONE',  ( 12.89999999999990266, 2.500000000000000000, 5.022947341949748790 ) ) ;
#24028 = ADVANCED_FACE ( 'NONE', ( #3795 ), #23425, .T. ) ;
#24029 = CONICAL_SURFACE ( 'NONE', #107650, 0.09999999999999982514, 0.003490658503988666988 ) ;
#24030 = AXIS2_PLACEMENT_3D ( 'NONE', #10771, #11446, #16874 ) ;
#24031 = CARTESIAN_POINT ( 'NONE',  ( -11.44999999999999751, 2.500000000000000000, 6.841600689897072485 ) ) ;
#24033 = EDGE_CURVE ( 'NONE', #94365, #117010, #92217, .T. ) ;
#24032 = CARTESIAN_POINT ( 'NONE',  ( -7.500000000000015099, 12.50000000000000000, -5.088040615133791356 ) ) ;
#24034 = DIRECTION ( 'NONE',  ( 0.000000000000000000, -0.000000000000000000, 1.000000000000000000 ) ) ;
#24036 = VERTEX_POINT ( 'NONE', #81231 ) ;
#24035 = CONICAL_SURFACE ( 'NONE', #118012, 0.1000000000000002554, 0.003490658503988666988 ) ;
#24037 = DIRECTION ( 'NONE',  ( 0.000000000000000000, 0.000000000000000000, 1.000000000000000000 ) ) ;
#24038 = ORIENTED_EDGE ( 'NONE', *, *, #31428, .T. ) ;
#24039 = CARTESIAN_POINT ( 'NONE',  ( 0.1999999999999571565, 2.500000000000000000, 3.983716857408420076 ) ) ;
#24040 = EDGE_CURVE ( 'NONE', #71367, #4913, #79708, .T. ) ;
#24041 = EDGE_CURVE ( 'NONE', #119467, #45959, #123609, .T. ) ;
#24042 = EDGE_LOOP ( 'NONE', ( #58536, #101094, #28340, #93534 ) ) ;
#24043 = ORIENTED_EDGE ( 'NONE', *, *, #115427, .F. ) ;
#24044 = CARTESIAN_POINT ( 'NONE',  ( -6.450000000000016165, 2.500000000000000000, 2.411473670974873862 ) ) ;
#24045 = DIRECTION ( 'NONE',  ( 0.000000000000000000, 0.000000000000000000, 1.000000000000000000 ) ) ;
#24046 = PLANE ( 'NONE',  #15368 ) ;
#24047 = DIRECTION ( 'NONE',  ( 0.000000000000000000, 0.000000000000000000, 1.000000000000000000 ) ) ;
#24048 = CARTESIAN_POINT ( 'NONE',  ( 184.5000000000000000, -7.430520870378829024, -1.418378131116527108 ) ) ;
#24049 = ORIENTED_EDGE ( 'NONE', *, *, #77034, .F. ) ;
#24050 = ORIENTED_EDGE ( 'NONE', *, *, #36034, .F. ) ;
#24051 = CARTESIAN_POINT ( 'NONE',  ( 10.44999999999991402, 12.50000000000000000, -2.165063509461101710 ) ) ;
#24052 = DIRECTION ( 'NONE',  ( -0.000000000000000000, -1.000000000000000000, -0.000000000000000000 ) ) ;
#24053 = DIRECTION ( 'NONE',  ( 0.000000000000000000, -0.9999939076577903929, 0.003490651415223739937 ) ) ;
#24054 = ORIENTED_EDGE ( 'NONE', *, *, #79409, .T. ) ;
#24055 = EDGE_LOOP ( 'NONE', ( #40407, #101634, #105706, #26760 ) ) ;
#24056 = CARTESIAN_POINT ( 'NONE',  ( -3.300000000000027800, 2.500000000000000000, -0.1000000000000022815 ) ) ;
#24057 = AXIS2_PLACEMENT_3D ( 'NONE', #84050, #74894, #95175 ) ;
#24058 = EDGE_LOOP ( 'NONE', ( #96539, #56752 ) ) ;
#24060 = VECTOR ( 'NONE', #80340, 1000.000000000000000 ) ;
#24059 = DIRECTION ( 'NONE',  ( 0.000000000000000000, 0.000000000000000000, -1.000000000000000000 ) ) ;
#24061 = DIRECTION ( 'NONE',  ( 0.000000000000000000, 0.000000000000000000, 1.000000000000000000 ) ) ;
#24062 = EDGE_LOOP ( 'NONE', ( #35587, #7662, #9192, #38991 ) ) ;
#24063 = FACE_OUTER_BOUND ( 'NONE', #27302, .T. ) ;
#24064 = FACE_OUTER_BOUND ( 'NONE', #20539, .T. ) ;
#24065 = DIRECTION ( 'NONE',  ( 0.000000000000000000, 1.000000000000000000, 0.000000000000000000 ) ) ;
#24066 = PLANE ( 'NONE',  #37546 ) ;
#24067 = ORIENTED_EDGE ( 'NONE', *, *, #95407, .T. ) ;
#24068 = CIRCLE ( 'NONE', #65910, 0.1000000000000002554 ) ;
#24069 = DIRECTION ( 'NONE',  ( 0.000000000000000000, 0.000000000000000000, 1.000000000000000000 ) ) ;
#24070 = ADVANCED_FACE ( 'NONE', ( #24727 ), #77642, .T. ) ;
#24072 = AXIS2_PLACEMENT_3D ( 'NONE', #86283, #13683, #16248 ) ;
#24071 = DIRECTION ( 'NONE',  ( 0.000000000000000000, -0.9999939076577903929, 0.003490651415223739937 ) ) ;
#24073 = EDGE_LOOP ( 'NONE', ( #3929, #120563 ) ) ;
#24074 = ORIENTED_EDGE ( 'NONE', *, *, #73601, .T. ) ;
#24075 = CARTESIAN_POINT ( 'NONE',  ( 184.1510416670080588, 4.367472073101518859, -7.564683531249999149 ) ) ;
#24076 = DIRECTION ( 'NONE',  ( 0.000000000000000000, 0.000000000000000000, 1.000000000000000000 ) ) ;
#24077 = DIRECTION ( 'NONE',  ( 0.000000000000000000, 0.000000000000000000, -1.000000000000000000 ) ) ;
#24078 = DIRECTION ( 'NONE',  ( 0.000000000000000000, 0.000000000000000000, -1.000000000000000000 ) ) ;
#24079 = CARTESIAN_POINT ( 'NONE',  ( -0.4500000000000402012, 2.500000000000000000, 2.165063509461097713 ) ) ;
#24080 = EDGE_CURVE ( 'NONE', #43648, #3765, #40018, .T. ) ;
#24081 = CONICAL_SURFACE ( 'NONE', #120220, 0.1000000000000002554, 0.003490658503988666988 ) ;
#24082 = DIRECTION ( 'NONE',  ( -4.274815082592931898E-19, -0.9999939076577903929, -0.003490651415223739937 ) ) ;
#24083 = AXIS2_PLACEMENT_3D ( 'NONE', #122061, #92592, #111585 ) ;
#24084 = CARTESIAN_POINT ( 'NONE',  ( -8.100000000000010303, 12.50000000000000000, 3.983716857408420964 ) ) ;
#24085 = DIRECTION ( 'NONE',  ( -0.000000000000000000, -1.000000000000000000, -0.000000000000000000 ) ) ;
#24086 = DIRECTION ( 'NONE',  ( 0.000000000000000000, 1.000000000000000000, 0.000000000000000000 ) ) ;
#24087 = DIRECTION ( 'NONE',  ( -4.274815082592931898E-19, -0.9999939076577903929, -0.003490651415223739937 ) ) ;
#24088 = DIRECTION ( 'NONE',  ( 0.000000000000000000, 1.000000000000000000, 0.000000000000000000 ) ) ;
#24089 = ORIENTED_EDGE ( 'NONE', *, *, #14077, .T. ) ;
#24090 = EDGE_LOOP ( 'NONE', ( #44824, #72379, #101026, #126010 ) ) ;
#24091 = ORIENTED_EDGE ( 'NONE', *, *, #111334, .T. ) ;
#24092 = VERTEX_POINT ( 'NONE', #104568 ) ;
#24093 = CIRCLE ( 'NONE', #11555, 0.06509327318403745899 ) ;
#24094 = DIRECTION ( 'NONE',  ( 0.000000000000000000, 0.000000000000000000, 1.000000000000000000 ) ) ;
#24095 = DIRECTION ( 'NONE',  ( 0.000000000000000000, -0.000000000000000000, 1.000000000000000000 ) ) ;
#24096 = VERTEX_POINT ( 'NONE', #37764 ) ;
#24097 = CARTESIAN_POINT ( 'NONE',  ( 6.249999999999968914, 12.50000000000000000, -6.560283801567339701 ) ) ;
#24098 = DIRECTION ( 'NONE',  ( 0.000000000000000000, 1.000000000000000000, 0.000000000000000000 ) ) ;
#24100 = ORIENTED_EDGE ( 'NONE', *, *, #49311, .T. ) ;
#24099 = LINE ( 'NONE', #52918, #64174 ) ;
#24101 = CIRCLE ( 'NONE', #97250, 0.09999999999999982514 ) ;
#24102 = DIRECTION ( 'NONE',  ( 0.000000000000000000, 1.000000000000000000, 0.000000000000000000 ) ) ;
#24103 = DIRECTION ( 'NONE',  ( 0.000000000000000000, 1.000000000000000000, 0.000000000000000000 ) ) ;
#24104 = ORIENTED_EDGE ( 'NONE', *, *, #100965, .T. ) ;
#24105 = CONICAL_SURFACE ( 'NONE', #86878, 0.1000000000000002554, 0.003490658503988666988 ) ;
#24106 = AXIS2_PLACEMENT_3D ( 'NONE', #50924, #71851, #13551 ) ;
#24107 = AXIS2_PLACEMENT_3D ( 'NONE', #83323, #33577, #73474 ) ;
#24108 = VERTEX_POINT ( 'NONE', #116307 ) ;
#24109 = VERTEX_POINT ( 'NONE', #16802 ) ;
#24110 = ORIENTED_EDGE ( 'NONE', *, *, #22204, .T. ) ;
#24111 = CARTESIAN_POINT ( 'NONE',  ( 12.09999999999990550, 12.50000000000000000, 3.702399969078682407 ) ) ;
#24112 = AXIS2_PLACEMENT_3D ( 'NONE', #35067, #24581, #23285 ) ;
#24113 = CARTESIAN_POINT ( 'NONE',  ( 184.7500000000000000, 9.429780353434619030E-16, -7.700000000000000178 ) ) ;
#24114 = DIRECTION ( 'NONE',  ( 0.000000000000000000, 1.000000000000000000, 0.000000000000000000 ) ) ;
#24115 = CONICAL_SURFACE ( 'NONE', #17843, 0.09999999999999982514, 0.003490658503988666988 ) ;
#24116 = DIRECTION ( 'NONE',  ( 0.000000000000000000, 1.000000000000000000, 0.000000000000000000 ) ) ;
#24118 = EDGE_CURVE ( 'NONE', #94495, #115716, #73443, .T. ) ;
#24117 = CIRCLE ( 'NONE', #15778, 0.06509327318403745899 ) ;
#24119 = VERTEX_POINT ( 'NONE', #116950 ) ;
#24120 = CARTESIAN_POINT ( 'NONE',  ( 9.549999999999915445, 2.500000000000000000, -2.165063509461101710 ) ) ;
#24121 = ORIENTED_EDGE ( 'NONE', *, *, #67545, .T. ) ;
#24122 = CARTESIAN_POINT ( 'NONE',  ( -0.2000000000000347888, 2.500000000000000000, 0.3464101615137758494 ) ) ;
#24124 = EDGE_CURVE ( 'NONE', #21163, #42755, #111076, .T. ) ;
#24123 = CARTESIAN_POINT ( 'NONE',  ( 10.28037028451869084, -2.499999999999618527, -9.136909653094715367 ) ) ;
#24125 = EDGE_CURVE ( 'NONE', #95225, #119631, #66564, .T. ) ;
#24126 = FACE_OUTER_BOUND ( 'NONE', #107497, .T. ) ;
#24127 = CARTESIAN_POINT ( 'NONE',  ( 19.61395058415580905, -2.556813634648763767, 4.305699210823851431 ) ) ;
#24128 = EDGE_CURVE ( 'NONE', #86700, #38783, #75746, .T. ) ;
#24129 = ORIENTED_EDGE ( 'NONE', *, *, #61888, .T. ) ;
#24130 = ORIENTED_EDGE ( 'NONE', *, *, #126274, .F. ) ;
#24131 = ADVANCED_FACE ( 'NONE', ( #7645 ), #83989, .T. ) ;
#24133 = VERTEX_POINT ( 'NONE', #55479 ) ;
#24132 = EDGE_CURVE ( 'NONE', #43500, #97794, #97330, .T. ) ;
#24134 = DIRECTION ( 'NONE',  ( 0.000000000000000000, 0.000000000000000000, 1.000000000000000000 ) ) ;
#24135 = DIRECTION ( 'NONE',  ( 0.000000000000000000, 0.000000000000000000, 1.000000000000000000 ) ) ;
#24136 = DIRECTION ( 'NONE',  ( -4.274815082592931898E-19, -0.9999939076577903929, -0.003490651415223739937 ) ) ;
#24137 = ADVANCED_FACE ( 'NONE', ( #26661 ), #96664, .T. ) ;
#24138 = FACE_BOUND ( 'NONE', #37199, .T. ) ;
#24139 = CARTESIAN_POINT ( 'NONE',  ( 2.949999999999943334, 12.50000000000000000, 6.495190528383297135 ) ) ;
#24140 = CIRCLE ( 'NONE', #118216, 0.1000000000000000056 ) ;
#24141 = DIRECTION ( 'NONE',  ( 0.000000000000000000, 0.000000000000000000, 1.000000000000000000 ) ) ;
#24142 = CARTESIAN_POINT ( 'NONE',  ( 9.149999999999915090, 12.50000000000000000, 6.495190528383297135 ) ) ;
#24143 = CARTESIAN_POINT ( 'NONE',  ( 187.3385416670080872, 6.551208109652274736, 3.782341765625001351 ) ) ;
#24144 = AXIS2_PLACEMENT_3D ( 'NONE', #81331, #112725, #100952 ) ;
#24145 = CARTESIAN_POINT ( 'NONE',  ( 8.549999999999924327, 12.50000000000000000, -6.841600689897077814 ) ) ;
#24146 = DIRECTION ( 'NONE',  ( 0.000000000000000000, -1.846105847067148515E-16, -1.000000000000000000 ) ) ;
#24147 = ORIENTED_EDGE ( 'NONE', *, *, #19461, .F. ) ;
#24148 = AXIS2_PLACEMENT_3D ( 'NONE', #57174, #17891, #97104 ) ;
#24149 = AXIS2_PLACEMENT_3D ( 'NONE', #91435, #83563, #101256 ) ;
#24150 = CARTESIAN_POINT ( 'NONE',  ( 7.499999999999960032, 12.50000000000000000, 0.06509327318403515528 ) ) ;
#24151 = ORIENTED_EDGE ( 'NONE', *, *, #125367, .F. ) ;
#24152 = VERTEX_POINT ( 'NONE', #47596 ) ;
#24153 = ORIENTED_EDGE ( 'NONE', *, *, #40240, .T. ) ;
#24154 = ORIENTED_EDGE ( 'NONE', *, *, #40411, .F. ) ;
#24155 = DIRECTION ( 'NONE',  ( 0.000000000000000000, -0.000000000000000000, 1.000000000000000000 ) ) ;
#24156 = FACE_BOUND ( 'NONE', #95139, .T. ) ;
#24157 = PLANE ( 'NONE',  #34730 ) ;
#24158 = AXIS2_PLACEMENT_3D ( 'NONE', #51033, #58906, #28806 ) ;
#24159 = ORIENTED_EDGE ( 'NONE', *, *, #104424, .F. ) ;
#24160 = FACE_OUTER_BOUND ( 'NONE', #19977, .T. ) ;
#24161 = CARTESIAN_POINT ( 'NONE',  ( -0.6500000000000389910, 12.50000000000000000, -6.148780366869526226 ) ) ;
#24162 = ORIENTED_EDGE ( 'NONE', *, *, #61807, .T. ) ;
#24163 = DIRECTION ( 'NONE',  ( 0.000000000000000000, 1.000000000000000000, 0.000000000000000000 ) ) ;
#24164 = DIRECTION ( 'NONE',  ( 0.000000000000000000, 0.000000000000000000, 1.000000000000000000 ) ) ;
#24165 = CIRCLE ( 'NONE', #109854, 0.06509327318403745899 ) ;
#24166 = AXIS2_PLACEMENT_3D ( 'NONE', #39501, #29653, #69566 ) ;
#24167 = EDGE_CURVE ( 'NONE', #34349, #41184, #58882, .T. ) ;
#24168 = ORIENTED_EDGE ( 'NONE', *, *, #128451, .F. ) ;
#24169 = ADVANCED_FACE ( 'NONE', ( #86858 ), #71377, .T. ) ;
#24170 = DIRECTION ( 'NONE',  ( 0.000000000000000000, 0.000000000000000000, 1.000000000000000000 ) ) ;
#24171 = FACE_OUTER_BOUND ( 'NONE', #39006, .T. ) ;
#24172 = ADVANCED_FACE ( 'NONE', ( #25348 ), #81848, .T. ) ;
#24173 = ORIENTED_EDGE ( 'NONE', *, *, #115019, .T. ) ;
#24174 = DIRECTION ( 'NONE',  ( 0.000000000000000000, -0.9999939076577903929, 0.003490651415223739937 ) ) ;
#24175 = CARTESIAN_POINT ( 'NONE',  ( 10.44999999999991402, 2.500000000000000000, 6.395190528383296602 ) ) ;
#24176 = AXIS2_PLACEMENT_3D ( 'NONE', #3742, #75070, #83610 ) ;
#24178 = EDGE_CURVE ( 'NONE', #129312, #127662, #123696, .T. ) ;
#24177 = FACE_OUTER_BOUND ( 'NONE', #45699, .T. ) ;
#24179 = EDGE_CURVE ( 'NONE', #20597, #121932, #14921, .T. ) ;
#24180 = ORIENTED_EDGE ( 'NONE', *, *, #41958, .F. ) ;
#24181 = ORIENTED_EDGE ( 'NONE', *, *, #129083, .T. ) ;
#24182 = DIRECTION ( 'NONE',  ( 0.000000000000000000, -0.9999939076577903929, 0.003490651415223739937 ) ) ;
#24183 = CIRCLE ( 'NONE', #17912, 0.09999999999999982514 ) ;
#24184 = ORIENTED_EDGE ( 'NONE', *, *, #100088, .T. ) ;
#24185 = DIRECTION ( 'NONE',  ( 0.000000000000000000, 0.000000000000000000, 1.000000000000000000 ) ) ;
#24186 = FACE_OUTER_BOUND ( 'NONE', #20519, .T. ) ;
#24187 = EDGE_CURVE ( 'NONE', #9410, #35149, #40100, .T. ) ;
#24188 = EDGE_CURVE ( 'NONE', #16690, #15822, #113248, .T. ) ;
#24189 = AXIS2_PLACEMENT_3D ( 'NONE', #17217, #66342, #38186 ) ;
#24190 = ORIENTED_EDGE ( 'NONE', *, *, #70582, .F. ) ;
#24191 = CIRCLE ( 'NONE', #55492, 0.1000000000000002554 ) ;
#24192 = PLANE ( 'NONE',  #97745 ) ;
#24193 = DIRECTION ( 'NONE',  ( -0.000000000000000000, 1.000000000000000000, -0.000000000000000000 ) ) ;
#24194 = DIRECTION ( 'NONE',  ( 0.000000000000000000, 0.000000000000000000, 1.000000000000000000 ) ) ;
#24195 =( BOUNDED_CURVE ( )  B_SPLINE_CURVE ( 2, ( #69447, #104079, #92314, #61593, #23577, #113907, #43886 ),
 .UNSPECIFIED., .F., .F. ) 
 B_SPLINE_CURVE_WITH_KNOTS ( ( 3, 2, 2, 3 ),
 ( 0.2142857142857144681, 0.2380952380952383041, 0.2619047619047621955, 0.2857142857142859760 ),
 .UNSPECIFIED. ) 
 CURVE ( )  GEOMETRIC_REPRESENTATION_ITEM ( )  RATIONAL_B_SPLINE_CURVE ( ( 0.9999999999999988898, 0.8660254037844397068, 1.000000000000000000, 0.8660254037844387076, 1.000000000000000000, 0.8660254037844371533, 1.000000000000001554 ) ) 
 REPRESENTATION_ITEM ( '' )  );
#24196 = CARTESIAN_POINT ( 'NONE',  ( 10.59999999999990905, 2.500000000000000000, -3.983716857408426293 ) ) ;
#24198 = EDGE_CURVE ( 'NONE', #59055, #13197, #92319, .T. ) ;
#24197 = DIRECTION ( 'NONE',  ( 0.000000000000000000, -0.9999939076577903929, 0.003490651415223739937 ) ) ;
#24199 = AXIS2_PLACEMENT_3D ( 'NONE', #113910, #34720, #54970 ) ;
#24200 = ORIENTED_EDGE ( 'NONE', *, *, #77814, .T. ) ;
#24201 = ORIENTED_EDGE ( 'NONE', *, *, #109636, .F. ) ;
#24202 = DIRECTION ( 'NONE',  ( -0.000000000000000000, -1.000000000000000000, -0.000000000000000000 ) ) ;
#24203 = CARTESIAN_POINT ( 'NONE',  ( 106.6633797337217970, 5.997582082682869853, -4.829774833287197922 ) ) ;
#24206 = ORIENTED_EDGE ( 'NONE', *, *, #123458, .T. ) ;
#24205 = ORIENTED_EDGE ( 'NONE', *, *, #38781, .T. ) ;
#24204 = CONICAL_SURFACE ( 'NONE', #103628, 0.1000000000000000472, 0.003490658503988666988 ) ;
#24207 = EDGE_LOOP ( 'NONE', ( #122225, #763, #7666, #36833 ) ) ;
#24208 = PLANE ( 'NONE',  #35391 ) ;
#24210 = AXIS2_PLACEMENT_3D ( 'NONE', #105479, #66185, #5966 ) ;
#24209 = CARTESIAN_POINT ( 'NONE',  ( 11.64999999999990443, 12.50000000000000000, -7.122917578226816815 ) ) ;
#24211 = CARTESIAN_POINT ( 'NONE',  ( 14.14999999999989377, 2.500000000000000000, -1.372243186433550033 ) ) ;
#24212 = AXIS2_PLACEMENT_3D ( 'NONE', #83915, #83300, #44016 ) ;
#24213 = DIRECTION ( 'NONE',  ( 1.000000000000000000, 0.000000000000000000, 0.000000000000000000 ) ) ;
#24214 = FACE_OUTER_BOUND ( 'NONE', #66218, .T. ) ;
#24215 = DIRECTION ( 'NONE',  ( 0.000000000000000000, 0.000000000000000000, -1.000000000000000000 ) ) ;
#24216 = CARTESIAN_POINT ( 'NONE',  ( 21.24754738303277435, 0.7337760880902381988, 4.182111650399361835 ) ) ;
#24217 = AXIS2_PLACEMENT_3D ( 'NONE', #96195, #108606, #66097 ) ;
#24218 = DIRECTION ( 'NONE',  ( 0.000000000000000000, 1.000000000000000000, 0.000000000000000000 ) ) ;
#24219 = DIRECTION ( 'NONE',  ( -0.000000000000000000, 1.000000000000000000, -0.000000000000000000 ) ) ;
#24220 = DIRECTION ( 'NONE',  ( 0.000000000000000000, 0.000000000000000000, -1.000000000000000000 ) ) ;
#24221 = ORIENTED_EDGE ( 'NONE', *, *, #81343, .F. ) ;
#24222 = CARTESIAN_POINT ( 'NONE',  ( -1.650000000000034772, 2.500000000000000000, 2.165063509461097713 ) ) ;
#24223 = ORIENTED_EDGE ( 'NONE', *, *, #97859, .F. ) ;
#24224 = ORIENTED_EDGE ( 'NONE', *, *, #34103, .T. ) ;
#24225 = CARTESIAN_POINT ( 'NONE',  ( -1.700000000000035261, 2.500000000000000000, 4.330127018922196314 ) ) ;
#24226 = CARTESIAN_POINT ( 'NONE',  ( 10.39999999999991154, 2.500000000000000000, 4.922947341949748257 ) ) ;
#24227 = AXIS2_PLACEMENT_3D ( 'NONE', #64097, #72642, #14334 ) ;
#24228 = DIRECTION ( 'NONE',  ( -0.000000000000000000, -1.000000000000000000, -0.000000000000000000 ) ) ;
#24229 = CARTESIAN_POINT ( 'NONE',  ( 165.4999999999999716, 0.000000000000000000, 2.000000000000000000 ) ) ;
#24230 = ADVANCED_FACE ( 'NONE', ( #45019 ), #364, .T. ) ;
#24232 = CARTESIAN_POINT ( 'NONE',  ( 0.1999999999999636513, 12.50000000000000000, -0.3464101615137760715 ) ) ;
#24231 = PRODUCT_DEFINITION_SHAPE ( 'NONE', 'NONE',  #129620 ) ;
#24233 = DIRECTION ( 'NONE',  ( 0.000000000000000000, 1.000000000000000000, 0.000000000000000000 ) ) ;
#24234 = PLANE ( 'NONE',  #103274 ) ;
#24235 = ORIENTED_EDGE ( 'NONE', *, *, #63851, .F. ) ;
#24236 = CARTESIAN_POINT ( 'NONE',  ( -5.850000000000018296, 2.500000000000000000, 7.288010851410849256 ) ) ;
#24237 = VECTOR ( 'NONE', #82471, 1000.000000000000000 ) ;
#24238 = AXIS2_PLACEMENT_3D ( 'NONE', #63765, #23842, #103693 ) ;
#24239 = DIRECTION ( 'NONE',  ( -4.274815082592931898E-19, -0.9999939076577903929, -0.003490651415223739937 ) ) ;
#24240 = ORIENTED_EDGE ( 'NONE', *, *, #97600, .T. ) ;
#24241 = ORIENTED_EDGE ( 'NONE', *, *, #79850, .T. ) ;
#24242 = CIRCLE ( 'NONE', #97389, 0.1000000000000002554 ) ;
#24243 = VERTEX_POINT ( 'NONE', #27942 ) ;
#24244 = ORIENTED_EDGE ( 'NONE', *, *, #78946, .T. ) ;
#24245 = CARTESIAN_POINT ( 'NONE',  ( -5.200000000000024158, 2.500000000000000000, -4.676537180435977881 ) ) ;
#24246 = CARTESIAN_POINT ( 'NONE',  ( 13.09999999999989839, 2.500000000000000000, -0.3464101615137783474 ) ) ;
#24247 = AXIS2_PLACEMENT_3D ( 'NONE', #122984, #54241, #94157 ) ;
#24248 = CARTESIAN_POINT ( 'NONE',  ( 12.89999999999990088, 12.50000000000000000, 4.265033745738159077 ) ) ;
#24249 = LINE ( 'NONE', #113925, #88364 ) ;
#24251 = VECTOR ( 'NONE', #30958, 1000.000000000000000 ) ;
#24250 = AXIS2_PLACEMENT_3D ( 'NONE', #96151, #7768, #5824 ) ;
#24252 = DIRECTION ( 'NONE',  ( -0.000000000000000000, -1.000000000000000000, -0.000000000000000000 ) ) ;
#24253 = VERTEX_POINT ( 'NONE', #107794 ) ;
#24254 = FACE_OUTER_BOUND ( 'NONE', #21328, .T. ) ;
#24255 = DIRECTION ( 'NONE',  ( -0.000000000000000000, 1.000000000000000000, -0.000000000000000000 ) ) ;
#24256 = CARTESIAN_POINT ( 'NONE',  ( 2.499999999999945377, 12.50000000000000000, 5.022947341949748790 ) ) ;
#24257 = VERTEX_POINT ( 'NONE', #124861 ) ;
#24258 = ORIENTED_EDGE ( 'NONE', *, *, #67268, .T. ) ;
#24259 = VERTEX_POINT ( 'NONE', #35204 ) ;
#24260 = DIRECTION ( 'NONE',  ( 0.000000000000000000, 0.000000000000000000, 1.000000000000000000 ) ) ;
#24261 = FACE_OUTER_BOUND ( 'NONE', #108872, .T. ) ;
#24262 = DIRECTION ( 'NONE',  ( -4.274815082592931898E-19, -0.9999939076577903929, -0.003490651415223739937 ) ) ;
#24263 = EDGE_CURVE ( 'NONE', #93088, #37898, #10852, .T. ) ;
#24264 = VERTEX_POINT ( 'NONE', #29252 ) ;
#24265 = DIRECTION ( 'NONE',  ( 0.000000000000000000, 0.000000000000000000, 1.000000000000000000 ) ) ;
#24266 = DIRECTION ( 'NONE',  ( -0.000000000000000000, 1.000000000000000000, -0.000000000000000000 ) ) ;
#24267 = EDGE_CURVE ( 'NONE', #116552, #11967, #118255, .T. ) ;
#24268 = CARTESIAN_POINT ( 'NONE',  ( 13.54999999999990123, 2.500000000000000000, 1.918653347947321564 ) ) ;
#24269 = DIRECTION ( 'NONE',  ( 0.000000000000000000, 1.000000000000000000, 0.000000000000000000 ) ) ;
#24270 = EDGE_CURVE ( 'NONE', #79131, #16954, #120839, .T. ) ;
#24271 = CIRCLE ( 'NONE', #114167, 0.1000000000000002554 ) ;
#24272 = FACE_OUTER_BOUND ( 'NONE', #61933, .T. ) ;
#24273 = VECTOR ( 'NONE', #41969, 1000.000000000000000 ) ;
#24274 = ORIENTED_EDGE ( 'NONE', *, *, #79556, .T. ) ;
#24275 = ADVANCED_FACE ( 'NONE', ( #69805 ), #39081, .T. ) ;
#24276 = ADVANCED_FACE ( 'NONE', ( #10241 ), #396, .F. ) ;
#24277 = ORIENTED_EDGE ( 'NONE', *, *, #50038, .T. ) ;
#24278 = EDGE_CURVE ( 'NONE', #36641, #43898, #28596, .T. ) ;
#24280 = ADVANCED_FACE ( 'NONE', ( #58063 ), #17070, .T. ) ;
#24279 = DIRECTION ( 'NONE',  ( 0.000000000000000000, -0.9999939076577903929, 0.003490651415223739937 ) ) ;
#24281 = EDGE_CURVE ( 'NONE', #95824, #25449, #119506, .T. ) ;
#24282 = CARTESIAN_POINT ( 'NONE',  ( 2.099999999999948574, 12.50000000000000000, 4.330127018922196314 ) ) ;
#24283 = DIRECTION ( 'NONE',  ( -4.274815082592931898E-19, -0.9999939076577903929, -0.003490651415223739937 ) ) ;
#24284 = DIRECTION ( 'NONE',  ( -0.000000000000000000, -1.000000000000000000, -0.000000000000000000 ) ) ;
#24286 = AXIS2_PLACEMENT_3D ( 'NONE', #88863, #37198, #67247 ) ;
#24285 = AXIS2_PLACEMENT_3D ( 'NONE', #18620, #48740, #88652 ) ;
#24287 = LINE ( 'NONE', #94299, #52270 ) ;
#24288 = VERTEX_POINT ( 'NONE', #41017 ) ;
#24289 = ORIENTED_EDGE ( 'NONE', *, *, #16648, .F. ) ;
#24290 = DIRECTION ( 'NONE',  ( -0.000000000000000000, 1.000000000000000000, -0.000000000000000000 ) ) ;
#24291 = DIRECTION ( 'NONE',  ( 0.000000000000000000, 0.000000000000000000, 1.000000000000000000 ) ) ;
#24292 = ADVANCED_FACE ( 'NONE', ( #88117 ), #100720, .T. ) ;
#24293 = FACE_OUTER_BOUND ( 'NONE', #31451, .T. ) ;
#24294 = DIRECTION ( 'NONE',  ( 0.000000000000000000, 0.000000000000000000, 1.000000000000000000 ) ) ;
#24295 = ORIENTED_EDGE ( 'NONE', *, *, #112788, .T. ) ;
#24297 = CONICAL_SURFACE ( 'NONE', #91197, 0.1000000000000002554, 0.003490658503988666988 ) ;
#24296 = CIRCLE ( 'NONE', #74557, 0.09999999999999999167 ) ;
#24299 = EDGE_CURVE ( 'NONE', #26010, #42850, #80920, .T. ) ;
#24298 = CARTESIAN_POINT ( 'NONE',  ( 1.649999999999950617, 12.50000000000000000, -2.165063509461101710 ) ) ;
#24300 = AXIS2_PLACEMENT_3D ( 'NONE', #55750, #17080, #57029 ) ;
#24301 = CARTESIAN_POINT ( 'NONE',  ( 8.549999999999924327, 2.500000000000000000, -6.841600689897077814 ) ) ;
#24302 = EDGE_LOOP ( 'NONE', ( #121389, #123177 ) ) ;
#24303 = CARTESIAN_POINT ( 'NONE',  ( -9.350000000000006750, 2.500000000000000000, -1.818653347947325916 ) ) ;
#24304 = ORIENTED_EDGE ( 'NONE', *, *, #71448, .T. ) ;
#24305 = CARTESIAN_POINT ( 'NONE',  ( -6.050000000000022027, 12.50000000000000000, -6.148780366869526226 ) ) ;
#24306 = VERTEX_POINT ( 'NONE', #98593 ) ;
#24307 = CARTESIAN_POINT ( 'NONE',  ( -0.8500000000000382805, 2.500000000000000000, -2.857883832488653741 ) ) ;
#24308 = DIRECTION ( 'NONE',  ( 0.000000000000000000, 0.000000000000000000, 1.000000000000000000 ) ) ;
#24309 = ORIENTED_EDGE ( 'NONE', *, *, #50040, .F. ) ;
#24310 = ORIENTED_EDGE ( 'NONE', *, *, #105416, .F. ) ;
#24311 = CARTESIAN_POINT ( 'NONE',  ( 185.7135416670080588, 4.367472073101518859, -7.564683531249999149 ) ) ;
#24312 = DIRECTION ( 'NONE',  ( -0.000000000000000000, 1.000000000000000000, -0.000000000000000000 ) ) ;
#24313 = AXIS2_PLACEMENT_3D ( 'NONE', #10948, #22755, #50919 ) ;
#24314 = CARTESIAN_POINT ( 'NONE',  ( 184.5052083336747444, -6.551208109652278289, 3.782341765624995134 ) ) ;
#24315 = CARTESIAN_POINT ( 'NONE',  ( -0.6500000000000403233, 12.50000000000000000, 6.148780366869520009 ) ) ;
#24316 = CONICAL_SURFACE ( 'NONE', #13838, 0.09999999999999982514, 0.003490658503988666988 ) ;
#24317 = CARTESIAN_POINT ( 'NONE',  ( -6.850000000000013856, 2.500000000000000000, 6.148780366869520897 ) ) ;
#24318 = DIRECTION ( 'NONE',  ( 0.000000000000000000, 1.000000000000000000, 0.000000000000000000 ) ) ;
#24319 = FACE_OUTER_BOUND ( 'NONE', #121455, .T. ) ;
#24320 = AXIS2_PLACEMENT_3D ( 'NONE', #108537, #88902, #78457 ) ;
#24321 = EDGE_CURVE ( 'NONE', #81450, #14967, #71475, .T. ) ;
#24322 = CARTESIAN_POINT ( 'NONE',  ( 1.249999999999952038, 12.50000000000000000, 5.802370205355744659 ) ) ;
#24323 = AXIS2_PLACEMENT_3D ( 'NONE', #92087, #31263, #40445 ) ;
#24324 = EDGE_CURVE ( 'NONE', #122022, #80208, #78350, .T. ) ;
#24325 = AXIS2_PLACEMENT_3D ( 'NONE', #2733, #70842, #50545 ) ;
#24326 = ORIENTED_EDGE ( 'NONE', *, *, #85896, .F. ) ;
#24327 = CIRCLE ( 'NONE', #41078, 0.1000000000000000056 ) ;
#24328 = ADVANCED_FACE ( 'NONE', ( #120200 ), #29882, .T. ) ;
#24329 = ORIENTED_EDGE ( 'NONE', *, *, #64829, .T. ) ;
#24330 = CARTESIAN_POINT ( 'NONE',  ( -3.350000000000028955, 12.50000000000000000, 2.165063509461097713 ) ) ;
#24331 = FACE_OUTER_BOUND ( 'NONE', #32264, .T. ) ;
#24332 = CARTESIAN_POINT ( 'NONE',  ( 4.999999999999935163, 12.50000000000000000, 3.637306695894644726 ) ) ;
#24333 = DIRECTION ( 'NONE',  ( 0.000000000000000000, 1.000000000000000000, 0.000000000000000000 ) ) ;
#24335 = VERTEX_POINT ( 'NONE', #119534 ) ;
#24334 = ORIENTED_EDGE ( 'NONE', *, *, #83726, .T. ) ;
#24336 = LINE ( 'NONE', #85815, #112274 ) ;
#24337 = ORIENTED_EDGE ( 'NONE', *, *, #5042, .F. ) ;
#24338 = ADVANCED_FACE ( 'NONE', ( #18763 ), #42153, .T. ) ;
#24339 = PLANE ( 'NONE',  #19941 ) ;
#24340 = CARTESIAN_POINT ( 'NONE',  ( 18.70618316909975221, -2.558637580971239611, 2.503050677946469182 ) ) ;
#24341 = AXIS2_PLACEMENT_3D ( 'NONE', #105270, #45076, #74527 ) ;
#24343 = ORIENTED_EDGE ( 'NONE', *, *, #128975, .T. ) ;
#24342 = ADVANCED_FACE ( 'NONE', ( #118901 ), #6605, .T. ) ;
#24344 = CARTESIAN_POINT ( 'NONE',  ( 2.499999999999947153, 2.500000000000000000, 3.737306695894644371 ) ) ;
#24345 = PLANE ( 'NONE',  #22214 ) ;
#24346 = DIRECTION ( 'NONE',  ( 0.000000000000000000, 0.000000000000000000, -1.000000000000000000 ) ) ;
#24349 = EDGE_CURVE ( 'NONE', #3070, #92934, #99276, .T. ) ;
#24348 = AXIS2_PLACEMENT_3D ( 'NONE', #39340, #38021, #117854 ) ;
#24347 = VECTOR ( 'NONE', #120948, 1000.000000000000000 ) ;
#24350 = FACE_OUTER_BOUND ( 'NONE', #105777, .T. ) ;
#24351 = DIRECTION ( 'NONE',  ( -4.274815082592931898E-19, -0.9999939076577903929, -0.003490651415223739937 ) ) ;
#24352 = DIRECTION ( 'NONE',  ( 0.000000000000000000, 0.000000000000000000, 1.000000000000000000 ) ) ;
#24353 = DIRECTION ( 'NONE',  ( -0.000000000000000000, -1.000000000000000000, -0.000000000000000000 ) ) ;
#24354 = DIRECTION ( 'NONE',  ( 0.000000000000000000, -0.9999939076577903929, 0.003490651415223739937 ) ) ;
#24356 = EDGE_CURVE ( 'NONE', #22443, #26454, #48411, .T. ) ;
#24355 = CARTESIAN_POINT ( 'NONE',  ( 0.4499999999999569344, 2.500000000000000000, -2.065063509461102065 ) ) ;
#24357 = VERTEX_POINT ( 'NONE', #52103 ) ;
#24358 = ORIENTED_EDGE ( 'NONE', *, *, #24187, .F. ) ;
#24359 = VERTEX_POINT ( 'NONE', #32487 ) ;
#24360 = CARTESIAN_POINT ( 'NONE',  ( -3.150000000000029665, 2.500000000000000000, 6.741600689897071952 ) ) ;
#24361 = ORIENTED_EDGE ( 'NONE', *, *, #59767, .F. ) ;
#24363 = ORIENTED_EDGE ( 'NONE', *, *, #1368, .T. ) ;
#24362 = VERTEX_POINT ( 'NONE', #1693 ) ;
#24364 = ORIENTED_EDGE ( 'NONE', *, *, #49351, .F. ) ;
#24365 = CARTESIAN_POINT ( 'NONE',  ( 11.64999999999990621, 12.50000000000000000, -2.230156782645139391 ) ) ;
#24366 = CARTESIAN_POINT ( 'NONE',  ( 10.64999999999991331, 2.500000000000000000, 6.941600689897073018 ) ) ;
#24367 = CARTESIAN_POINT ( 'NONE',  ( 186.9583333333332860, 4.445597072760133273, 7.699999999999975309 ) ) ;
#24368 = DIRECTION ( 'NONE',  ( 0.000000000000000000, 0.000000000000000000, 1.000000000000000000 ) ) ;
#24369 = CARTESIAN_POINT ( 'NONE',  ( -12.69999999999999396, 2.500000000000000000, 0.2464101615137776757 ) ) ;
#24370 = EDGE_CURVE ( 'NONE', #16509, #98934, #21339, .T. ) ;
#24371 = VERTEX_POINT ( 'NONE', #122773 ) ;
#24372 = CARTESIAN_POINT ( 'NONE',  ( 10.39999999999991509, 2.500000000000000000, -0.6928203230275542523 ) ) ;
#24373 = ORIENTED_EDGE ( 'NONE', *, *, #28290, .T. ) ;
#24375 = ORIENTED_EDGE ( 'NONE', *, *, #11089, .T. ) ;
#24374 = AXIS2_PLACEMENT_3D ( 'NONE', #77312, #108058, #119169 ) ;
#24376 = EDGE_LOOP ( 'NONE', ( #35580, #95950 ) ) ;
#24377 = AXIS2_PLACEMENT_3D ( 'NONE', #75276, #115177, #55647 ) ;
#24378 = CARTESIAN_POINT ( 'NONE',  ( -9.350000000000004974, 12.50000000000000000, 6.841600689897072485 ) ) ;
#24379 = VERTEX_POINT ( 'NONE', #41659 ) ;
#24380 = EDGE_LOOP ( 'NONE', ( #74689, #16497 ) ) ;
#24381 = VERTEX_POINT ( 'NONE', #112313 ) ;
#24382 = CARTESIAN_POINT ( 'NONE',  ( 10.59999999999990905, 2.500000000000000000, -3.883716857408426648 ) ) ;
#24384 = VECTOR ( 'NONE', #24635, 1000.000000000000000 ) ;
#24383 = AXIS2_PLACEMENT_3D ( 'NONE', #10564, #69490, #9295 ) ;
#24385 = DIRECTION ( 'NONE',  ( 0.000000000000000000, 1.000000000000000000, 0.000000000000000000 ) ) ;
#24386 = DIRECTION ( 'NONE',  ( 0.000000000000000000, 0.000000000000000000, 1.000000000000000000 ) ) ;
#24387 = ADVANCED_FACE ( 'NONE', ( #71742 ), #111669, .T. ) ;
#24388 = CARTESIAN_POINT ( 'NONE',  ( -8.100000000000013856, 2.500000000000000000, -0.3464101615137782364 ) ) ;
#24389 = CARTESIAN_POINT ( 'NONE',  ( 6.249999999999967137, 2.500000000000000000, 6.495190528383297135 ) ) ;
#24390 = FACE_OUTER_BOUND ( 'NONE', #117107, .T. ) ;
#24391 = DIRECTION ( 'NONE',  ( 0.000000000000000000, 0.000000000000000000, 1.000000000000000000 ) ) ;
#24393 = AXIS2_PLACEMENT_3D ( 'NONE', #93681, #43949, #84510 ) ;
#24392 = CIRCLE ( 'NONE', #34878, 0.06509327318403745899 ) ;
#24394 = VERTEX_POINT ( 'NONE', #51467 ) ;
#24395 = DIRECTION ( 'NONE',  ( 0.000000000000000000, 0.000000000000000000, 1.000000000000000000 ) ) ;
#24396 = ORIENTED_EDGE ( 'NONE', *, *, #21592, .T. ) ;
#24397 = CARTESIAN_POINT ( 'NONE',  ( 185.9479166673494603, -6.668395609140176816, -3.850000000000003642 ) ) ;
#24398 = ORIENTED_EDGE ( 'NONE', *, *, #61082, .F. ) ;
#24399 = ADVANCED_FACE ( 'NONE', ( #113597 ), #14083, .T. ) ;
#24400 = VERTEX_POINT ( 'NONE', #73023 ) ;
#24401 = DIRECTION ( 'NONE',  ( 0.000000000000000000, -0.9999939076577903929, 0.003490651415223739937 ) ) ;
#24402 = CARTESIAN_POINT ( 'NONE',  ( 184.0260416670080588, -6.551208109652273848, -3.782341765625003571 ) ) ;
#24403 = DIRECTION ( 'NONE',  ( 0.000000000000000000, 0.000000000000000000, -1.000000000000000000 ) ) ;
#24404 = ORIENTED_EDGE ( 'NONE', *, *, #41220, .T. ) ;
#24405 = DIRECTION ( 'NONE',  ( 0.000000000000000000, 1.000000000000000000, 0.000000000000000000 ) ) ;
#24406 = ORIENTED_EDGE ( 'NONE', *, *, #47275, .F. ) ;
#24407 = LINE ( 'NONE', #14570, #41512 ) ;
#24408 = PLANE ( 'NONE',  #18021 ) ;
#24409 = DIRECTION ( 'NONE',  ( 0.000000000000000000, 1.000000000000000000, 0.000000000000000000 ) ) ;
#24410 = AXIS2_PLACEMENT_3D ( 'NONE', #6927, #105808, #6288 ) ;
#24411 = LINE ( 'NONE', #23776, #55581 ) ;
#24412 = CIRCLE ( 'NONE', #97561, 0.1000000000000002554 ) ;
#24413 = CARTESIAN_POINT ( 'NONE',  ( -0.8500000000000395017, 12.50000000000000000, 2.165063509461097713 ) ) ;
#24414 = ORIENTED_EDGE ( 'NONE', *, *, #90047, .F. ) ;
#24415 = CONICAL_SURFACE ( 'NONE', #9747, 0.09999999999999999167, 0.003490658503988666988 ) ;
#24416 = AXIS2_PLACEMENT_3D ( 'NONE', #41734, #39162, #120280 ) ;
#24417 = EDGE_LOOP ( 'NONE', ( #114502, #113111 ) ) ;
#24418 = CIRCLE ( 'NONE', #82919, 0.06509327318403745899 ) ;
#24419 = CARTESIAN_POINT ( 'NONE',  ( 9.399999999999915090, 12.50000000000000000, -4.676537180435977881 ) ) ;
#24420 = DIRECTION ( 'NONE',  ( 0.000000000000000000, 0.000000000000000000, 1.000000000000000000 ) ) ;
#24421 = CIRCLE ( 'NONE', #99742, 0.06509327318403745899 ) ;
#24422 = EDGE_CURVE ( 'NONE', #126052, #114688, #52735, .T. ) ;
#24423 = CARTESIAN_POINT ( 'NONE',  ( 184.8385416670080872, 6.551208109652274736, 3.782341765625001351 ) ) ;
#24424 = CARTESIAN_POINT ( 'NONE',  ( -11.25000000000000000, 2.500000000000000000, 7.288010851410849256 ) ) ;
#24425 = DIRECTION ( 'NONE',  ( 0.000000000000000000, 0.000000000000000000, -1.000000000000000000 ) ) ;
#24426 = DIRECTION ( 'NONE',  ( 0.000000000000000000, 1.000000000000000000, 0.000000000000000000 ) ) ;
#24427 = DIRECTION ( 'NONE',  ( 0.000000000000000000, -0.9999939076577903929, 0.003490651415223739937 ) ) ;
#24428 = VERTEX_POINT ( 'NONE', #82207 ) ;
#24429 = CONICAL_SURFACE ( 'NONE', #107963, 0.1000000000000002554, 0.003490658503988666988 ) ;
#24430 = EDGE_CURVE ( 'NONE', #57186, #79091, #109029, .T. ) ;
#24431 = DIRECTION ( 'NONE',  ( 0.000000000000000000, 1.000000000000000000, 0.000000000000000000 ) ) ;
#24433 = AXIS2_PLACEMENT_3D ( 'NONE', #94350, #4660, #44619 ) ;
#24432 = CIRCLE ( 'NONE', #41187, 0.06509327318403745899 ) ;
#24434 = DIRECTION ( 'NONE',  ( 0.000000000000000000, 1.000000000000000000, 0.000000000000000000 ) ) ;
#24435 = DIRECTION ( 'NONE',  ( 0.000000000000000000, 1.000000000000000000, 0.000000000000000000 ) ) ;
#24436 = EDGE_LOOP ( 'NONE', ( #110069, #128129 ) ) ;
#24437 = EDGE_CURVE ( 'NONE', #65711, #54010, #54744, .T. ) ;
#24438 = EDGE_CURVE ( 'NONE', #31853, #16422, #103129, .T. ) ;
#24439 = ADVANCED_FACE ( 'NONE', ( #42953 ), #92509, .T. ) ;
#24440 = ADVANCED_FACE ( 'NONE', ( #42283 ), #31988, .T. ) ;
#24441 = CARTESIAN_POINT ( 'NONE',  ( -5.850000000000022737, 12.50000000000000000, -2.230156782645139391 ) ) ;
#24442 = EDGE_LOOP ( 'NONE', ( #49303, #3888, #97712, #76884 ) ) ;
#24443 = ADVANCED_FACE ( 'NONE', ( #61283 ), #86234, .T. ) ;
#24444 = CARTESIAN_POINT ( 'NONE',  ( 1.649999999999951061, 2.500000000000000000, -6.395190528383301931 ) ) ;
#24445 = EDGE_LOOP ( 'NONE', ( #80663, #29291, #98992, #6003 ) ) ;
#24446 = CARTESIAN_POINT ( 'NONE',  ( 8.749999999999921840, 12.50000000000000000, -5.737276932171712751 ) ) ;
#24447 = DIRECTION ( 'NONE',  ( 0.000000000000000000, 0.000000000000000000, -1.000000000000000000 ) ) ;
#24449 = EDGE_CURVE ( 'NONE', #4367, #6762, #19436, .T. ) ;
#24448 = VECTOR ( 'NONE', #5654, 1000.000000000000000 ) ;
#24450 = DIRECTION ( 'NONE',  ( -0.000000000000000000, 1.000000000000000000, -0.000000000000000000 ) ) ;
#24451 = EDGE_LOOP ( 'NONE', ( #122681, #112502 ) ) ;
#24452 = EDGE_CURVE ( 'NONE', #15915, #92369, #69518, .T. ) ;
#24454 = ADVANCED_FACE ( 'NONE', ( #83504 ), #102485, .T. ) ;
#24453 = CARTESIAN_POINT ( 'NONE',  ( -3.100000000000028511, 12.50000000000000000, -3.983716857408426293 ) ) ;
#24455 = DIRECTION ( 'NONE',  ( -0.000000000000000000, 1.000000000000000000, -0.000000000000000000 ) ) ;
#24456 = EDGE_CURVE ( 'NONE', #29616, #34192, #117614, .T. ) ;
#24457 = ORIENTED_EDGE ( 'NONE', *, *, #68644, .F. ) ;
#24458 = CARTESIAN_POINT ( 'NONE',  ( 11.64999999999990443, 12.50000000000000000, -7.188010851410854052 ) ) ;
#24459 = AXIS2_PLACEMENT_3D ( 'NONE', #101957, #128867, #50282 ) ;
#24460 = ORIENTED_EDGE ( 'NONE', *, *, #115850, .T. ) ;
#24461 = AXIS2_PLACEMENT_3D ( 'NONE', #106360, #96518, #6842 ) ;
#24462 = VERTEX_POINT ( 'NONE', #91374 ) ;
#24463 = DIRECTION ( 'NONE',  ( -4.274815082592931898E-19, -0.9999939076577903929, -0.003490651415223739937 ) ) ;
#24464 = CARTESIAN_POINT ( 'NONE',  ( -3.950000000000026379, 12.50000000000000000, 2.511473670974873507 ) ) ;
#24465 = CARTESIAN_POINT ( 'NONE',  ( 3.349999999999942801, 2.500000000000000000, 2.857883832488649301 ) ) ;
#24466 = ORIENTED_EDGE ( 'NONE', *, *, #25859, .T. ) ;
#24467 = DIRECTION ( 'NONE',  ( 0.000000000000000000, 0.000000000000000000, -1.000000000000000000 ) ) ;
#24468 = CARTESIAN_POINT ( 'NONE',  ( -2.700000000000031264, 2.500000000000000000, 4.676537180435972552 ) ) ;
#24469 = ORIENTED_EDGE ( 'NONE', *, *, #1538, .T. ) ;
#24471 = AXIS2_PLACEMENT_3D ( 'NONE', #102648, #64022, #103950 ) ;
#24470 = CIRCLE ( 'NONE', #103892, 0.06509327318403745899 ) ;
#24472 = FACE_OUTER_BOUND ( 'NONE', #28764, .T. ) ;
#24473 = FACE_OUTER_BOUND ( 'NONE', #101116, .T. ) ;
#24474 = DIRECTION ( 'NONE',  ( 0.000000000000000000, -0.000000000000000000, 1.000000000000000000 ) ) ;
#24475 = CARTESIAN_POINT ( 'NONE',  ( 4.549999999999939426, 2.500000000000000000, -2.165063509461101710 ) ) ;
#24476 = DIRECTION ( 'NONE',  ( 0.000000000000000000, -0.9999939076577903929, 0.003490651415223739937 ) ) ;
#24477 = CARTESIAN_POINT ( 'NONE',  ( -2.700000000000030376, 2.500000000000000000, 4.083716857408421497 ) ) ;
#24478 = CARTESIAN_POINT ( 'NONE',  ( 10.59999999999990905, 2.500000000000000000, -4.676537180435978769 ) ) ;
#24480 = AXIS2_PLACEMENT_3D ( 'NONE', #62157, #50380, #102066 ) ;
#24479 = AXIS2_PLACEMENT_3D ( 'NONE', #402, #30556, #55959 ) ;
#24481 = AXIS2_PLACEMENT_3D ( 'NONE', #104952, #63775, #64402 ) ;
#24482 = ORIENTED_EDGE ( 'NONE', *, *, #78265, .T. ) ;
#24483 = EDGE_LOOP ( 'NONE', ( #63828, #81850 ) ) ;
#24484 = VERTEX_POINT ( 'NONE', #54032 ) ;
#24485 = ORIENTED_EDGE ( 'NONE', *, *, #50010, .F. ) ;
#24486 = CARTESIAN_POINT ( 'NONE',  ( 7.949999999999922018, 2.500000000000000000, 6.395190528383296602 ) ) ;
#24487 = DIRECTION ( 'NONE',  ( 0.000000000000000000, -0.000000000000000000, 1.000000000000000000 ) ) ;
#24488 = LINE ( 'NONE', #126560, #90704 ) ;
#24489 = EDGE_LOOP ( 'NONE', ( #68978, #119574, #121638, #124222 ) ) ;
#24490 = FACE_BOUND ( 'NONE', #13100, .T. ) ;
#24491 = CARTESIAN_POINT ( 'NONE',  ( -10.85000000000000142, 2.500000000000000000, -6.495190528383298911 ) ) ;
#24492 = DIRECTION ( 'NONE',  ( 0.000000000000000000, -0.9999939076577903929, 0.003490651415223739937 ) ) ;
#24493 = ADVANCED_FACE ( 'NONE', ( #44195 ), #25705, .T. ) ;
#24494 = CARTESIAN_POINT ( 'NONE',  ( 187.5000000000000000, 6.368163355566236381E-16, 5.200000000000000178 ) ) ;
#24495 = CARTESIAN_POINT ( 'NONE',  ( 7.499999999999927169, 12.50000000000000000, 3.637306695894644726 ) ) ;
#24496 = ADVANCED_FACE ( 'NONE', ( #116801 ), #77929, .T. ) ;
#24497 = DIRECTION ( 'NONE',  ( 0.000000000000000000, 1.000000000000000000, 0.000000000000000000 ) ) ;
#24498 = LINE ( 'NONE', #64416, #97664 ) ;
#24499 = CARTESIAN_POINT ( 'NONE',  ( -0.6000000000000383915, 2.500000000000000000, -3.983716857408426293 ) ) ;
#24500 = DIRECTION ( 'NONE',  ( 0.000000000000000000, 0.000000000000000000, 1.000000000000000000 ) ) ;
#24501 = FACE_OUTER_BOUND ( 'NONE', #4649, .T. ) ;
#24502 = CONICAL_SURFACE ( 'NONE', #20297, 0.1000000000000000056, 0.003490658503988666988 ) ;
#24503 = VECTOR ( 'NONE', #13219, 1000.000000000000000 ) ;
#24505 = EDGE_CURVE ( 'NONE', #14107, #91704, #15218, .T. ) ;
#24504 = CARTESIAN_POINT ( 'NONE',  ( -12.04999999999999538, 12.50000000000000000, 2.165063509461097713 ) ) ;
#24506 = ORIENTED_EDGE ( 'NONE', *, *, #13342, .F. ) ;
#24508 = ORIENTED_EDGE ( 'NONE', *, *, #40424, .T. ) ;
#24507 = VECTOR ( 'NONE', #78061, 1000.000000000000000 ) ;
#24509 = EDGE_LOOP ( 'NONE', ( #41394, #1768 ) ) ;
#24510 = ORIENTED_EDGE ( 'NONE', *, *, #87935, .F. ) ;
#24511 = CARTESIAN_POINT ( 'NONE',  ( 13.94999999999989804, 2.500000000000000000, 1.818653347947321475 ) ) ;
#24512 = ORIENTED_EDGE ( 'NONE', *, *, #83551, .F. ) ;
#24513 = CARTESIAN_POINT ( 'NONE',  ( -4.550000000000022915, 12.50000000000000000, 6.495190528383297135 ) ) ;
#24514 = ORIENTED_EDGE ( 'NONE', *, *, #54871, .F. ) ;
#24516 = ORIENTED_EDGE ( 'NONE', *, *, #58667, .F. ) ;
#24515 = CIRCLE ( 'NONE', #55896, 0.06509327318403741736 ) ;
#24517 = CIRCLE ( 'NONE', #106077, 2.250000000000001776 ) ;
#24518 = CONICAL_SURFACE ( 'NONE', #120662, 0.1000000000000002554, 0.003490658503988666988 ) ;
#24519 = DIRECTION ( 'NONE',  ( -0.000000000000000000, -1.000000000000000000, -0.000000000000000000 ) ) ;
#24520 = CARTESIAN_POINT ( 'NONE',  ( 3.299999999999942979, 2.500000000000000000, 4.330127018922196314 ) ) ;
#24521 = DIRECTION ( 'NONE',  ( 0.000000000000000000, 0.000000000000000000, -1.000000000000000000 ) ) ;
#24522 = DIRECTION ( 'NONE',  ( 0.000000000000000000, 1.000000000000000000, 0.000000000000000000 ) ) ;
#24523 = AXIS2_PLACEMENT_3D ( 'NONE', #94220, #56221, #46400 ) ;
#24524 = ORIENTED_EDGE ( 'NONE', *, *, #61194, .F. ) ;
#24525 = ORIENTED_EDGE ( 'NONE', *, *, #39990, .F. ) ;
#24527 = AXIS2_PLACEMENT_3D ( 'NONE', #61374, #68111, #1152 ) ;
#24526 = CONICAL_SURFACE ( 'NONE', #76757, 0.1000000000000002554, 0.003490658503988666988 ) ;
#24528 = ORIENTED_EDGE ( 'NONE', *, *, #91998, .F. ) ;
#24530 = VERTEX_POINT ( 'NONE', #56585 ) ;
#24529 = DIRECTION ( 'NONE',  ( 0.000000000000000000, 0.000000000000000000, 1.000000000000000000 ) ) ;
#24531 = CARTESIAN_POINT ( 'NONE',  ( 184.7083333333333428, -4.445597072760175017, -7.699999999999898037 ) ) ;
#24532 = EDGE_LOOP ( 'NONE', ( #5488, #89716, #100803, #6643 ) ) ;
#24533 = ORIENTED_EDGE ( 'NONE', *, *, #115171, .T. ) ;
#24534 = DIRECTION ( 'NONE',  ( -0.000000000000000000, -1.000000000000000000, -0.000000000000000000 ) ) ;
#24535 = PLANE ( 'NONE',  #83032 ) ;
#24536 = DIRECTION ( 'NONE',  ( -0.000000000000000000, -1.000000000000000000, -0.000000000000000000 ) ) ;
#24537 = FACE_OUTER_BOUND ( 'NONE', #96766, .T. ) ;
#24538 = LINE ( 'NONE', #54627, #87913 ) ;
#24539 = AXIS2_PLACEMENT_3D ( 'NONE', #97690, #37504, #88507 ) ;
#24540 = ORIENTED_EDGE ( 'NONE', *, *, #98030, .T. ) ;
#24541 = DIRECTION ( 'NONE',  ( -4.274815082592931898E-19, -0.9999939076577903929, -0.003490651415223739937 ) ) ;
#24542 = ORIENTED_EDGE ( 'NONE', *, *, #66849, .F. ) ;
#24543 = CARTESIAN_POINT ( 'NONE',  ( 17.50000000000000000, 2.499999999999999556, 1.333333333333336590 ) ) ;
#24544 = ORIENTED_EDGE ( 'NONE', *, *, #56789, .T. ) ;
#24545 = FACE_OUTER_BOUND ( 'NONE', #55239, .T. ) ;
#24546 = DIRECTION ( 'NONE',  ( -1.000000000000000000, 0.000000000000000000, 0.000000000000000000 ) ) ;
#24547 = EDGE_CURVE ( 'NONE', #14028, #39660, #47439, .T. ) ;
#24548 = FACE_OUTER_BOUND ( 'NONE', #67227, .T. ) ;
#24549 = EDGE_CURVE ( 'NONE', #66106, #52738, #55326, .T. ) ;
#24550 = DIRECTION ( 'NONE',  ( 0.000000000000000000, 0.000000000000000000, 1.000000000000000000 ) ) ;
#24551 = VERTEX_POINT ( 'NONE', #96503 ) ;
#24552 = CARTESIAN_POINT ( 'NONE',  ( -1.250000000000037970, 12.50000000000000000, 7.188010851410848723 ) ) ;
#24553 = CONICAL_SURFACE ( 'NONE', #97700, 0.1000000000000002554, 0.003490658503988666988 ) ;
#24554 = AXIS2_PLACEMENT_3D ( 'NONE', #59218, #3501, #51337 ) ;
#24555 = FACE_OUTER_BOUND ( 'NONE', #31313, .T. ) ;
#24556 = ORIENTED_EDGE ( 'NONE', *, *, #20023, .F. ) ;
#24557 = ORIENTED_EDGE ( 'NONE', *, *, #164, .F. ) ;
#24559 = EDGE_LOOP ( 'NONE', ( #36919, #34579, #3426, #104820 ) ) ;
#24558 = EDGE_CURVE ( 'NONE', #5496, #93617, #124707, .T. ) ;
#24560 = CARTESIAN_POINT ( 'NONE',  ( 9.599999999999914380, 12.50000000000000000, -4.265033745738164406 ) ) ;
#24561 = DIRECTION ( 'NONE',  ( 0.000000000000000000, 0.000000000000000000, -1.000000000000000000 ) ) ;
#24562 = CARTESIAN_POINT ( 'NONE',  ( 185.2343750003414016, 8.734944146203032389, 5.348610694689227483E-16 ) ) ;
#24563 = DIRECTION ( 'NONE',  ( 1.000000000000000000, 0.000000000000000000, 0.000000000000000000 ) ) ;
#24565 = VECTOR ( 'NONE', #102015, 1000.000000000000000 ) ;
#24564 = CONICAL_SURFACE ( 'NONE', #116489, 0.09999999999999982514, 0.003490658503988666988 ) ;
#24566 = VECTOR ( 'NONE', #53199, 1000.000000000000000 ) ;
#24567 = DIRECTION ( 'NONE',  ( -0.000000000000000000, 1.000000000000000000, -0.000000000000000000 ) ) ;
#24568 = LINE ( 'NONE', #57254, #17269 ) ;
#24569 = AXIS2_PLACEMENT_3D ( 'NONE', #6836, #17970, #16662 ) ;
#24570 = ORIENTED_EDGE ( 'NONE', *, *, #60264, .F. ) ;
#24571 = FACE_OUTER_BOUND ( 'NONE', #115179, .T. ) ;
#24572 = CONICAL_SURFACE ( 'NONE', #97723, 0.09999999999999982514, 0.003490658503988666988 ) ;
#24573 = EDGE_CURVE ( 'NONE', #53445, #85857, #65410, .T. ) ;
#24574 = ORIENTED_EDGE ( 'NONE', *, *, #80141, .T. ) ;
#24575 = CARTESIAN_POINT ( 'NONE',  ( 4.999999999999933387, 2.500000000000000000, 4.922947341949748257 ) ) ;
#24576 = DIRECTION ( 'NONE',  ( 0.000000000000000000, 1.000000000000000000, 0.000000000000000000 ) ) ;
#24577 = DIRECTION ( 'NONE',  ( -4.274815082592931898E-19, -0.9999939076577903929, -0.003490651415223739937 ) ) ;
#24578 = ORIENTED_EDGE ( 'NONE', *, *, #47233, .T. ) ;
#24579 = EDGE_CURVE ( 'NONE', #31361, #33917, #52800, .T. ) ;
#24580 = CIRCLE ( 'NONE', #114459, 0.06509327318403745899 ) ;
#24581 = DIRECTION ( 'NONE',  ( -0.000000000000000000, -1.000000000000000000, -0.000000000000000000 ) ) ;
#24582 = DIRECTION ( 'NONE',  ( 0.000000000000000000, 0.000000000000000000, 1.000000000000000000 ) ) ;
#24583 = AXIS2_PLACEMENT_3D ( 'NONE', #92108, #62673, #24034 ) ;
#24584 = EDGE_CURVE ( 'NONE', #76293, #70678, #50756, .T. ) ;
#24585 = ADVANCED_FACE ( 'NONE', ( #105714 ), #27756, .T. ) ;
#24586 = ADVANCED_FACE ( 'NONE', ( #6827 ), #115569, .T. ) ;
#24587 = AXIS2_PLACEMENT_3D ( 'NONE', #35309, #96772, #126903 ) ;
#24588 = EDGE_CURVE ( 'NONE', #75028, #110459, #73717, .T. ) ;
#24589 = ORIENTED_EDGE ( 'NONE', *, *, #81077, .T. ) ;
#24590 = AXIS2_PLACEMENT_3D ( 'NONE', #99310, #57451, #58740 ) ;
#24591 = DIRECTION ( 'NONE',  ( 0.000000000000000000, 0.000000000000000000, 1.000000000000000000 ) ) ;
#24592 = CONICAL_SURFACE ( 'NONE', #55888, 0.09999999999999999167, 0.003490658503988666988 ) ;
#24593 = ORIENTED_EDGE ( 'NONE', *, *, #98876, .F. ) ;
#24594 = ORIENTED_EDGE ( 'NONE', *, *, #127627, .T. ) ;
#24595 = DIRECTION ( 'NONE',  ( 0.000000000000000000, 0.000000000000000000, 1.000000000000000000 ) ) ;
#24596 = EDGE_CURVE ( 'NONE', #12708, #63537, #29827, .T. ) ;
#24597 = EDGE_CURVE ( 'NONE', #63648, #90185, #2711, .T. ) ;
#24598 = CIRCLE ( 'NONE', #83196, 0.1000000000000000056 ) ;
#24599 = ORIENTED_EDGE ( 'NONE', *, *, #63284, .T. ) ;
#24600 = CARTESIAN_POINT ( 'NONE',  ( 3.749999999999944045, 2.500000000000000000, -2.757883832488654097 ) ) ;
#24601 = CARTESIAN_POINT ( 'NONE',  ( -14.14999999999998614, 12.50000000000000000, 2.165063509461101265 ) ) ;
#24602 = AXIS2_PLACEMENT_3D ( 'NONE', #12726, #120769, #111591 ) ;
#24603 = CARTESIAN_POINT ( 'NONE',  ( 8.749999999999923617, 2.500000000000000000, 1.472243186433545459 ) ) ;
#24604 = ORIENTED_EDGE ( 'NONE', *, *, #83070, .T. ) ;
#24605 = ADVANCED_FACE ( 'NONE', ( #84778 ), #86710, .T. ) ;
#24606 = CIRCLE ( 'NONE', #106181, 0.06509327318403745899 ) ;
#24608 = EDGE_CURVE ( 'NONE', #46684, #99945, #56987, .T. ) ;
#24607 = FACE_BOUND ( 'NONE', #121572, .T. ) ;
#24609 = DIRECTION ( 'NONE',  ( -0.000000000000000000, 1.000000000000000000, -0.000000000000000000 ) ) ;
#24611 = ORIENTED_EDGE ( 'NONE', *, *, #25468, .T. ) ;
#24610 = CARTESIAN_POINT ( 'NONE',  ( -5.600000000000020073, 2.500000000000000000, 0.3464101615137736845 ) ) ;
#24612 = CARTESIAN_POINT ( 'NONE',  ( 12.09999999999990550, 2.500000000000000000, -3.537306695894649966 ) ) ;
#24613 = AXIS2_PLACEMENT_3D ( 'NONE', #87456, #89408, #69114 ) ;
#24614 = EDGE_CURVE ( 'NONE', #59573, #11927, #106973, .T. ) ;
#24615 = LINE ( 'NONE', #46180, #96919 ) ;
#24616 = EDGE_CURVE ( 'NONE', #114539, #97064, #24568, .T. ) ;
#24617 = EDGE_LOOP ( 'NONE', ( #103878, #78783 ) ) ;
#24619 = AXIS2_PLACEMENT_3D ( 'NONE', #115361, #87850, #65644 ) ;
#24618 = AXIS2_PLACEMENT_3D ( 'NONE', #75401, #125162, #44672 ) ;
#24620 = VERTEX_POINT ( 'NONE', #7494 ) ;
#24621 = ORIENTED_EDGE ( 'NONE', *, *, #123740, .F. ) ;
#24622 = CARTESIAN_POINT ( 'NONE',  ( 5.849999999999931255, 2.500000000000000000, 2.957883832488649389 ) ) ;
#24623 = DIRECTION ( 'NONE',  ( 0.000000000000000000, 1.000000000000000000, 0.000000000000000000 ) ) ;
#24624 = CARTESIAN_POINT ( 'NONE',  ( -8.350000000000013856, 12.50000000000000000, -2.165063509461101710 ) ) ;
#24625 = APPLICATION_CONTEXT ( 'automotive_design' ) ;
#24626 = FACE_BOUND ( 'NONE', #30164, .T. ) ;
#24627 = ORIENTED_EDGE ( 'NONE', *, *, #109900, .T. ) ;
#24628 = CARTESIAN_POINT ( 'NONE',  ( 185.5260416670080588, -6.551208109652273848, -3.782341765625003571 ) ) ;
#24629 = LINE ( 'NONE', #124757, #107614 ) ;
#24630 = CARTESIAN_POINT ( 'NONE',  ( 3.949999999999939782, 2.500000000000000000, 2.611473670974873151 ) ) ;
#24631 = FACE_OUTER_BOUND ( 'NONE', #36603, .T. ) ;
#24632 = DIRECTION ( 'NONE',  ( 0.000000000000000000, 1.000000000000000000, 0.000000000000000000 ) ) ;
#24633 = DIRECTION ( 'NONE',  ( -0.000000000000000000, 1.000000000000000000, -0.000000000000000000 ) ) ;
#24634 = DIRECTION ( 'NONE',  ( 0.000000000000000000, 1.000000000000000000, 0.000000000000000000 ) ) ;
#24635 = DIRECTION ( 'NONE',  ( -4.274815082592931898E-19, -0.9999939076577903929, -0.003490651415223739937 ) ) ;
#24636 = ORIENTED_EDGE ( 'NONE', *, *, #87502, .F. ) ;
#24637 = ORIENTED_EDGE ( 'NONE', *, *, #40412, .F. ) ;
#24638 = ORIENTED_EDGE ( 'NONE', *, *, #103761, .F. ) ;
#24639 = ORIENTED_EDGE ( 'NONE', *, *, #84587, .T. ) ;
#24640 = ORIENTED_EDGE ( 'NONE', *, *, #114393, .F. ) ;
#24641 = FACE_OUTER_BOUND ( 'NONE', #52815, .T. ) ;
#24642 = VECTOR ( 'NONE', #5645, 1000.000000000000000 ) ;
#24643 = FACE_OUTER_BOUND ( 'NONE', #67835, .T. ) ;
#24644 = ORIENTED_EDGE ( 'NONE', *, *, #124658, .T. ) ;
#24645 = FACE_BOUND ( 'NONE', #33787, .T. ) ;
#24646 = DIRECTION ( 'NONE',  ( 0.000000000000000000, 1.000000000000000000, 0.000000000000000000 ) ) ;
#24647 = AXIS2_PLACEMENT_3D ( 'NONE', #102296, #61738, #11328 ) ;
#24648 = EDGE_CURVE ( 'NONE', #4060, #114896, #94582, .T. ) ;
#24649 = AXIS2_PLACEMENT_3D ( 'NONE', #100886, #121183, #72735 ) ;
#24650 = DIRECTION ( 'NONE',  ( 0.000000000000000000, 0.000000000000000000, 1.000000000000000000 ) ) ;
#24651 = EDGE_CURVE ( 'NONE', #83875, #40839, #48709, .T. ) ;
#24652 = EDGE_LOOP ( 'NONE', ( #73723, #113327, #32998, #111449 ) ) ;
#24653 = LINE ( 'NONE', #64564, #70392 ) ;
#24654 = CARTESIAN_POINT ( 'NONE',  ( 1.899999999999951283, 12.50000000000000000, -4.611443907251939756 ) ) ;
#24655 = CARTESIAN_POINT ( 'NONE',  ( -5.400000000000020783, 2.500000000000000000, 0.6928203230275494784 ) ) ;
#24656 = EDGE_LOOP ( 'NONE', ( #7069, #128520, #10153, #100922 ) ) ;
#24657 = CARTESIAN_POINT ( 'NONE',  ( -5.650000000000019895, 2.500000000000000000, 1.818653347947321475 ) ) ;
#24658 = AXIS2_PLACEMENT_3D ( 'NONE', #92976, #42597, #72687 ) ;
#24659 = EDGE_LOOP ( 'NONE', ( #50292, #32300, #71696, #12808 ) ) ;
#24660 = AXIS2_PLACEMENT_3D ( 'NONE', #82503, #72036, #91661 ) ;
#24661 = AXIS2_PLACEMENT_3D ( 'NONE', #92444, #49972, #89862 ) ;
#24662 = EDGE_LOOP ( 'NONE', ( #96735, #17541 ) ) ;
#24663 = EDGE_LOOP ( 'NONE', ( #80809, #18932, #64886, #119370 ) ) ;
#24664 = DIRECTION ( 'NONE',  ( 0.000000000000000000, 0.000000000000000000, 1.000000000000000000 ) ) ;
#24665 = FACE_OUTER_BOUND ( 'NONE', #60746, .T. ) ;
#24666 = FACE_OUTER_BOUND ( 'NONE', #118865, .T. ) ;
#24667 = ORIENTED_EDGE ( 'NONE', *, *, #26714, .F. ) ;
#24668 = CARTESIAN_POINT ( 'NONE',  ( 13.54999999999989768, 12.50000000000000000, -2.511473670974877948 ) ) ;
#24669 = CIRCLE ( 'NONE', #108284, 0.06509327318403745899 ) ;
#24670 = CARTESIAN_POINT ( 'NONE',  ( 2.499999999999983569, 12.50000000000000000, 0.06509327318403515528 ) ) ;
#24671 = CARTESIAN_POINT ( 'NONE',  ( 0.1999999999999571565, 12.50000000000000000, 3.983716857408420076 ) ) ;
#24672 = PLANE ( 'NONE',  #24583 ) ;
#24674 = EDGE_LOOP ( 'NONE', ( #111034, #20408 ) ) ;
#24673 = DIRECTION ( 'NONE',  ( -0.000000000000000000, 1.000000000000000000, -0.000000000000000000 ) ) ;
#24675 = CIRCLE ( 'NONE', #85298, 0.06509327318403745899 ) ;
#24676 = CARTESIAN_POINT ( 'NONE',  ( -2.900000000000029221, 2.500000000000000000, -2.276824562219559311E-15 ) ) ;
#24677 = ORIENTED_EDGE ( 'NONE', *, *, #6084, .F. ) ;
#24678 = CARTESIAN_POINT ( 'NONE',  ( -14.39999999999998614, 2.500000000000000000, -0.3464101615137760715 ) ) ;
#24679 = AXIS2_PLACEMENT_3D ( 'NONE', #42667, #76463, #83222 ) ;
#24680 = ORIENTED_EDGE ( 'NONE', *, *, #77501, .T. ) ;
#24681 = ORIENTED_EDGE ( 'NONE', *, *, #80, .F. ) ;
#24682 = DIRECTION ( 'NONE',  ( 0.000000000000000000, 0.000000000000000000, 1.000000000000000000 ) ) ;
#24683 = PRESENTATION_LAYER_ASSIGNMENT (  '', '', ( #47672 ) ) ;
#24684 = FACE_OUTER_BOUND ( 'NONE', #81245, .T. ) ;
#24685 = CARTESIAN_POINT ( 'NONE',  ( -11.25000000000000178, 12.50000000000000000, -1.472243186433546125 ) ) ;
#24686 = LINE ( 'NONE', #77003, #105220 ) ;
#24688 = CIRCLE ( 'NONE', #97829, 0.06509327318403745899 ) ;
#24687 = DIRECTION ( 'NONE',  ( -0.000000000000000000, -1.000000000000000000, -0.000000000000000000 ) ) ;
#24689 = ORIENTED_EDGE ( 'NONE', *, *, #104676, .F. ) ;
#24690 = AXIS2_PLACEMENT_3D ( 'NONE', #90352, #89088, #80561 ) ;
#24691 = ORIENTED_EDGE ( 'NONE', *, *, #86521, .T. ) ;
#24692 = ADVANCED_FACE ( 'NONE', ( #30392 ), #111365, .T. ) ;
#24693 = DIRECTION ( 'NONE',  ( 0.000000000000000000, 0.000000000000000000, 1.000000000000000000 ) ) ;
#24694 = AXIS2_PLACEMENT_3D ( 'NONE', #83364, #24435, #55825 ) ;
#24695 = CARTESIAN_POINT ( 'NONE',  ( -4.150000000000025224, 12.50000000000000000, 5.867463478539781896 ) ) ;
#24696 = DIRECTION ( 'NONE',  ( 0.000000000000000000, 0.000000000000000000, 1.000000000000000000 ) ) ;
#24697 = ORIENTED_EDGE ( 'NONE', *, *, #119429, .F. ) ;
#24698 = EDGE_LOOP ( 'NONE', ( #110186, #118650 ) ) ;
#24699 = DIRECTION ( 'NONE',  ( 0.000000000000000000, -0.000000000000000000, 1.000000000000000000 ) ) ;
#24700 = AXIS2_PLACEMENT_3D ( 'NONE', #124482, #47213, #125125 ) ;
#24701 = VERTEX_POINT ( 'NONE', #77526 ) ;
#24702 = FACE_OUTER_BOUND ( 'NONE', #108157, .T. ) ;
#24703 = DIRECTION ( 'NONE',  ( 0.000000000000000000, 0.000000000000000000, 1.000000000000000000 ) ) ;
#24704 = VERTEX_POINT ( 'NONE', #10698 ) ;
#24705 = DIRECTION ( 'NONE',  ( 0.000000000000000000, -0.000000000000000000, 1.000000000000000000 ) ) ;
#24706 = DIRECTION ( 'NONE',  ( 0.000000000000000000, 0.000000000000000000, 1.000000000000000000 ) ) ;
#24707 = LINE ( 'NONE', #6963, #5022 ) ;
#24708 = EDGE_CURVE ( 'NONE', #55428, #2826, #4756, .T. ) ;
#24709 = VECTOR ( 'NONE', #71466, 1000.000000000000000 ) ;
#24710 = EDGE_CURVE ( 'NONE', #107893, #4124, #108907, .T. ) ;
#24711 = CARTESIAN_POINT ( 'NONE',  ( 6.049999999999932321, 2.500000000000000000, 1.918653347947321564 ) ) ;
#24712 = ORIENTED_EDGE ( 'NONE', *, *, #51328, .F. ) ;
#24713 = CARTESIAN_POINT ( 'NONE',  ( -0.6000000000000383915, 2.500000000000000000, -4.676537180435977881 ) ) ;
#24714 = VECTOR ( 'NONE', #14854, 1000.000000000000000 ) ;
#24715 = CARTESIAN_POINT ( 'NONE',  ( 11.84999999999990372, 2.500000000000000000, 1.718653347947321386 ) ) ;
#24716 = ORIENTED_EDGE ( 'NONE', *, *, #27200, .T. ) ;
#24717 = ORIENTED_EDGE ( 'NONE', *, *, #9948, .T. ) ;
#24718 = ADVANCED_FACE ( 'NONE', ( #127921 ), #75877, .T. ) ;
#24719 = CARTESIAN_POINT ( 'NONE',  ( 185.3802083336747160, 4.367472073101515306, 7.564683531250000925 ) ) ;
#24720 = PLANE ( 'NONE',  #122233 ) ;
#24721 = CARTESIAN_POINT ( 'NONE',  ( 3.349999999999945466, 2.500000000000000000, -2.857883832488653741 ) ) ;
#24722 = DIRECTION ( 'NONE',  ( 0.000000000000000000, 0.000000000000000000, 1.000000000000000000 ) ) ;
#24723 = DIRECTION ( 'NONE',  ( 0.000000000000000000, -0.9999939076577903929, 0.003490651415223739937 ) ) ;
#24724 = CARTESIAN_POINT ( 'NONE',  ( -10.60000000000000320, 2.500000000000000000, -3.883716857408422207 ) ) ;
#24725 = CARTESIAN_POINT ( 'NONE',  ( -14.19999999999998685, 2.500000000000000000, -0.1000000000000001166 ) ) ;
#24726 = CARTESIAN_POINT ( 'NONE',  ( 11.64999999999990798, 12.50000000000000000, -1.472243186433550122 ) ) ;
#24727 = FACE_OUTER_BOUND ( 'NONE', #51275, .T. ) ;
#24728 = CARTESIAN_POINT ( 'NONE',  ( -9.550000000000007816, 12.50000000000000000, -6.495190528383297135 ) ) ;
#24729 = EDGE_LOOP ( 'NONE', ( #43614, #15304, #2163, #89077 ) ) ;
#24730 = ORIENTED_EDGE ( 'NONE', *, *, #93730, .T. ) ;
#24731 = EDGE_LOOP ( 'NONE', ( #112021, #100565 ) ) ;
#24732 = AXIS2_PLACEMENT_3D ( 'NONE', #12421, #69409, #92269 ) ;
#24733 = AXIS2_PLACEMENT_3D ( 'NONE', #10361, #77800, #78484 ) ;
#24734 = EDGE_LOOP ( 'NONE', ( #95651, #55399 ) ) ;
#24735 = CARTESIAN_POINT ( 'NONE',  ( -14.14999999999998614, 2.500000000000000000, -2.857883832488651521 ) ) ;
#24736 = DIRECTION ( 'NONE',  ( 0.000000000000000000, 1.000000000000000000, 0.000000000000000000 ) ) ;
#24737 = FACE_OUTER_BOUND ( 'NONE', #21578, .T. ) ;
#24738 = EDGE_LOOP ( 'NONE', ( #82328, #1885, #88731, #34845 ) ) ;
#24739 = VECTOR ( 'NONE', #60301, 1000.000000000000000 ) ;
#24740 = PLANE ( 'NONE',  #29921 ) ;
#24741 = EDGE_CURVE ( 'NONE', #37904, #74337, #59177, .T. ) ;
#24742 = CIRCLE ( 'NONE', #33160, 0.1000000000000002554 ) ;
#24743 = FACE_OUTER_BOUND ( 'NONE', #64967, .T. ) ;
#24745 = ORIENTED_EDGE ( 'NONE', *, *, #84572, .T. ) ;
#24744 = DIRECTION ( 'NONE',  ( 0.000000000000000000, 0.000000000000000000, 1.000000000000000000 ) ) ;
#24746 = ADVANCED_FACE ( 'NONE', ( #28445 ), #6894, .T. ) ;
#24747 = DIRECTION ( 'NONE',  ( 0.000000000000000000, 0.000000000000000000, 1.000000000000000000 ) ) ;
#24749 = EDGE_CURVE ( 'NONE', #70878, #48804, #29720, .T. ) ;
#24748 = AXIS2_PLACEMENT_3D ( 'NONE', #34617, #114430, #24780 ) ;
#24750 = FACE_OUTER_BOUND ( 'NONE', #20433, .T. ) ;
#24751 = ORIENTED_EDGE ( 'NONE', *, *, #105190, .F. ) ;
#24752 = CONICAL_SURFACE ( 'NONE', #118742, 0.1000000000000002554, 0.003490658503988666988 ) ;
#24753 = VERTEX_POINT ( 'NONE', #90570 ) ;
#24754 = ORIENTED_EDGE ( 'NONE', *, *, #30858, .T. ) ;
#24755 = VERTEX_POINT ( 'NONE', #88645 ) ;
#24756 = DIRECTION ( 'NONE',  ( 0.000000000000000000, 0.000000000000000000, 1.000000000000000000 ) ) ;
#24757 = ADVANCED_FACE ( 'NONE', ( #69646 ), #37623, .T. ) ;
#24758 = EDGE_CURVE ( 'NONE', #117106, #80059, #90296, .T. ) ;
#24759 = EDGE_CURVE ( 'NONE', #90702, #17926, #103072, .T. ) ;
#24760 = ADVANCED_FACE ( 'NONE', ( #59861 ), #52992, .T. ) ;
#24761 = CARTESIAN_POINT ( 'NONE',  ( -7.050000000000016698, 2.500000000000000000, -2.065063509461102065 ) ) ;
#24762 = FACE_OUTER_BOUND ( 'NONE', #81524, .T. ) ;
#24763 = DIRECTION ( 'NONE',  ( 0.000000000000000000, 0.000000000000000000, 1.000000000000000000 ) ) ;
#24764 = AXIS2_PLACEMENT_3D ( 'NONE', #3881, #62817, #2577 ) ;
#24765 = VERTEX_POINT ( 'NONE', #107645 ) ;
#24766 = EDGE_CURVE ( 'NONE', #102282, #108236, #8770, .T. ) ;
#24767 = CARTESIAN_POINT ( 'NONE',  ( -7.100000000000013856, 2.500000000000000000, 4.922947341949748257 ) ) ;
#24768 = ORIENTED_EDGE ( 'NONE', *, *, #56075, .T. ) ;
#24769 = AXIS2_PLACEMENT_3D ( 'NONE', #122614, #50643, #40853 ) ;
#24770 = DIRECTION ( 'NONE',  ( 0.000000000000000000, 0.000000000000000000, 1.000000000000000000 ) ) ;
#24771 = FACE_OUTER_BOUND ( 'NONE', #77137, .T. ) ;
#24772 = CARTESIAN_POINT ( 'NONE',  ( -14.79999999999998295, 2.500000000000000000, -0.3464101615137760715 ) ) ;
#24773 = CARTESIAN_POINT ( 'NONE',  ( 17.17539648375908712, -2.541523116374657221, 5.507477068181874102 ) ) ;
#24774 = EDGE_CURVE ( 'NONE', #113894, #111448, #80096, .T. ) ;
#24775 = ORIENTED_EDGE ( 'NONE', *, *, #4004, .T. ) ;
#24776 = CIRCLE ( 'NONE', #28982, 0.09999999999999999167 ) ;
#24777 = EDGE_LOOP ( 'NONE', ( #41894, #116576, #78659, #50920 ) ) ;
#24778 = VERTEX_POINT ( 'NONE', #40195 ) ;
#24779 = CARTESIAN_POINT ( 'NONE',  ( 4.349999999999937472, 12.50000000000000000, 6.776507416713035248 ) ) ;
#24780 = DIRECTION ( 'NONE',  ( 0.000000000000000000, 0.000000000000000000, 1.000000000000000000 ) ) ;
#24781 = CARTESIAN_POINT ( 'NONE',  ( 7.099999999999927702, 2.500000000000000000, 5.022947341949748790 ) ) ;
#24782 = FACE_BOUND ( 'NONE', #81804, .T. ) ;
#24783 = CARTESIAN_POINT ( 'NONE',  ( -8.150000000000014566, 2.500000000000000000, -6.941600689897073906 ) ) ;
#24784 = CARTESIAN_POINT ( 'NONE',  ( 7.899999999999924860, 2.500000000000000000, 3.637306695894644726 ) ) ;
#24785 = CARTESIAN_POINT ( 'NONE',  ( -9.550000000000002487, 2.500000000000000000, 6.595190528383296780 ) ) ;
#24786 = CIRCLE ( 'NONE', #12241, 0.06509327318403745899 ) ;
#24787 = CARTESIAN_POINT ( 'NONE',  ( 186.7135416670080872, 4.367472073101518859, -7.564683531249999149 ) ) ;
#24788 = DIRECTION ( 'NONE',  ( 0.000000000000000000, 0.000000000000000000, 1.000000000000000000 ) ) ;
#24789 = VECTOR ( 'NONE', #6586, 1000.000000000000000 ) ;
#24790 = DIRECTION ( 'NONE',  ( 0.000000000000000000, 0.000000000000000000, -1.000000000000000000 ) ) ;
#24791 = VERTEX_POINT ( 'NONE', #110222 ) ;
#24792 = CARTESIAN_POINT ( 'NONE',  ( -1.850000000000033396, 2.500000000000000000, -6.148780366869526226 ) ) ;
#24793 = ORIENTED_EDGE ( 'NONE', *, *, #10662, .T. ) ;
#24794 = ORIENTED_EDGE ( 'NONE', *, *, #22528, .F. ) ;
#24795 = EDGE_LOOP ( 'NONE', ( #15501, #57796, #76443, #1240 ) ) ;
#24796 = ORIENTED_EDGE ( 'NONE', *, *, #22410, .T. ) ;
#24797 = CONICAL_SURFACE ( 'NONE', #18527, 0.1000000000000002554, 0.003490658503988666988 ) ;
#24798 = FACE_OUTER_BOUND ( 'NONE', #6584, .T. ) ;
#24799 = FACE_BOUND ( 'NONE', #67251, .T. ) ;
#24800 = DIRECTION ( 'NONE',  ( 0.000000000000000000, 0.000000000000000000, -1.000000000000000000 ) ) ;
#24802 = CIRCLE ( 'NONE', #97954, 0.06509327318403745899 ) ;
#24801 = CIRCLE ( 'NONE', #68703, 7.700000000000000178 ) ;
#24803 = ADVANCED_FACE ( 'NONE', ( #20555 ), #52907, .T. ) ;
#24804 = ORIENTED_EDGE ( 'NONE', *, *, #1118, .T. ) ;
#24805 = CARTESIAN_POINT ( 'NONE',  ( 21.15177371151419194, 2.593223176056360657, 4.151029080743467325 ) ) ;
#24806 = FACE_OUTER_BOUND ( 'NONE', #14436, .T. ) ;
#24807 = EDGE_LOOP ( 'NONE', ( #51738, #103142 ) ) ;
#24808 = DIRECTION ( 'NONE',  ( 0.000000000000000000, 1.000000000000000000, 0.000000000000000000 ) ) ;
#24809 = CARTESIAN_POINT ( 'NONE',  ( 3.349999999999945466, 2.500000000000000000, -7.188010851410854052 ) ) ;
#24810 = EDGE_CURVE ( 'NONE', #107604, #53683, #101016, .T. ) ;
#24811 = ORIENTED_EDGE ( 'NONE', *, *, #116909, .T. ) ;
#24812 = CIRCLE ( 'NONE', #97967, 0.1000000000000002554 ) ;
#24813 = DIRECTION ( 'NONE',  ( 0.000000000000000000, 0.000000000000000000, 1.000000000000000000 ) ) ;
#24814 = PLANE ( 'NONE',  #51739 ) ;
#24815 = ORIENTED_EDGE ( 'NONE', *, *, #100647, .F. ) ;
#24816 = CIRCLE ( 'NONE', #33250, 0.09999999999999982514 ) ;
#24817 = LINE ( 'NONE', #36593, #126224 ) ;
#24818 = AXIS2_PLACEMENT_3D ( 'NONE', #65437, #123698, #64796 ) ;
#24819 = CARTESIAN_POINT ( 'NONE',  ( -12.49999999999999467, 2.500000000000000000, -3.637306695894647390 ) ) ;
#24820 = AXIS2_PLACEMENT_3D ( 'NONE', #22782, #91498, #1820 ) ;
#24821 = DIRECTION ( 'NONE',  ( 0.000000000000000000, -0.9999939076577903929, 0.003490651415223739937 ) ) ;
#24822 = EDGE_LOOP ( 'NONE', ( #121322, #46581 ) ) ;
#24823 = ORIENTED_EDGE ( 'NONE', *, *, #116909, .F. ) ;
#24824 = CARTESIAN_POINT ( 'NONE',  ( 11.89999999999990443, 12.50000000000000000, -0.4115034346978156399 ) ) ;
#24826 = ORIENTED_EDGE ( 'NONE', *, *, #74779, .F. ) ;
#24825 = CIRCLE ( 'NONE', #3887, 0.06509327318403745899 ) ;
#24827 = DIRECTION ( 'NONE',  ( 0.000000000000000000, 0.000000000000000000, 1.000000000000000000 ) ) ;
#24828 = PLANE ( 'NONE',  #99650 ) ;
#24829 = AXIS2_PLACEMENT_3D ( 'NONE', #51604, #41793, #81060 ) ;
#24830 = CIRCLE ( 'NONE', #100147, 0.1000000000000002554 ) ;
#24831 = EDGE_LOOP ( 'NONE', ( #18031, #101729, #52173, #2169 ) ) ;
#24832 = DIRECTION ( 'NONE',  ( -0.000000000000000000, 1.000000000000000000, -0.000000000000000000 ) ) ;
#24833 = CARTESIAN_POINT ( 'NONE',  ( 7.899999999999924860, 2.500000000000000000, 3.637306695894644726 ) ) ;
#24834 = CARTESIAN_POINT ( 'NONE',  ( 2.899999999999945732, 2.500000000000000000, -2.385244779468109755E-15 ) ) ;
#24835 = CARTESIAN_POINT ( 'NONE',  ( 5.199999999999933564, 12.50000000000000000, 0.4115034346978109769 ) ) ;
#24836 = DIRECTION ( 'NONE',  ( -4.274815082592931898E-19, -0.9999939076577903929, -0.003490651415223739937 ) ) ;
#24837 = VECTOR ( 'NONE', #27186, 1000.000000000000000 ) ;
#24838 = VERTEX_POINT ( 'NONE', #61782 ) ;
#24841 = ORIENTED_EDGE ( 'NONE', *, *, #40313, .F. ) ;
#24840 = EDGE_CURVE ( 'NONE', #58497, #119313, #109427, .T. ) ;
#24839 = AXIS2_PLACEMENT_3D ( 'NONE', #77845, #109903, #48397 ) ;
#24842 = DIRECTION ( 'NONE',  ( -0.000000000000000000, -1.000000000000000000, -0.000000000000000000 ) ) ;
#24843 = DIRECTION ( 'NONE',  ( -0.000000000000000000, -1.000000000000000000, -0.000000000000000000 ) ) ;
#24844 = CARTESIAN_POINT ( 'NONE',  ( -11.05000000000000249, 12.50000000000000000, -6.148780366869522673 ) ) ;
#24846 = ORIENTED_EDGE ( 'NONE', *, *, #82123, .F. ) ;
#24845 = EDGE_LOOP ( 'NONE', ( #98785, #70382, #126492, #78589 ) ) ;
#24847 = EDGE_LOOP ( 'NONE', ( #26293, #12203, #62356, #41695 ) ) ;
#24848 = DIRECTION ( 'NONE',  ( -0.000000000000000000, 1.000000000000000000, -0.000000000000000000 ) ) ;
#24851 = EDGE_CURVE ( 'NONE', #102186, #73740, #11370, .T. ) ;
#24850 = DIRECTION ( 'NONE',  ( -4.274815082592931898E-19, -0.9999939076577903929, -0.003490651415223739937 ) ) ;
#24849 = CONICAL_SURFACE ( 'NONE', #127266, 0.1000000000000002554, 0.003490658503988666988 ) ;
#24852 = DIRECTION ( 'NONE',  ( 0.000000000000000000, 0.000000000000000000, -1.000000000000000000 ) ) ;
#24853 = DIRECTION ( 'NONE',  ( 0.000000000000000000, 0.000000000000000000, 1.000000000000000000 ) ) ;
#24854 = DIRECTION ( 'NONE',  ( -0.000000000000000000, -1.000000000000000000, -0.000000000000000000 ) ) ;
#24855 = DIRECTION ( 'NONE',  ( 0.000000000000000000, 0.000000000000000000, 1.000000000000000000 ) ) ;
#24856 = LINE ( 'NONE', #96163, #123858 ) ;
#24857 = DIRECTION ( 'NONE',  ( 0.000000000000000000, -0.000000000000000000, 1.000000000000000000 ) ) ;
#24858 = CARTESIAN_POINT ( 'NONE',  ( 2.099999999999948574, 12.50000000000000000, 4.330127018922196314 ) ) ;
#24859 = EDGE_CURVE ( 'NONE', #128359, #41239, #115674, .T. ) ;
#24860 = EDGE_CURVE ( 'NONE', #64737, #11527, #121321, .T. ) ;
#24861 = FACE_OUTER_BOUND ( 'NONE', #88022, .T. ) ;
#24862 = VERTEX_POINT ( 'NONE', #43436 ) ;
#24863 = CONICAL_SURFACE ( 'NONE', #28790, 0.1000000000000000472, 0.003490658503988666988 ) ;
#24864 = EDGE_CURVE ( 'NONE', #113778, #52806, #11111, .T. ) ;
#24865 = DIRECTION ( 'NONE',  ( 0.000000000000000000, -0.9999939076577903929, 0.003490651415223739937 ) ) ;
#24866 = ORIENTED_EDGE ( 'NONE', *, *, #103669, .T. ) ;
#24867 = ORIENTED_EDGE ( 'NONE', *, *, #83503, .T. ) ;
#24868 = EDGE_CURVE ( 'NONE', #80261, #22096, #90548, .T. ) ;
#24869 = DIRECTION ( 'NONE',  ( 0.000000000000000000, 1.000000000000000000, 0.000000000000000000 ) ) ;
#24870 = CARTESIAN_POINT ( 'NONE',  ( -6.850000000000013856, 12.50000000000000000, 6.906693963081109722 ) ) ;
#24871 = AXIS2_PLACEMENT_3D ( 'NONE', #53361, #93278, #72993 ) ;
#24872 = DIRECTION ( 'NONE',  ( 0.000000000000000000, 0.000000000000000000, 1.000000000000000000 ) ) ;
#24874 = AXIS2_PLACEMENT_3D ( 'NONE', #126347, #56930, #96870 ) ;
#24873 = CARTESIAN_POINT ( 'NONE',  ( 5.649999999999934630, 12.50000000000000000, -1.883746621131363375 ) ) ;
#24875 = LINE ( 'NONE', #54969, #15108 ) ;
#24876 = CARTESIAN_POINT ( 'NONE',  ( -6.450000000000019718, 2.500000000000000000, -6.048780366869526581 ) ) ;
#24877 = DIRECTION ( 'NONE',  ( 0.000000000000000000, 1.000000000000000000, 0.000000000000000000 ) ) ;
#24878 = EDGE_LOOP ( 'NONE', ( #116786, #47663 ) ) ;
#24879 = FACE_OUTER_BOUND ( 'NONE', #67007, .T. ) ;
#24880 = AXIS2_PLACEMENT_3D ( 'NONE', #14032, #53344, #53979 ) ;
#24881 = DIRECTION ( 'NONE',  ( -4.274815082592931898E-19, -0.9999939076577903929, -0.003490651415223739937 ) ) ;
#24882 = VERTEX_POINT ( 'NONE', #51955 ) ;
#24883 = ORIENTED_EDGE ( 'NONE', *, *, #26654, .T. ) ;
#24884 = AXIS2_PLACEMENT_3D ( 'NONE', #95, #59698, #99603 ) ;
#24885 = ORIENTED_EDGE ( 'NONE', *, *, #114279, .T. ) ;
#24886 = CIRCLE ( 'NONE', #108502, 0.1000000000000002554 ) ;
#24887 = EDGE_LOOP ( 'NONE', ( #116915, #73786, #25533, #129098 ) ) ;
#24888 = DIRECTION ( 'NONE',  ( 0.000000000000000000, 0.000000000000000000, -1.000000000000000000 ) ) ;
#24889 = CARTESIAN_POINT ( 'NONE',  ( 8.549999999999918998, 2.500000000000000000, 6.841600689897072485 ) ) ;
#24890 = VECTOR ( 'NONE', #110517, 1000.000000000000000 ) ;
#24891 = CARTESIAN_POINT ( 'NONE',  ( 108.0000000000000142, 9.000000000000001776, -0.2500000000000000000 ) ) ;
#24892 = DIRECTION ( 'NONE',  ( 0.000000000000000000, -0.000000000000000000, 1.000000000000000000 ) ) ;
#24893 = DIRECTION ( 'NONE',  ( 0.000000000000000000, 0.000000000000000000, -1.000000000000000000 ) ) ;
#24894 = ORIENTED_EDGE ( 'NONE', *, *, #50899, .T. ) ;
#24895 = FACE_OUTER_BOUND ( 'NONE', #74620, .T. ) ;
#24896 = CARTESIAN_POINT ( 'NONE',  ( -6.250000000000017764, 2.500000000000000000, 7.188010851410848723 ) ) ;
#24897 = EDGE_CURVE ( 'NONE', #80982, #48968, #102845, .T. ) ;
#24898 = CARTESIAN_POINT ( 'NONE',  ( 7.899999999999924860, 2.500000000000000000, 5.022947341949748790 ) ) ;
#24899 = ORIENTED_EDGE ( 'NONE', *, *, #25916, .T. ) ;
#24900 = ORIENTED_EDGE ( 'NONE', *, *, #69043, .F. ) ;
#24901 = ORIENTED_EDGE ( 'NONE', *, *, #106160, .T. ) ;
#24902 = EDGE_CURVE ( 'NONE', #85816, #108779, #31660, .T. ) ;
#24903 = AXIS2_PLACEMENT_3D ( 'NONE', #91945, #81483, #103040 ) ;
#24904 = PLANE ( 'NONE',  #21593 ) ;
#24905 = ADVANCED_FACE ( 'NONE', ( #122622 ), #111477, .T. ) ;
#24906 = EDGE_CURVE ( 'NONE', #108234, #91772, #78031, .T. ) ;
#24907 = ADVANCED_FACE ( 'NONE', ( #12645 ), #73826, .T. ) ;
#24908 = LINE ( 'NONE', #8314, #15355 ) ;
#24909 = DIRECTION ( 'NONE',  ( 0.000000000000000000, -0.000000000000000000, 1.000000000000000000 ) ) ;
#24910 = AXIS2_PLACEMENT_3D ( 'NONE', #101380, #63385, #92184 ) ;
#24911 = CONICAL_SURFACE ( 'NONE', #10244, 0.1000000000000000056, 0.003490658503988666988 ) ;
#24912 = ADVANCED_FACE ( 'NONE', ( #92501 ), #94752, .T. ) ;
#24913 = EDGE_LOOP ( 'NONE', ( #4429, #129596 ) ) ;
#24914 = DIRECTION ( 'NONE',  ( 0.000000000000000000, 1.000000000000000000, 0.000000000000000000 ) ) ;
#24915 = DIRECTION ( 'NONE',  ( 0.000000000000000000, 0.000000000000000000, -1.000000000000000000 ) ) ;
#24916 = DIRECTION ( 'NONE',  ( 0.000000000000000000, -0.9999939076577903929, 0.003490651415223739937 ) ) ;
#24917 = DIRECTION ( 'NONE',  ( -4.274815082592931898E-19, -0.9999939076577903929, -0.003490651415223739937 ) ) ;
#24918 = DIRECTION ( 'NONE',  ( -0.000000000000000000, -1.000000000000000000, -0.000000000000000000 ) ) ;
#24919 = CONICAL_SURFACE ( 'NONE', #129413, 0.1000000000000002554, 0.003490658503988666988 ) ;
#24921 = EDGE_CURVE ( 'NONE', #99497, #25372, #98961, .T. ) ;
#24920 = AXIS2_PLACEMENT_3D ( 'NONE', #26005, #67170, #126122 ) ;
#24922 = ORIENTED_EDGE ( 'NONE', *, *, #99659, .T. ) ;
#24923 = CONICAL_SURFACE ( 'NONE', #52121, 0.1000000000000000472, 0.003490658503988666988 ) ;
#24924 = EDGE_CURVE ( 'NONE', #51310, #63382, #41507, .T. ) ;
#24925 = CARTESIAN_POINT ( 'NONE',  ( -4.200000000000029488, 2.500000000000000000, -4.230127018922201998 ) ) ;
#24926 = ORIENTED_EDGE ( 'NONE', *, *, #877, .T. ) ;
#24927 = ORIENTED_EDGE ( 'NONE', *, *, #124751, .F. ) ;
#24928 = DIRECTION ( 'NONE',  ( 0.000000000000000000, 1.000000000000000000, 0.000000000000000000 ) ) ;
#24929 = FACE_BOUND ( 'NONE', #26755, .T. ) ;
#24930 = VECTOR ( 'NONE', #55847, 1000.000000000000000 ) ;
#24931 = DIRECTION ( 'NONE',  ( 0.000000000000000000, 1.000000000000000000, 0.000000000000000000 ) ) ;
#24932 = CARTESIAN_POINT ( 'NONE',  ( 0.7999999999999548583, 2.500000000000000000, 4.330127018922196314 ) ) ;
#24933 = CARTESIAN_POINT ( 'NONE',  ( -5.200000000000025935, 2.500000000000000000, -4.083716857408426826 ) ) ;
#24934 = ORIENTED_EDGE ( 'NONE', *, *, #45714, .F. ) ;
#24935 = EDGE_LOOP ( 'NONE', ( #2842, #69067, #52546, #46170 ) ) ;
#24936 = FACE_OUTER_BOUND ( 'NONE', #76370, .T. ) ;
#24937 = LINE ( 'NONE', #76616, #28064 ) ;
#24938 = DIRECTION ( 'NONE',  ( 0.000000000000000000, 0.000000000000000000, 1.000000000000000000 ) ) ;
#24939 = DIRECTION ( 'NONE',  ( -0.000000000000000000, 1.000000000000000000, -0.000000000000000000 ) ) ;
#24940 = EDGE_LOOP ( 'NONE', ( #18182, #47348 ) ) ;
#24941 = CARTESIAN_POINT ( 'NONE',  ( -5.850000000000021849, 2.500000000000000000, -2.857883832488653741 ) ) ;
#24942 = LINE ( 'NONE', #4626, #114356 ) ;
#24943 = CONICAL_SURFACE ( 'NONE', #100164, 0.09999999999999982514, 0.003490658503988666988 ) ;
#24944 = ORIENTED_EDGE ( 'NONE', *, *, #93468, .F. ) ;
#24945 = DIRECTION ( 'NONE',  ( 0.000000000000000000, 0.000000000000000000, -1.000000000000000000 ) ) ;
#24946 = ORIENTED_EDGE ( 'NONE', *, *, #122494, .F. ) ;
#24947 = FACE_BOUND ( 'NONE', #55866, .T. ) ;
#24948 = CARTESIAN_POINT ( 'NONE',  ( -10.40000000000000213, 12.50000000000000000, 0.6928203230275494784 ) ) ;
#24949 = ORIENTED_EDGE ( 'NONE', *, *, #11331, .F. ) ;
#24950 = FACE_OUTER_BOUND ( 'NONE', #22004, .T. ) ;
#24951 = DIRECTION ( 'NONE',  ( -0.000000000000000000, -1.000000000000000000, -0.000000000000000000 ) ) ;
#24952 = EDGE_LOOP ( 'NONE', ( #120724, #68847, #69875, #91408 ) ) ;
#24953 = ORIENTED_EDGE ( 'NONE', *, *, #48535, .F. ) ;
#24954 = CARTESIAN_POINT ( 'NONE',  ( 185.3385416670080872, 6.551208109652274736, 3.782341765625001351 ) ) ;
#24955 = CONICAL_SURFACE ( 'NONE', #18692, 0.1000000000000000056, 0.003490658503988666988 ) ;
#24956 = DIRECTION ( 'NONE',  ( -0.000000000000000000, 1.000000000000000000, -0.000000000000000000 ) ) ;
#24957 = DIRECTION ( 'NONE',  ( -0.000000000000000000, 1.000000000000000000, -0.000000000000000000 ) ) ;
#24958 = ADVANCED_FACE ( 'NONE', ( #93221 ), #29922, .T. ) ;
#24959 = DIRECTION ( 'NONE',  ( -0.000000000000000000, 1.000000000000000000, -0.000000000000000000 ) ) ;
#24960 = CARTESIAN_POINT ( 'NONE',  ( 4.999999999999936939, 2.500000000000000000, -0.7928203230275542301 ) ) ;
#24961 = CARTESIAN_POINT ( 'NONE',  ( 1.249999999999953815, 12.50000000000000000, -2.922977105672691422 ) ) ;
#24962 = DIRECTION ( 'NONE',  ( 0.000000000000000000, 0.000000000000000000, 1.000000000000000000 ) ) ;
#24963 = VECTOR ( 'NONE', #84402, 1000.000000000000000 ) ;
#24964 = ORIENTED_EDGE ( 'NONE', *, *, #76440, .T. ) ;
#24965 = ORIENTED_EDGE ( 'NONE', *, *, #14966, .F. ) ;
#24966 = DIRECTION ( 'NONE',  ( 0.000000000000000000, 0.000000000000000000, -1.000000000000000000 ) ) ;
#24968 = CONICAL_SURFACE ( 'NONE', #22928, 0.1000000000000000472, 0.003490658503988666988 ) ;
#24967 = AXIS2_PLACEMENT_3D ( 'NONE', #73340, #36509, #59379 ) ;
#24969 = PLANE ( 'NONE',  #95686 ) ;
#24970 = CARTESIAN_POINT ( 'NONE',  ( -6.450000000000016165, 2.500000000000000000, 2.611473670974873151 ) ) ;
#24971 = LINE ( 'NONE', #83263, #53244 ) ;
#24972 = VECTOR ( 'NONE', #48646, 1000.000000000000000 ) ;
#24974 = VERTEX_POINT ( 'NONE', #82100 ) ;
#24973 = ORIENTED_EDGE ( 'NONE', *, *, #64221, .F. ) ;
#24975 = FACE_BOUND ( 'NONE', #20046, .T. ) ;
#24976 = EDGE_LOOP ( 'NONE', ( #85852, #95541, #46748, #54051, #3149, #85174, #50534, #49698 ) ) ;
#24977 = CARTESIAN_POINT ( 'NONE',  ( -0.6500000000000389910, 2.500000000000000000, -6.148780366869526226 ) ) ;
#24978 = DIRECTION ( 'NONE',  ( 0.000000000000000000, 0.000000000000000000, 1.000000000000000000 ) ) ;
#24979 = ORIENTED_EDGE ( 'NONE', *, *, #36333, .F. ) ;
#24980 = DIRECTION ( 'NONE',  ( -0.000000000000000000, -1.000000000000000000, -0.000000000000000000 ) ) ;
#24983 = DIRECTION ( 'NONE',  ( 0.000000000000000000, 0.000000000000000000, 1.000000000000000000 ) ) ;
#24982 = AXIS2_PLACEMENT_3D ( 'NONE', #118130, #28476, #40727 ) ;
#24981 = CONICAL_SURFACE ( 'NONE', #45924, 0.1000000000000002554, 0.003490658503988666988 ) ;
#24984 = DIRECTION ( 'NONE',  ( 0.000000000000000000, 0.000000000000000000, -1.000000000000000000 ) ) ;
#24985 = DIRECTION ( 'NONE',  ( 0.000000000000000000, 1.000000000000000000, 0.000000000000000000 ) ) ;
#24986 = DIRECTION ( 'NONE',  ( 0.000000000000000000, 0.000000000000000000, -1.000000000000000000 ) ) ;
#24987 = FACE_OUTER_BOUND ( 'NONE', #44055, .T. ) ;
#24988 = DIRECTION ( 'NONE',  ( 0.000000000000000000, 1.000000000000000000, 0.000000000000000000 ) ) ;
#24989 = DIRECTION ( 'NONE',  ( 0.000000000000000000, 1.000000000000000000, 0.000000000000000000 ) ) ;
#24990 = CARTESIAN_POINT ( 'NONE',  ( 4.999999999999938716, 2.500000000000000000, -5.122947341949753763 ) ) ;
#24991 = VERTEX_POINT ( 'NONE', #82765 ) ;
#24992 = ORIENTED_EDGE ( 'NONE', *, *, #37157, .F. ) ;
#24993 = ORIENTED_EDGE ( 'NONE', *, *, #112921, .T. ) ;
#24994 = CARTESIAN_POINT ( 'NONE',  ( 14.59999999999989484, 12.50000000000000000, 0.6928203230275494784 ) ) ;
#24995 = ORIENTED_EDGE ( 'NONE', *, *, #16988, .F. ) ;
#24996 = DIRECTION ( 'NONE',  ( 0.000000000000000000, 0.000000000000000000, -1.000000000000000000 ) ) ;
#24997 = CIRCLE ( 'NONE', #98145, 0.09999999999999982514 ) ;
#24999 = ORIENTED_EDGE ( 'NONE', *, *, #74726, .F. ) ;
#24998 = VERTEX_POINT ( 'NONE', #52633 ) ;
#25000 = ORIENTED_EDGE ( 'NONE', *, *, #110957, .F. ) ;
#25001 = DIRECTION ( 'NONE',  ( 0.000000000000000000, 0.000000000000000000, 1.000000000000000000 ) ) ;
#25002 = AXIS2_PLACEMENT_3D ( 'NONE', #73519, #122636, #93820 ) ;
#25003 = EDGE_CURVE ( 'NONE', #97516, #29211, #55044, .T. ) ;
#25004 = CIRCLE ( 'NONE', #62671, 0.06509327318403745899 ) ;
#25005 = DIRECTION ( 'NONE',  ( 0.000000000000000000, 0.000000000000000000, -1.000000000000000000 ) ) ;
#25006 = DIRECTION ( 'NONE',  ( 0.000000000000000000, 0.000000000000000000, 1.000000000000000000 ) ) ;
#25007 = DIRECTION ( 'NONE',  ( 0.000000000000000000, 0.000000000000000000, 1.000000000000000000 ) ) ;
#25008 = EDGE_CURVE ( 'NONE', #94668, #84709, #34128, .T. ) ;
#25009 = ORIENTED_EDGE ( 'NONE', *, *, #24040, .T. ) ;
#25010 = EDGE_CURVE ( 'NONE', #28470, #22443, #74218, .T. ) ;
#25011 = AXIS2_PLACEMENT_3D ( 'NONE', #56436, #106201, #17127 ) ;
#25014 = CIRCLE ( 'NONE', #106569, 0.06509327318403745899 ) ;
#25013 = CARTESIAN_POINT ( 'NONE',  ( -11.64999999999999858, 12.50000000000000000, -1.537336459617583584 ) ) ;
#25012 = VECTOR ( 'NONE', #111649, 1000.000000000000000 ) ;
#25015 = EDGE_LOOP ( 'NONE', ( #112542, #48371 ) ) ;
#25016 = VECTOR ( 'NONE', #14995, 1000.000000000000000 ) ;
#25017 = ORIENTED_EDGE ( 'NONE', *, *, #104987, .F. ) ;
#25018 = ORIENTED_EDGE ( 'NONE', *, *, #101397, .T. ) ;
#25019 = EDGE_CURVE ( 'NONE', #77356, #50837, #63370, .T. ) ;
#25021 = ADVANCED_FACE ( 'NONE', ( #4163 ), #96798, .T. ) ;
#25020 = CARTESIAN_POINT ( 'NONE',  ( -4.400000000000025224, 2.500000000000000000, -0.4464101615137783252 ) ) ;
#25023 = ORIENTED_EDGE ( 'NONE', *, *, #89569, .F. ) ;
#25022 = EDGE_CURVE ( 'NONE', #21324, #18873, #40394, .T. ) ;
#25024 = ORIENTED_EDGE ( 'NONE', *, *, #64746, .T. ) ;
#25026 = VERTEX_POINT ( 'NONE', #112857 ) ;
#25025 = EDGE_CURVE ( 'NONE', #67610, #29442, #2818, .T. ) ;
#25027 = VECTOR ( 'NONE', #100920, 1000.000000000000000 ) ;
#25028 = DIRECTION ( 'NONE',  ( 0.000000000000000000, -0.000000000000000000, 1.000000000000000000 ) ) ;
#25029 = CARTESIAN_POINT ( 'NONE',  ( 133.2169897921533845, 0.5000000000000000000, -4.655597831175330548 ) ) ;
#25030 = DIRECTION ( 'NONE',  ( 0.000000000000000000, 1.000000000000000000, 0.000000000000000000 ) ) ;
#25031 = DIRECTION ( 'NONE',  ( 0.000000000000000000, 1.000000000000000000, 0.000000000000000000 ) ) ;
#25032 = DIRECTION ( 'NONE',  ( 0.000000000000000000, 0.000000000000000000, 1.000000000000000000 ) ) ;
#25033 = DIRECTION ( 'NONE',  ( 0.000000000000000000, 1.000000000000000000, 0.000000000000000000 ) ) ;
#25034 = VERTEX_POINT ( 'NONE', #103020 ) ;
#25035 = EDGE_CURVE ( 'NONE', #36406, #90496, #75968, .T. ) ;
#25036 = CARTESIAN_POINT ( 'NONE',  ( 13.34999999999990017, 2.500000000000000000, 1.472243186433545459 ) ) ;
#25037 = CONICAL_SURFACE ( 'NONE', #64822, 0.09999999999999982514, 0.003490658503988666988 ) ;
#25038 = VERTEX_POINT ( 'NONE', #83403 ) ;
#25039 = FACE_OUTER_BOUND ( 'NONE', #37704, .T. ) ;
#25040 = EDGE_LOOP ( 'NONE', ( #109205, #73944 ) ) ;
#25041 = DIRECTION ( 'NONE',  ( -0.000000000000000000, 1.000000000000000000, -0.000000000000000000 ) ) ;
#25042 = AXIS2_PLACEMENT_3D ( 'NONE', #81362, #28390, #34194 ) ;
#25043 = EDGE_LOOP ( 'NONE', ( #19855, #102100, #119465, #34152 ) ) ;
#25044 = VERTEX_POINT ( 'NONE', #52008 ) ;
#25045 = DIRECTION ( 'NONE',  ( 0.000000000000000000, 1.000000000000000000, 0.000000000000000000 ) ) ;
#25046 = LINE ( 'NONE', #104873, #44339 ) ;
#25047 = DIRECTION ( 'NONE',  ( 0.000000000000000000, 0.000000000000000000, -1.000000000000000000 ) ) ;
#25048 = DIRECTION ( 'NONE',  ( 0.000000000000000000, 0.000000000000000000, -1.000000000000000000 ) ) ;
#25049 = ORIENTED_EDGE ( 'NONE', *, *, #28597, .T. ) ;
#25050 = DIRECTION ( 'NONE',  ( 0.000000000000000000, 1.000000000000000000, 0.000000000000000000 ) ) ;
#25051 = DIRECTION ( 'NONE',  ( -4.274815082592931898E-19, -0.9999939076577903929, -0.003490651415223739937 ) ) ;
#25052 = DIRECTION ( 'NONE',  ( 0.000000000000000000, 1.000000000000000000, 0.000000000000000000 ) ) ;
#25053 = DIRECTION ( 'NONE',  ( 0.000000000000000000, 0.000000000000000000, 1.000000000000000000 ) ) ;
#25054 = DIRECTION ( 'NONE',  ( 0.000000000000000000, 0.000000000000000000, 1.000000000000000000 ) ) ;
#25055 = ORIENTED_EDGE ( 'NONE', *, *, #36993, .T. ) ;
#25056 = B_SPLINE_CURVE_WITH_KNOTS ( 'NONE', 3,
 ( #78797, #59815, #99716, #30992, #10647, #70893 ),
 .UNSPECIFIED., .F., .F.,
 ( 4, 2, 4 ),
 ( 0.000000000000000000, 0.5000000000000000000, 1.000000000000000000 ),
 .UNSPECIFIED. ) ;
#25057 = EDGE_LOOP ( 'NONE', ( #119212, #46144, #47432, #51263 ) ) ;
#25058 = EDGE_CURVE ( 'NONE', #60727, #7453, #42182, .T. ) ;
#25059 = AXIS2_PLACEMENT_3D ( 'NONE', #57534, #99394, #8410 ) ;
#25060 = EDGE_CURVE ( 'NONE', #16149, #31481, #69715, .T. ) ;
#25061 = EDGE_LOOP ( 'NONE', ( #124617, #27477, #76506, #47568 ) ) ;
#25062 = CARTESIAN_POINT ( 'NONE',  ( 10.84999999999990905, 12.50000000000000000, 2.230156782645134950 ) ) ;
#25063 = DIRECTION ( 'NONE',  ( 0.000000000000000000, 0.000000000000000000, 1.000000000000000000 ) ) ;
#25064 = ADVANCED_FACE ( 'NONE', ( #24472 ), #11425, .T. ) ;
#25065 = CIRCLE ( 'NONE', #10392, 0.06509327318403745899 ) ;
#25066 = CARTESIAN_POINT ( 'NONE',  ( 184.1718750003414016, 9.264065473108010111E-16, -7.564683531250000925 ) ) ;
#25067 = DIRECTION ( 'NONE',  ( -4.274815082592931898E-19, -0.9999939076577903929, -0.003490651415223739937 ) ) ;
#25068 = PLANE ( 'NONE',  #86261 ) ;
#25069 = EDGE_CURVE ( 'NONE', #80728, #50779, #113485, .T. ) ;
#25070 = DIRECTION ( 'NONE',  ( 0.000000000000000000, 0.000000000000000000, 1.000000000000000000 ) ) ;
#25071 = CARTESIAN_POINT ( 'NONE',  ( 7.899999999999924860, 2.500000000000000000, 4.330127018922196314 ) ) ;
#25072 = ORIENTED_EDGE ( 'NONE', *, *, #81032, .T. ) ;
#25073 = EDGE_CURVE ( 'NONE', #103182, #85304, #55148, .T. ) ;
#25075 = CONICAL_SURFACE ( 'NONE', #8338, 0.1000000000000000472, 0.003490658503988666988 ) ;
#25074 = AXIS2_PLACEMENT_3D ( 'NONE', #112150, #44702, #23775 ) ;
#25076 = ADVANCED_FACE ( 'NONE', ( #53301 ), #59371, .T. ) ;
#25077 = EDGE_CURVE ( 'NONE', #107141, #53057, #73915, .T. ) ;
#25078 = DIRECTION ( 'NONE',  ( -0.000000000000000000, 1.000000000000000000, -0.000000000000000000 ) ) ;
#25079 = LINE ( 'NONE', #114103, #116619 ) ;
#25080 = ORIENTED_EDGE ( 'NONE', *, *, #36355, .T. ) ;
#25081 = EDGE_CURVE ( 'NONE', #41461, #66584, #80185, .T. ) ;
#25082 = LINE ( 'NONE', #104907, #124234 ) ;
#25083 = ORIENTED_EDGE ( 'NONE', *, *, #4301, .T. ) ;
#25084 = CARTESIAN_POINT ( 'NONE',  ( 10.64999999999991331, 12.50000000000000000, -1.818653347947325916 ) ) ;
#25085 = ORIENTED_EDGE ( 'NONE', *, *, #46155, .T. ) ;
#25086 = FACE_OUTER_BOUND ( 'NONE', #4961, .T. ) ;
#25087 = CARTESIAN_POINT ( 'NONE',  ( -9.350000000000006750, 12.50000000000000000, -2.511473670974877948 ) ) ;
#25088 = DIRECTION ( 'NONE',  ( -0.000000000000000000, -1.000000000000000000, -0.000000000000000000 ) ) ;
#25089 = ORIENTED_EDGE ( 'NONE', *, *, #63262, .F. ) ;
#25090 = AXIS2_PLACEMENT_3D ( 'NONE', #3919, #83772, #113886 ) ;
#25091 = CARTESIAN_POINT ( 'NONE',  ( 14.34999999999989306, 12.50000000000000000, -1.883746621131363597 ) ) ;
#25092 = AXIS2_PLACEMENT_3D ( 'NONE', #86640, #37556, #7425 ) ;
#25093 = CARTESIAN_POINT ( 'NONE',  ( 12.29999999999990123, 2.500000000000000000, 0.4464101615137735513 ) ) ;
#25094 = ORIENTED_EDGE ( 'NONE', *, *, #111949, .F. ) ;
#25095 = AXIS2_PLACEMENT_3D ( 'NONE', #44398, #84962, #54226 ) ;
#25096 = DIRECTION ( 'NONE',  ( 0.000000000000000000, 1.000000000000000000, 0.000000000000000000 ) ) ;
#25097 = EDGE_LOOP ( 'NONE', ( #72914, #68379 ) ) ;
#25098 = ORIENTED_EDGE ( 'NONE', *, *, #110774, .F. ) ;
#25099 = DIRECTION ( 'NONE',  ( -0.000000000000000000, 1.000000000000000000, -0.000000000000000000 ) ) ;
#25100 = PLANE ( 'NONE',  #89770 ) ;
#25101 = ORIENTED_EDGE ( 'NONE', *, *, #13443, .F. ) ;
#25102 = VECTOR ( 'NONE', #53131, 1000.000000000000000 ) ;
#25103 = CARTESIAN_POINT ( 'NONE',  ( 9.999999999999912959, 2.500000000000000000, -5.022947341949754119 ) ) ;
#25104 = CARTESIAN_POINT ( 'NONE',  ( 11.89999999999990798, 2.500000000000000000, 4.576537180435972019 ) ) ;
#25105 = ORIENTED_EDGE ( 'NONE', *, *, #62877, .F. ) ;
#25107 = CARTESIAN_POINT ( 'NONE',  ( 12.69999999999990159, 12.50000000000000000, 4.611443907251934426 ) ) ;
#25106 = CIRCLE ( 'NONE', #60643, 0.06509327318403745899 ) ;
#25108 = LINE ( 'NONE', #25754, #89015 ) ;
#25109 = AXIS2_PLACEMENT_3D ( 'NONE', #18326, #48438, #88342 ) ;
#25110 = EDGE_CURVE ( 'NONE', #21005, #99549, #30023, .T. ) ;
#25111 = DIRECTION ( 'NONE',  ( 0.000000000000000000, 0.000000000000000000, 1.000000000000000000 ) ) ;
#25112 = CARTESIAN_POINT ( 'NONE',  ( -9.999999999999971578, 2.500000000000000000, -4.230127018922197557 ) ) ;
#25113 = DIRECTION ( 'NONE',  ( 0.000000000000000000, 0.000000000000000000, 1.000000000000000000 ) ) ;
#25114 = CARTESIAN_POINT ( 'NONE',  ( 7.049999999999926992, 2.500000000000000000, 2.165063509461097713 ) ) ;
#25115 = VECTOR ( 'NONE', #12995, 1000.000000000000000 ) ;
#25116 = ORIENTED_EDGE ( 'NONE', *, *, #43207, .F. ) ;
#25117 = EDGE_LOOP ( 'NONE', ( #103880, #14609 ) ) ;
#25118 = ORIENTED_EDGE ( 'NONE', *, *, #112050, .F. ) ;
#25119 = ORIENTED_EDGE ( 'NONE', *, *, #126365, .F. ) ;
#25120 = AXIS2_PLACEMENT_3D ( 'NONE', #62796, #32706, #71305 ) ;
#25121 = CARTESIAN_POINT ( 'NONE',  ( -10.00000000000000533, 2.500000000000000000, 5.022947341949748790 ) ) ;
#25122 = FACE_OUTER_BOUND ( 'NONE', #52620, .T. ) ;
#25123 = CARTESIAN_POINT ( 'NONE',  ( 14.19999999999989626, 2.500000000000000000, -0.1000000000000022815 ) ) ;
#25124 = VERTEX_POINT ( 'NONE', #106878 ) ;
#25125 = ADVANCED_FACE ( 'NONE', ( #66949 ), #71880, .T. ) ;
#25126 = FACE_BOUND ( 'NONE', #81172, .T. ) ;
#25127 = FACE_OUTER_BOUND ( 'NONE', #66959, .T. ) ;
#25128 = PLANE ( 'NONE',  #6180 ) ;
#25129 = FACE_OUTER_BOUND ( 'NONE', #55897, .T. ) ;
#25130 = LINE ( 'NONE', #14010, #32508 ) ;
#25131 = DIRECTION ( 'NONE',  ( -4.274815082592931898E-19, -0.9999939076577903929, -0.003490651415223739937 ) ) ;
#25132 = CARTESIAN_POINT ( 'NONE',  ( 11.44999999999990514, 2.500000000000000000, -6.148780366869526226 ) ) ;
#25133 = DIRECTION ( 'NONE',  ( 0.000000000000000000, 1.000000000000000000, 0.000000000000000000 ) ) ;
#25134 = CARTESIAN_POINT ( 'NONE',  ( -2.100000000000033396, 12.50000000000000000, 0.6928203230275494784 ) ) ;
#25135 = CARTESIAN_POINT ( 'NONE',  ( -2.300000000000032685, 2.500000000000000000, -4.676537180435978769 ) ) ;
#25136 = DIRECTION ( 'NONE',  ( 0.000000000000000000, 1.000000000000000000, 0.000000000000000000 ) ) ;
#25137 = ORIENTED_EDGE ( 'NONE', *, *, #103485, .F. ) ;
#25138 = EDGE_LOOP ( 'NONE', ( #48491, #46512 ) ) ;
#25139 = ORIENTED_EDGE ( 'NONE', *, *, #119586, .F. ) ;
#25140 = ORIENTED_EDGE ( 'NONE', *, *, #102342, .F. ) ;
#25141 = CARTESIAN_POINT ( 'NONE',  ( 12.09999999999990550, 12.50000000000000000, 4.957854068765711553 ) ) ;
#25142 = EDGE_LOOP ( 'NONE', ( #11665, #5207 ) ) ;
#25143 = AXIS2_PLACEMENT_3D ( 'NONE', #95372, #116280, #5677 ) ;
#25144 = CARTESIAN_POINT ( 'NONE',  ( -14.14999999999998792, 2.500000000000000000, 2.857883832488652853 ) ) ;
#25145 = EDGE_LOOP ( 'NONE', ( #67105, #15185 ) ) ;
#25146 = ORIENTED_EDGE ( 'NONE', *, *, #91573, .F. ) ;
#25147 = EDGE_CURVE ( 'NONE', #45548, #34729, #111571, .T. ) ;
#25149 = AXIS2_PLACEMENT_3D ( 'NONE', #93853, #4160, #112854 ) ;
#25148 = AXIS2_PLACEMENT_3D ( 'NONE', #43444, #23790, #64348 ) ;
#25150 = CARTESIAN_POINT ( 'NONE',  ( 10.89704209839471716, -1.500000000000189626, 8.980393934824014934 ) ) ;
#25151 = DIRECTION ( 'NONE',  ( 0.000000000000000000, 1.000000000000000000, 0.000000000000000000 ) ) ;
#25152 = FACE_OUTER_BOUND ( 'NONE', #126018, .T. ) ;
#25153 = DIRECTION ( 'NONE',  ( 0.000000000000000000, 0.000000000000000000, 1.000000000000000000 ) ) ;
#25154 = ORIENTED_EDGE ( 'NONE', *, *, #98015, .T. ) ;
#25155 = EDGE_CURVE ( 'NONE', #95676, #54254, #17465, .T. ) ;
#25156 = VERTEX_POINT ( 'NONE', #25107 ) ;
#25157 = ORIENTED_EDGE ( 'NONE', *, *, #63597, .T. ) ;
#25159 = ORIENTED_EDGE ( 'NONE', *, *, #25968, .F. ) ;
#25158 = CARTESIAN_POINT ( 'NONE',  ( 3.749999999999942268, 2.500000000000000000, -1.472243186433550122 ) ) ;
#25160 = EDGE_CURVE ( 'NONE', #7810, #106597, #96896, .T. ) ;
#25162 = EDGE_CURVE ( 'NONE', #96782, #117692, #104941, .T. ) ;
#25161 = DIRECTION ( 'NONE',  ( 0.000000000000000000, 0.000000000000000000, -1.000000000000000000 ) ) ;
#25164 = ORIENTED_EDGE ( 'NONE', *, *, #10553, .F. ) ;
#25163 = ADVANCED_FACE ( 'NONE', ( #15263 ), #4943, .T. ) ;
#25165 = EDGE_CURVE ( 'NONE', #25630, #60755, #124088, .T. ) ;
#25166 = ORIENTED_EDGE ( 'NONE', *, *, #95816, .F. ) ;
#25167 = CARTESIAN_POINT ( 'NONE',  ( 5.849999999999933031, 2.500000000000000000, 7.188010851410848723 ) ) ;
#25168 = CARTESIAN_POINT ( 'NONE',  ( 2.899999999999946620, 2.500000000000000000, -0.7928203230275543412 ) ) ;
#25169 = DIRECTION ( 'NONE',  ( 0.000000000000000000, -0.000000000000000000, 1.000000000000000000 ) ) ;
#25170 = CARTESIAN_POINT ( 'NONE',  ( -1.650000000000034772, 2.500000000000000000, 1.472243186433545459 ) ) ;
#25171 = CARTESIAN_POINT ( 'NONE',  ( -4.600000000000028955, 2.500000000000000000, -4.330127018922201643 ) ) ;
#25172 = ADVANCED_FACE ( 'NONE', ( #86600 ), #86428, .T. ) ;
#25173 = ORIENTED_EDGE ( 'NONE', *, *, #93470, .F. ) ;
#25174 = CARTESIAN_POINT ( 'NONE',  ( -6.250000000000015987, 12.50000000000000000, 1.472243186433545459 ) ) ;
#25175 = ADVANCED_FACE ( 'NONE', ( #55854 ), #78138, .T. ) ;
#25176 = CIRCLE ( 'NONE', #98329, 0.09999999999999999167 ) ;
#25177 = ADVANCED_FACE ( 'NONE', ( #95787 ), #75487, .T. ) ;
#25178 = VERTEX_POINT ( 'NONE', #4807 ) ;
#25179 = CARTESIAN_POINT ( 'NONE',  ( -1.250000000000037970, 12.50000000000000000, 2.857883832488649301 ) ) ;
#25180 = ORIENTED_EDGE ( 'NONE', *, *, #70008, .F. ) ;
#25181 = CARTESIAN_POINT ( 'NONE',  ( 4.999999999999935163, 2.500000000000000000, 3.737306695894644371 ) ) ;
#25182 = DIRECTION ( 'NONE',  ( 0.000000000000000000, -0.000000000000000000, 1.000000000000000000 ) ) ;
#25183 = CARTESIAN_POINT ( 'NONE',  ( 4.599999999999936584, 2.500000000000000000, 4.330127018922196314 ) ) ;
#25184 = CARTESIAN_POINT ( 'NONE',  ( -6.450000000000019718, 2.500000000000000000, -1.918653347947326004 ) ) ;
#25185 = ORIENTED_EDGE ( 'NONE', *, *, #114820, .F. ) ;
#25186 = AXIS2_PLACEMENT_3D ( 'NONE', #100574, #101233, #80315 ) ;
#25187 = CARTESIAN_POINT ( 'NONE',  ( 133.2169897921533845, 2.500000000000000000, -2.337293474289257933 ) ) ;
#25188 = CARTESIAN_POINT ( 'NONE',  ( 7.899999999999923084, 2.500000000000000000, -0.6928203230275542523 ) ) ;
#25189 = ORIENTED_EDGE ( 'NONE', *, *, #119423, .T. ) ;
#25190 = ORIENTED_EDGE ( 'NONE', *, *, #35160, .T. ) ;
#25191 = ORIENTED_EDGE ( 'NONE', *, *, #64480, .F. ) ;
#25192 = CARTESIAN_POINT ( 'NONE',  ( -0.6000000000000388356, 12.50000000000000000, 3.983716857408420964 ) ) ;
#25193 = DIRECTION ( 'NONE',  ( 0.000000000000000000, 0.000000000000000000, 1.000000000000000000 ) ) ;
#25194 = CARTESIAN_POINT ( 'NONE',  ( 186.7343750003414300, 8.734944146203032389, 5.348610694689227483E-16 ) ) ;
#25195 = FACE_OUTER_BOUND ( 'NONE', #50764, .T. ) ;
#25196 = VECTOR ( 'NONE', #34094, 1000.000000000000000 ) ;
#25197 = AXIS2_PLACEMENT_3D ( 'NONE', #59414, #128800, #88171 ) ;
#25198 = CARTESIAN_POINT ( 'NONE',  ( -10.84999999999999964, 2.500000000000000000, 7.088010851410848190 ) ) ;
#25199 = CARTESIAN_POINT ( 'NONE',  ( 7.899999999999923084, 2.500000000000000000, 0.6928203230275494784 ) ) ;
#25200 = VECTOR ( 'NONE', #96720, 1000.000000000000000 ) ;
#25201 = EDGE_LOOP ( 'NONE', ( #61771, #93695 ) ) ;
#25202 = CARTESIAN_POINT ( 'NONE',  ( 5.849999999999935696, 12.50000000000000000, -7.253104124594891289 ) ) ;
#25203 = ORIENTED_EDGE ( 'NONE', *, *, #73606, .F. ) ;
#25204 = CARTESIAN_POINT ( 'NONE',  ( 5.599999999999934808, 12.50000000000000000, -3.918623584224389056 ) ) ;
#25205 = CARTESIAN_POINT ( 'NONE',  ( 8.749999999999923617, 2.500000000000000000, -7.188010851410854052 ) ) ;
#25206 = ADVANCED_FACE ( 'NONE', ( #14623 ), #76151, .T. ) ;
#25207 = DIRECTION ( 'NONE',  ( -0.000000000000000000, 1.000000000000000000, -0.000000000000000000 ) ) ;
#25208 = ORIENTED_EDGE ( 'NONE', *, *, #12449, .T. ) ;
#25209 = EDGE_CURVE ( 'NONE', #53781, #97017, #105616, .T. ) ;
#25210 = EDGE_CURVE ( 'NONE', #57482, #110807, #109526, .T. ) ;
#25211 = CARTESIAN_POINT ( 'NONE',  ( -4.150000000000025224, 2.500000000000000000, 7.188010851410848723 ) ) ;
#25212 = FACE_OUTER_BOUND ( 'NONE', #68246, .T. ) ;
#25213 = ORIENTED_EDGE ( 'NONE', *, *, #15384, .F. ) ;
#25214 = ADVANCED_FACE ( 'NONE', ( #6726 ), #25894, .T. ) ;
#25215 = DIRECTION ( 'NONE',  ( -1.000000000000000000, -0.000000000000000000, -0.000000000000000000 ) ) ;
#25216 = ORIENTED_EDGE ( 'NONE', *, *, #64344, .F. ) ;
#25217 = ORIENTED_EDGE ( 'NONE', *, *, #65829, .F. ) ;
#25218 = PLANE ( 'NONE',  #117704 ) ;
#25219 = VECTOR ( 'NONE', #14690, 1000.000000000000000 ) ;
#25220 = CONICAL_SURFACE ( 'NONE', #29451, 0.1000000000000002554, 0.003490658503988666988 ) ;
#25221 = AXIS2_PLACEMENT_3D ( 'NONE', #121437, #11495, #13415 ) ;
#25222 = ORIENTED_EDGE ( 'NONE', *, *, #91988, .F. ) ;
#25223 = DIRECTION ( 'NONE',  ( 0.000000000000000000, 1.000000000000000000, 0.000000000000000000 ) ) ;
#25224 = DIRECTION ( 'NONE',  ( -0.000000000000000000, 1.000000000000000000, -0.000000000000000000 ) ) ;
#25225 = CARTESIAN_POINT ( 'NONE',  ( -11.84999999999999787, 12.50000000000000000, -1.818653347947321919 ) ) ;
#25226 = ORIENTED_EDGE ( 'NONE', *, *, #25418, .T. ) ;
#25228 = FACE_BOUND ( 'NONE', #44140, .T. ) ;
#25227 = CIRCLE ( 'NONE', #33659, 0.06509327318403745899 ) ;
#25230 = ORIENTED_EDGE ( 'NONE', *, *, #62198, .T. ) ;
#25229 = CARTESIAN_POINT ( 'NONE',  ( -9.200000000000009948, 12.50000000000000000, -4.330127018922197202 ) ) ;
#25231 = VECTOR ( 'NONE', #10806, 1000.000000000000000 ) ;
#25232 = DIRECTION ( 'NONE',  ( -0.000000000000000000, 1.000000000000000000, -0.000000000000000000 ) ) ;
#25233 = DIRECTION ( 'NONE',  ( -4.274815082592931898E-19, -0.9999939076577903929, -0.003490651415223739937 ) ) ;
#25234 = EDGE_CURVE ( 'NONE', #121575, #80079, #47342, .T. ) ;
#25235 = ORIENTED_EDGE ( 'NONE', *, *, #13021, .F. ) ;
#25236 = ORIENTED_EDGE ( 'NONE', *, *, #38957, .F. ) ;
#25237 = ORIENTED_EDGE ( 'NONE', *, *, #110256, .F. ) ;
#25238 = DIRECTION ( 'NONE',  ( 0.000000000000000000, -0.9999939076577903929, 0.003490651415223739937 ) ) ;
#25239 = CARTESIAN_POINT ( 'NONE',  ( 14.14999999999989555, 12.50000000000000000, 2.099970236277060032 ) ) ;
#25240 = FACE_OUTER_BOUND ( 'NONE', #20377, .T. ) ;
#25241 = FACE_BOUND ( 'NONE', #75179, .T. ) ;
#25242 = ORIENTED_EDGE ( 'NONE', *, *, #63262, .T. ) ;
#25243 = CARTESIAN_POINT ( 'NONE',  ( 186.9010416670080303, -4.367472073101519747, 7.564683531249999149 ) ) ;
#25244 = CARTESIAN_POINT ( 'NONE',  ( -9.800000000000004263, 2.500000000000000000, -0.4464101615137783252 ) ) ;
#25245 = FACE_OUTER_BOUND ( 'NONE', #128541, .T. ) ;
#25246 = CARTESIAN_POINT ( 'NONE',  ( -5.400000000000020783, 2.500000000000000000, 5.022947341949748790 ) ) ;
#25247 = EDGE_CURVE ( 'NONE', #63253, #47460, #88591, .T. ) ;
#25248 = CARTESIAN_POINT ( 'NONE',  ( 5.399999999999932854, 12.50000000000000000, 4.957854068765711553 ) ) ;
#25249 = CARTESIAN_POINT ( 'NONE',  ( -2.100000000000034284, 12.50000000000000000, -4.395220292106239768 ) ) ;
#25250 = CARTESIAN_POINT ( 'NONE',  ( -8.550000000000009592, 2.500000000000000000, 6.841600689897072485 ) ) ;
#25251 = DIRECTION ( 'NONE',  ( 0.000000000000000000, 1.000000000000000000, 0.000000000000000000 ) ) ;
#25252 = CONICAL_SURFACE ( 'NONE', #23128, 0.1000000000000002554, 0.003490658503988666988 ) ;
#25253 = CONICAL_SURFACE ( 'NONE', #108884, 0.1000000000000000472, 0.003490658503988666988 ) ;
#25254 = DIRECTION ( 'NONE',  ( -0.000000000000000000, 1.000000000000000000, -0.000000000000000000 ) ) ;
#25255 = EDGE_LOOP ( 'NONE', ( #104408, #724 ) ) ;
#25256 = ORIENTED_EDGE ( 'NONE', *, *, #40464, .F. ) ;
#25257 = ORIENTED_EDGE ( 'NONE', *, *, #94940, .F. ) ;
#25258 = EDGE_LOOP ( 'NONE', ( #21103, #50309, #21432, #76213 ) ) ;
#25259 = ORIENTED_EDGE ( 'NONE', *, *, #3748, .T. ) ;
#25260 = CARTESIAN_POINT ( 'NONE',  ( -0.8500000000000382805, 2.500000000000000000, -2.857883832488653741 ) ) ;
#25261 = CARTESIAN_POINT ( 'NONE',  ( 6.249999999999932498, 2.500000000000000000, -2.957883832488653830 ) ) ;
#25262 = ORIENTED_EDGE ( 'NONE', *, *, #64650, .F. ) ;
#25263 = EDGE_CURVE ( 'NONE', #46243, #23743, #15407, .T. ) ;
#25264 = FACE_BOUND ( 'NONE', #77563, .T. ) ;
#25265 = CARTESIAN_POINT ( 'NONE',  ( -1.250000000000001110, 2.500000000000000000, -2.065063509461102065 ) ) ;
#25266 = CIRCLE ( 'NONE', #67108, 0.09999999999999982514 ) ;
#25267 = LINE ( 'NONE', #56660, #65739 ) ;
#25268 = ORIENTED_EDGE ( 'NONE', *, *, #89471, .T. ) ;
#25269 = CARTESIAN_POINT ( 'NONE',  ( 2.499999999999945377, 2.500000000000000000, 5.122947341949749323 ) ) ;
#25270 = ADVANCED_FACE ( 'NONE', ( #40759 ), #9337, .T. ) ;
#25271 = CARTESIAN_POINT ( 'NONE',  ( -14.99999999999998224, 2.500000000000000000, -0.6928203230275519209 ) ) ;
#25272 = DIRECTION ( 'NONE',  ( -0.000000000000000000, -1.000000000000000000, -0.000000000000000000 ) ) ;
#25273 = ORIENTED_EDGE ( 'NONE', *, *, #44977, .T. ) ;
#25274 = DIRECTION ( 'NONE',  ( -0.000000000000000000, -1.000000000000000000, -0.000000000000000000 ) ) ;
#25275 = CONICAL_SURFACE ( 'NONE', #142, 0.09999999999999982514, 0.003490658503988666988 ) ;
#25276 = ORIENTED_EDGE ( 'NONE', *, *, #41922, .F. ) ;
#25277 = AXIS2_PLACEMENT_3D ( 'NONE', #113641, #6236, #5593 ) ;
#25278 = EDGE_LOOP ( 'NONE', ( #110644, #61717, #109858, #39983 ) ) ;
#25279 = VERTEX_POINT ( 'NONE', #117994 ) ;
#25280 = CARTESIAN_POINT ( 'NONE',  ( -5.600000000000023626, 2.500000000000000000, -4.676537180435977881 ) ) ;
#25281 = DIRECTION ( 'NONE',  ( -0.000000000000000000, -1.000000000000000000, -0.000000000000000000 ) ) ;
#25282 = DIRECTION ( 'NONE',  ( 0.000000000000000000, 0.000000000000000000, 1.000000000000000000 ) ) ;
#25283 = ORIENTED_EDGE ( 'NONE', *, *, #58897, .T. ) ;
#25284 = DIRECTION ( 'NONE',  ( -0.000000000000000000, -1.000000000000000000, -0.000000000000000000 ) ) ;
#25285 = AXIS2_PLACEMENT_3D ( 'NONE', #27328, #57464, #58113 ) ;
#25286 = PLANE ( 'NONE',  #24008 ) ;
#25287 = ADVANCED_FACE ( 'NONE', ( #120582 ), #82348, .T. ) ;
#25288 = CARTESIAN_POINT ( 'NONE',  ( 5.849999999999931255, 2.500000000000000000, 2.857883832488649301 ) ) ;
#25289 = AXIS2_PLACEMENT_3D ( 'NONE', #13994, #53941, #112864 ) ;
#25290 = CARTESIAN_POINT ( 'NONE',  ( 183.8645833340161175, -6.668395609140180369, 3.849999999999994760 ) ) ;
#25291 = CARTESIAN_POINT ( 'NONE',  ( -5.000000000000023093, 2.500000000000000000, 4.922947341949748257 ) ) ;
#25292 = DIRECTION ( 'NONE',  ( -0.000000000000000000, -1.000000000000000000, -0.000000000000000000 ) ) ;
#25293 = EDGE_LOOP ( 'NONE', ( #18299, #105159, #8244, #89343 ) ) ;
#25294 = DIRECTION ( 'NONE',  ( 0.000000000000000000, 0.000000000000000000, 1.000000000000000000 ) ) ;
#25295 = EDGE_CURVE ( 'NONE', #8330, #123664, #18511, .T. ) ;
#25296 = ORIENTED_EDGE ( 'NONE', *, *, #95109, .F. ) ;
#25297 = EDGE_LOOP ( 'NONE', ( #105651, #57124, #64140, #119678 ) ) ;
#25298 = CARTESIAN_POINT ( 'NONE',  ( -12.89999999999999147, 12.50000000000000000, -4.265033745738161741 ) ) ;
#25299 = CARTESIAN_POINT ( 'NONE',  ( 129.5000000000000000, 1.375000000000000000, 7.634788798650556707 ) ) ;
#25300 = EDGE_CURVE ( 'NONE', #87351, #118459, #108812, .T. ) ;
#25301 = CARTESIAN_POINT ( 'NONE',  ( -2.500000000000030642, 2.500000000000000000, -0.6928203230275541413 ) ) ;
#25303 = EDGE_CURVE ( 'NONE', #97440, #36662, #29179, .T. ) ;
#25302 = DIRECTION ( 'NONE',  ( 0.000000000000000000, 0.000000000000000000, 1.000000000000000000 ) ) ;
#25304 = EDGE_CURVE ( 'NONE', #96622, #99498, #13268, .T. ) ;
#25305 = DIRECTION ( 'NONE',  ( 0.000000000000000000, -0.000000000000000000, 1.000000000000000000 ) ) ;
#25306 = ADVANCED_FACE ( 'NONE', ( #68250 ), #63459, .T. ) ;
#25307 = EDGE_LOOP ( 'NONE', ( #80987, #16208 ) ) ;
#25308 = ORIENTED_EDGE ( 'NONE', *, *, #67183, .T. ) ;
#25309 = DIRECTION ( 'NONE',  ( 0.000000000000000000, 1.000000000000000000, 0.000000000000000000 ) ) ;
#25310 = CARTESIAN_POINT ( 'NONE',  ( 9.599999999999914380, 12.50000000000000000, -5.088040615133791356 ) ) ;
#25311 = EDGE_CURVE ( 'NONE', #98287, #19378, #69538, .T. ) ;
#25313 = CARTESIAN_POINT ( 'NONE',  ( 14.59999999999989484, 2.500000000000000000, -0.5928203230275541635 ) ) ;
#25312 = CIRCLE ( 'NONE', #117321, 0.06509327318403745899 ) ;
#25314 = ORIENTED_EDGE ( 'NONE', *, *, #51656, .T. ) ;
#25315 = ORIENTED_EDGE ( 'NONE', *, *, #51539, .F. ) ;
#25316 = CIRCLE ( 'NONE', #125662, 0.06509327318403745899 ) ;
#25317 = CONICAL_SURFACE ( 'NONE', #40019, 0.1000000000000002554, 0.003490658503988666988 ) ;
#25318 = EDGE_CURVE ( 'NONE', #119603, #9738, #109474, .T. ) ;
#25319 = DIRECTION ( 'NONE',  ( -4.274815082592931898E-19, -0.9999939076577903929, -0.003490651415223739937 ) ) ;
#25320 = EDGE_CURVE ( 'NONE', #66380, #106765, #752, .T. ) ;
#25321 = VERTEX_POINT ( 'NONE', #89826 ) ;
#25322 = DIRECTION ( 'NONE',  ( 0.000000000000000000, 0.000000000000000000, 1.000000000000000000 ) ) ;
#25323 = EDGE_CURVE ( 'NONE', #10983, #71602, #128420, .T. ) ;
#25325 = EDGE_CURVE ( 'NONE', #76363, #126865, #122148, .T. ) ;
#25324 = CIRCLE ( 'NONE', #104736, 0.06509327318403745899 ) ;
#25326 = CARTESIAN_POINT ( 'NONE',  ( 11.69999999999990514, 2.500000000000000000, -2.276824562219559311E-15 ) ) ;
#25327 = ORIENTED_EDGE ( 'NONE', *, *, #115199, .T. ) ;
#25328 = DIRECTION ( 'NONE',  ( 0.000000000000000000, 0.000000000000000000, 1.000000000000000000 ) ) ;
#25329 = CARTESIAN_POINT ( 'NONE',  ( 185.5416666666666856, -4.445597072760063107, 7.700000000000102318 ) ) ;
#25330 = CARTESIAN_POINT ( 'NONE',  ( 4.149999999999936406, 2.500000000000000000, 6.495190528383297135 ) ) ;
#25331 = VECTOR ( 'NONE', #26467, 1000.000000000000000 ) ;
#25333 = ADVANCED_FACE ( 'NONE', ( #143 ), #25997, .T. ) ;
#25332 = CARTESIAN_POINT ( 'NONE',  ( 129.5000000000000000, 0.000000000000000000, 0.000000000000000000 ) ) ;
#25334 = EDGE_LOOP ( 'NONE', ( #40282, #121366, #123844, #71481 ) ) ;
#25335 = FACE_OUTER_BOUND ( 'NONE', #115783, .T. ) ;
#25336 = DIRECTION ( 'NONE',  ( 0.000000000000000000, 0.000000000000000000, -1.000000000000000000 ) ) ;
#25337 = VERTEX_POINT ( 'NONE', #47989 ) ;
#25338 = ORIENTED_EDGE ( 'NONE', *, *, #92069, .F. ) ;
#25339 = PLANE ( 'NONE',  #27459 ) ;
#25340 = CARTESIAN_POINT ( 'NONE',  ( 9.349999999999919709, 12.50000000000000000, -6.148780366869526226 ) ) ;
#25341 = CARTESIAN_POINT ( 'NONE',  ( 8.149999999999920419, 2.500000000000000000, -1.718653347947325827 ) ) ;
#25342 = DIRECTION ( 'NONE',  ( 0.000000000000000000, 0.000000000000000000, 1.000000000000000000 ) ) ;
#25343 = CARTESIAN_POINT ( 'NONE',  ( -9.550000000000006040, 12.50000000000000000, 2.230156782645134950 ) ) ;
#25344 = DIRECTION ( 'NONE',  ( 0.000000000000000000, -0.000000000000000000, 1.000000000000000000 ) ) ;
#25345 = CARTESIAN_POINT ( 'NONE',  ( -7.500000000000001776, -1.500000000000000000, -9.999999999999998224 ) ) ;
#25346 = DIRECTION ( 'NONE',  ( 0.000000000000000000, -0.000000000000000000, 1.000000000000000000 ) ) ;
#25347 = CARTESIAN_POINT ( 'NONE',  ( -1.050000000000038236, 2.500000000000000000, -6.048780366869526581 ) ) ;
#25348 = FACE_OUTER_BOUND ( 'NONE', #19120, .T. ) ;
#25349 = CARTESIAN_POINT ( 'NONE',  ( 139.9358549477330200, 2.500000000000000000, -3.576063159858998475 ) ) ;
#25350 = CIRCLE ( 'NONE', #83847, 0.09999999999999982514 ) ;
#25351 = ORIENTED_EDGE ( 'NONE', *, *, #106176, .F. ) ;
#25352 = AXIS2_PLACEMENT_3D ( 'NONE', #87950, #48061, #222 ) ;
#25353 = EDGE_LOOP ( 'NONE', ( #60289, #68706, #43931, #107555 ) ) ;
#25354 = ORIENTED_EDGE ( 'NONE', *, *, #19270, .T. ) ;
#25355 = LINE ( 'NONE', #75753, #58317 ) ;
#25356 = DIRECTION ( 'NONE',  ( 0.000000000000000000, 1.000000000000000000, 0.000000000000000000 ) ) ;
#25357 = DIRECTION ( 'NONE',  ( 0.000000000000000000, 0.000000000000000000, 1.000000000000000000 ) ) ;
#25358 = AXIS2_PLACEMENT_3D ( 'NONE', #125675, #49091, #598 ) ;
#25359 = AXIS2_PLACEMENT_3D ( 'NONE', #5856, #16313, #75898 ) ;
#25360 = EDGE_LOOP ( 'NONE', ( #55464, #55955 ) ) ;
#25361 = CARTESIAN_POINT ( 'NONE',  ( -11.89999999999999503, 12.50000000000000000, 3.983716857408420076 ) ) ;
#25362 = ADVANCED_FACE ( 'NONE', ( #87878 ), #30291, .T. ) ;
#25363 = EDGE_CURVE ( 'NONE', #97929, #81732, #99154, .T. ) ;
#25364 = CARTESIAN_POINT ( 'NONE',  ( 1.049999999999952083, 2.500000000000000000, 6.841600689897072485 ) ) ;
#25366 = EDGE_LOOP ( 'NONE', ( #93144, #38923 ) ) ;
#25365 = LINE ( 'NONE', #44373, #41309 ) ;
#25367 = DIRECTION ( 'NONE',  ( 0.000000000000000000, 0.000000000000000000, 1.000000000000000000 ) ) ;
#25368 = AXIS2_PLACEMENT_3D ( 'NONE', #101228, #11547, #42983 ) ;
#25369 = ORIENTED_EDGE ( 'NONE', *, *, #94511, .T. ) ;
#25370 = ADVANCED_FACE ( 'NONE', ( #127818 ), #9265, .T. ) ;
#25371 = AXIS2_PLACEMENT_3D ( 'NONE', #47480, #89339, #6874 ) ;
#25372 = VERTEX_POINT ( 'NONE', #83248 ) ;
#25373 = ORIENTED_EDGE ( 'NONE', *, *, #114585, .T. ) ;
#25375 = VERTEX_POINT ( 'NONE', #52475 ) ;
#25374 = VECTOR ( 'NONE', #61296, 1000.000000000000000 ) ;
#25376 = DIRECTION ( 'NONE',  ( 0.000000000000000000, -0.000000000000000000, 1.000000000000000000 ) ) ;
#25377 = AXIS2_PLACEMENT_3D ( 'NONE', #55370, #46187, #86089 ) ;
#25378 = CARTESIAN_POINT ( 'NONE',  ( -13.09999999999999254, 12.50000000000000000, 0.3464101615137777923 ) ) ;
#25379 = DIRECTION ( 'NONE',  ( -0.000000000000000000, 1.000000000000000000, -0.000000000000000000 ) ) ;
#25380 = FACE_OUTER_BOUND ( 'NONE', #20379, .T. ) ;
#25381 = ORIENTED_EDGE ( 'NONE', *, *, #48110, .T. ) ;
#25382 = AXIS2_PLACEMENT_3D ( 'NONE', #72782, #43332, #113337 ) ;
#25383 = AXIS2_PLACEMENT_3D ( 'NONE', #105836, #16142, #98570 ) ;
#25384 = LINE ( 'NONE', #3827, #10514 ) ;
#25385 = VERTEX_POINT ( 'NONE', #42025 ) ;
#25386 = CARTESIAN_POINT ( 'NONE',  ( 21.23528140090950345, -2.699413673072311504, -2.293764360948880476 ) ) ;
#25387 = DIRECTION ( 'NONE',  ( 0.000000000000000000, 0.000000000000000000, 1.000000000000000000 ) ) ;
#25388 = CARTESIAN_POINT ( 'NONE',  ( -17.50000000000000000, -1.500000000000000000, 9.000000000000001776 ) ) ;
#25389 = CARTESIAN_POINT ( 'NONE',  ( 16.58100817950494843, -2.557139044001658146, 6.067820687733448182 ) ) ;
#25390 = ORIENTED_EDGE ( 'NONE', *, *, #1695, .F. ) ;
#25391 = ORIENTED_EDGE ( 'NONE', *, *, #111641, .T. ) ;
#25392 = ORIENTED_EDGE ( 'NONE', *, *, #9273, .T. ) ;
#25393 = DIRECTION ( 'NONE',  ( 0.000000000000000000, 0.000000000000000000, 1.000000000000000000 ) ) ;
#25394 = FACE_OUTER_BOUND ( 'NONE', #46699, .T. ) ;
#25395 = DIRECTION ( 'NONE',  ( 0.000000000000000000, -0.9999939076577903929, 0.003490651415223739937 ) ) ;
#25396 = FACE_BOUND ( 'NONE', #128836, .T. ) ;
#25397 = CARTESIAN_POINT ( 'NONE',  ( -11.89999999999999680, 12.50000000000000000, 0.2813168883297402778 ) ) ;
#25398 = DIRECTION ( 'NONE',  ( 0.000000000000000000, 0.000000000000000000, 1.000000000000000000 ) ) ;
#25399 = DIRECTION ( 'NONE',  ( 0.000000000000000000, 1.000000000000000000, 0.000000000000000000 ) ) ;
#25400 = LINE ( 'NONE', #23485, #95988 ) ;
#25401 = EDGE_CURVE ( 'NONE', #97177, #67035, #30120, .T. ) ;
#25402 = CIRCLE ( 'NONE', #50541, 0.1000000000000002554 ) ;
#25403 = AXIS2_PLACEMENT_3D ( 'NONE', #90069, #49533, #69143 ) ;
#25405 = CIRCLE ( 'NONE', #115278, 0.06509327318403743123 ) ;
#25404 = DIRECTION ( 'NONE',  ( 0.000000000000000000, -0.000000000000000000, 1.000000000000000000 ) ) ;
#25406 = CARTESIAN_POINT ( 'NONE',  ( 187.5000000000000000, 0.000000000000000000, 0.000000000000000000 ) ) ;
#25407 = CARTESIAN_POINT ( 'NONE',  ( -1.450000000000035927, 12.50000000000000000, -1.883746621131363597 ) ) ;
#25408 = CIRCLE ( 'NONE', #42160, 0.06509327318403745899 ) ;
#25409 = DIRECTION ( 'NONE',  ( 0.000000000000000000, 0.000000000000000000, 1.000000000000000000 ) ) ;
#25410 = AXIS2_PLACEMENT_3D ( 'NONE', #19349, #96614, #116903 ) ;
#25411 = ORIENTED_EDGE ( 'NONE', *, *, #48625, .T. ) ;
#25412 = VERTEX_POINT ( 'NONE', #21745 ) ;
#25413 = ORIENTED_EDGE ( 'NONE', *, *, #106634, .F. ) ;
#25414 = EDGE_LOOP ( 'NONE', ( #26027, #125427 ) ) ;
#25416 = EDGE_CURVE ( 'NONE', #15697, #77313, #30930, .T. ) ;
#25415 = CONICAL_SURFACE ( 'NONE', #73538, 0.1000000000000000472, 0.003490658503988666988 ) ;
#25417 = CARTESIAN_POINT ( 'NONE',  ( 9.599999999999914380, 12.50000000000000000, 3.702399969078682407 ) ) ;
#25418 = EDGE_CURVE ( 'NONE', #34661, #53613, #38531, .T. ) ;
#25419 = FACE_BOUND ( 'NONE', #117441, .T. ) ;
#25420 = CARTESIAN_POINT ( 'NONE',  ( -6.900000000000015454, 12.50000000000000000, 3.983716857408420076 ) ) ;
#25421 = VECTOR ( 'NONE', #21412, 1000.000000000000000 ) ;
#25422 = EDGE_LOOP ( 'NONE', ( #88033, #75677, #101451, #94348 ) ) ;
#25423 = CARTESIAN_POINT ( 'NONE',  ( 76.45227062019213804, 3.905198618281777723, 5.870121734766100552 ) ) ;
#25424 = EDGE_CURVE ( 'NONE', #1183, #106661, #121867, .T. ) ;
#25425 = CARTESIAN_POINT ( 'NONE',  ( -1.650000000000035660, 12.50000000000000000, 2.857883832488649301 ) ) ;
#25426 = VERTEX_POINT ( 'NONE', #112057 ) ;
#25427 = DIRECTION ( 'NONE',  ( 0.000000000000000000, 0.000000000000000000, 1.000000000000000000 ) ) ;
#25428 = CARTESIAN_POINT ( 'NONE',  ( 7.049999999999930544, 2.500000000000000000, -6.495190528383302464 ) ) ;
#25429 = ADVANCED_FACE ( 'NONE', ( #22401 ), #63556, .T. ) ;
#25430 = VERTEX_POINT ( 'NONE', #21085 ) ;
#25431 = DIRECTION ( 'NONE',  ( 0.000000000000000000, -0.000000000000000000, 1.000000000000000000 ) ) ;
#25432 = DIRECTION ( 'NONE',  ( 0.000000000000000000, 0.000000000000000000, -1.000000000000000000 ) ) ;
#25433 = AXIS2_PLACEMENT_3D ( 'NONE', #62740, #33288, #45674 ) ;
#25434 = AXIS2_PLACEMENT_3D ( 'NONE', #64311, #26335, #126468 ) ;
#25435 = VERTEX_POINT ( 'NONE', #61677 ) ;
#25436 = LINE ( 'NONE', #104027, #17543 ) ;
#25437 = DIRECTION ( 'NONE',  ( 0.000000000000000000, 0.000000000000000000, -1.000000000000000000 ) ) ;
#25438 = DIRECTION ( 'NONE',  ( -0.000000000000000000, 1.000000000000000000, -0.000000000000000000 ) ) ;
#25439 = EDGE_LOOP ( 'NONE', ( #124406, #19710, #15767, #109192 ) ) ;
#25440 = VERTEX_POINT ( 'NONE', #62319 ) ;
#25441 = FACE_OUTER_BOUND ( 'NONE', #46842, .T. ) ;
#25442 = AXIS2_PLACEMENT_3D ( 'NONE', #67224, #57450, #7682 ) ;
#25443 = ORIENTED_EDGE ( 'NONE', *, *, #125046, .F. ) ;
#25444 = CARTESIAN_POINT ( 'NONE',  ( 4.349999999999940137, 2.500000000000000000, -2.411473670974877859 ) ) ;
#25445 = AXIS2_PLACEMENT_3D ( 'NONE', #103091, #95212, #4872 ) ;
#25446 = CARTESIAN_POINT ( 'NONE',  ( -12.29999999999999538, 12.50000000000000000, -4.676537180435976104 ) ) ;
#25448 = EDGE_CURVE ( 'NONE', #108113, #10762, #96997, .T. ) ;
#25447 = CONICAL_SURFACE ( 'NONE', #57044, 0.09999999999999982514, 0.003490658503988666988 ) ;
#25449 = VERTEX_POINT ( 'NONE', #11262 ) ;
#25450 = AXIS2_PLACEMENT_3D ( 'NONE', #80514, #120426, #77055 ) ;
#25451 = CONICAL_SURFACE ( 'NONE', #42211, 0.09999999999999999167, 0.003490658503988666988 ) ;
#25452 = CARTESIAN_POINT ( 'NONE',  ( 108.0000000000000142, 5.855766388782936538, -5.000000000000004441 ) ) ;
#25453 = CARTESIAN_POINT ( 'NONE',  ( -10.00000000000000355, 2.500000000000000000, -0.6928203230275541413 ) ) ;
#25454 = CARTESIAN_POINT ( 'NONE',  ( -6.050000000000017586, 2.500000000000000000, 1.918653347947321564 ) ) ;
#25455 = CARTESIAN_POINT ( 'NONE',  ( -1.050000000000037348, 2.500000000000000000, -2.511473670974877948 ) ) ;
#25456 = EDGE_CURVE ( 'NONE', #55712, #29239, #13361, .T. ) ;
#25457 = CARTESIAN_POINT ( 'NONE',  ( -7.700000000000014388, 2.500000000000000000, -0.3464101615137782364 ) ) ;
#25458 = EDGE_CURVE ( 'NONE', #52063, #55284, #69281, .T. ) ;
#25459 = VERTEX_POINT ( 'NONE', #75988 ) ;
#25460 = PRODUCT_DEFINITION_FORMATION_WITH_SPECIFIED_SOURCE ( 'ANY', '', #57498, .NOT_KNOWN. ) ;
#25461 = AXIS2_PLACEMENT_3D ( 'NONE', #5450, #63746, #125243 ) ;
#25462 = ORIENTED_EDGE ( 'NONE', *, *, #101348, .T. ) ;
#25463 = CARTESIAN_POINT ( 'NONE',  ( 12.94999999999990337, 12.50000000000000000, 2.165063509461097713 ) ) ;
#25465 = VECTOR ( 'NONE', #47987, 1000.000000000000000 ) ;
#25464 = DIRECTION ( 'NONE',  ( 0.000000000000000000, 1.000000000000000000, 0.000000000000000000 ) ) ;
#25466 = VECTOR ( 'NONE', #2798, 1000.000000000000000 ) ;
#25467 = VECTOR ( 'NONE', #73741, 1000.000000000000000 ) ;
#25468 = EDGE_CURVE ( 'NONE', #127685, #39745, #34321, .T. ) ;
#25469 = CARTESIAN_POINT ( 'NONE',  ( -9.150000000000009237, 2.500000000000000000, -2.165063509461101710 ) ) ;
#25471 = VERTEX_POINT ( 'NONE', #17026 ) ;
#25470 = EDGE_LOOP ( 'NONE', ( #105447, #57512, #79101, #80008 ) ) ;
#25472 = EDGE_CURVE ( 'NONE', #14841, #50907, #86611, .T. ) ;
#25473 = ORIENTED_EDGE ( 'NONE', *, *, #20758, .F. ) ;
#25474 = EDGE_CURVE ( 'NONE', #37222, #107667, #42747, .T. ) ;
#25475 = DIRECTION ( 'NONE',  ( 0.000000000000000000, 0.000000000000000000, -1.000000000000000000 ) ) ;
#25476 = AXIS2_PLACEMENT_3D ( 'NONE', #2225, #3533, #63748 ) ;
#25477 = CARTESIAN_POINT ( 'NONE',  ( 1.249999999999952038, 12.50000000000000000, 2.922977105672686982 ) ) ;
#25478 = LINE ( 'NONE', #55599, #16340 ) ;
#25479 = EDGE_CURVE ( 'NONE', #83685, #96204, #19739, .T. ) ;
#25480 = LINE ( 'NONE', #15654, #107545 ) ;
#25481 = VECTOR ( 'NONE', #95004, 1000.000000000000000 ) ;
#25482 = CARTESIAN_POINT ( 'NONE',  ( -7.500000000000015099, 2.500000000000000000, -0.6928203230275541413 ) ) ;
#25483 = DIRECTION ( 'NONE',  ( 0.000000000000000000, 0.000000000000000000, 1.000000000000000000 ) ) ;
#25484 = DIRECTION ( 'NONE',  ( -0.000000000000000000, -1.000000000000000000, -0.000000000000000000 ) ) ;
#25485 = DIRECTION ( 'NONE',  ( -0.000000000000000000, 1.000000000000000000, -0.000000000000000000 ) ) ;
#25487 = EDGE_CURVE ( 'NONE', #127183, #16787, #94950, .T. ) ;
#25486 = CARTESIAN_POINT ( 'NONE',  ( 11.04999999999991012, 12.50000000000000000, -1.818653347947326138 ) ) ;
#25488 = EDGE_LOOP ( 'NONE', ( #129121, #97800 ) ) ;
#25489 = CARTESIAN_POINT ( 'NONE',  ( 11.04999999999991189, 2.500000000000000000, -2.511473670974877948 ) ) ;
#25490 = EDGE_LOOP ( 'NONE', ( #9611, #68494 ) ) ;
#25491 = ORIENTED_EDGE ( 'NONE', *, *, #47179, .T. ) ;
#25492 = DIRECTION ( 'NONE',  ( -0.000000000000000000, -1.000000000000000000, -0.000000000000000000 ) ) ;
#25493 = DIRECTION ( 'NONE',  ( 0.000000000000000000, 1.000000000000000000, 0.000000000000000000 ) ) ;
#25494 = DIRECTION ( 'NONE',  ( 0.000000000000000000, 0.000000000000000000, -1.000000000000000000 ) ) ;
#25495 = DIRECTION ( 'NONE',  ( 0.000000000000000000, 0.000000000000000000, 1.000000000000000000 ) ) ;
#25496 = DIRECTION ( 'NONE',  ( -0.000000000000000000, -1.000000000000000000, -0.000000000000000000 ) ) ;
#25497 = DIRECTION ( 'NONE',  ( -0.000000000000000000, 1.000000000000000000, -0.000000000000000000 ) ) ;
#25498 = VECTOR ( 'NONE', #10299, 1000.000000000000000 ) ;
#25499 = CARTESIAN_POINT ( 'NONE',  ( 2.299999999999947864, 2.500000000000000000, 3.983716857408420964 ) ) ;
#25500 = VERTEX_POINT ( 'NONE', #5303 ) ;
#25501 = DIRECTION ( 'NONE',  ( -0.000000000000000000, 1.000000000000000000, -0.000000000000000000 ) ) ;
#25502 = CONICAL_SURFACE ( 'NONE', #35988, 0.1000000000000002554, 0.003490658503988666988 ) ;
#25503 = CIRCLE ( 'NONE', #127924, 0.06509327318403745899 ) ;
#25504 = CARTESIAN_POINT ( 'NONE',  ( 187.5000000000000000, 0.000000000000000000, 7.700000000000000178 ) ) ;
#25505 = ORIENTED_EDGE ( 'NONE', *, *, #57969, .T. ) ;
#25506 = CIRCLE ( 'NONE', #98664, 0.06509327318403741736 ) ;
#25507 = EDGE_LOOP ( 'NONE', ( #25881, #91974 ) ) ;
#25508 = AXIS2_PLACEMENT_3D ( 'NONE', #64162, #104097, #82537 ) ;
#25509 = VERTEX_POINT ( 'NONE', #106729 ) ;
#25510 = CONICAL_SURFACE ( 'NONE', #15123, 0.1000000000000002554, 0.003490658503988666988 ) ;
#25511 = AXIS2_PLACEMENT_3D ( 'NONE', #106840, #25078, #37491 ) ;
#25512 = VERTEX_POINT ( 'NONE', #124450 ) ;
#25513 = CARTESIAN_POINT ( 'NONE',  ( 12.29999999999990123, 12.50000000000000000, 0.3464101615137735735 ) ) ;
#25514 = DIRECTION ( 'NONE',  ( 0.000000000000000000, 0.000000000000000000, 1.000000000000000000 ) ) ;
#25515 = AXIS2_PLACEMENT_3D ( 'NONE', #85567, #56723, #106500 ) ;
#25516 = DIRECTION ( 'NONE',  ( -4.274815082592931898E-19, -0.9999939076577903929, -0.003490651415223739937 ) ) ;
#25517 = EDGE_CURVE ( 'NONE', #120135, #120902, #45249, .T. ) ;
#25518 = DIRECTION ( 'NONE',  ( -0.000000000000000000, 1.000000000000000000, -0.000000000000000000 ) ) ;
#25519 = CARTESIAN_POINT ( 'NONE',  ( -11.69999999999999574, 12.50000000000000000, 4.330127018922196314 ) ) ;
#25520 = ORIENTED_EDGE ( 'NONE', *, *, #114608, .T. ) ;
#25521 = CARTESIAN_POINT ( 'NONE',  ( -1.050000000000037348, 2.500000000000000000, -2.511473670974877948 ) ) ;
#25522 = CARTESIAN_POINT ( 'NONE',  ( -4.600000000000024514, 12.50000000000000000, -0.6277270498435167934 ) ) ;
#25524 = EDGE_CURVE ( 'NONE', #71846, #21325, #101207, .T. ) ;
#25523 = DIRECTION ( 'NONE',  ( 0.000000000000000000, 0.000000000000000000, -1.000000000000000000 ) ) ;
#25525 = EDGE_LOOP ( 'NONE', ( #23361, #62837 ) ) ;
#25526 = B_SPLINE_CURVE_WITH_KNOTS ( 'NONE', 3,
 ( #62483, #13353, #34315, #71641 ),
 .UNSPECIFIED., .F., .F.,
 ( 4, 4 ),
 ( 0.2000000000000000944, 0.7999999999999997113 ),
 .UNSPECIFIED. ) ;
#25527 = VERTEX_POINT ( 'NONE', #37374 ) ;
#25528 = ORIENTED_EDGE ( 'NONE', *, *, #40311, .T. ) ;
#25529 = FACE_OUTER_BOUND ( 'NONE', #114010, .T. ) ;
#25530 = DIRECTION ( 'NONE',  ( 0.000000000000000000, -0.000000000000000000, 1.000000000000000000 ) ) ;
#25531 = CIRCLE ( 'NONE', #77761, 0.06509327318403745899 ) ;
#25532 = FACE_OUTER_BOUND ( 'NONE', #11559, .T. ) ;
#25533 = ORIENTED_EDGE ( 'NONE', *, *, #41248, .T. ) ;
#25534 = DIRECTION ( 'NONE',  ( 0.000000000000000000, 1.000000000000000000, 0.000000000000000000 ) ) ;
#25535 = CARTESIAN_POINT ( 'NONE',  ( 4.599999999999936584, 12.50000000000000000, 3.637306695894644726 ) ) ;
#25536 = DIRECTION ( 'NONE',  ( -0.000000000000000000, -1.000000000000000000, -0.000000000000000000 ) ) ;
#25537 = PLANE ( 'NONE',  #14878 ) ;
#25538 = CARTESIAN_POINT ( 'NONE',  ( -10.84999999999999964, 12.50000000000000000, 7.253104124594885960 ) ) ;
#25539 = VECTOR ( 'NONE', #114423, 1000.000000000000000 ) ;
#25540 = AXIS2_PLACEMENT_3D ( 'NONE', #10054, #20524, #21150 ) ;
#25541 = EDGE_LOOP ( 'NONE', ( #86981, #16145 ) ) ;
#25542 = DIRECTION ( 'NONE',  ( 0.000000000000000000, 0.000000000000000000, 1.000000000000000000 ) ) ;
#25543 = CIRCLE ( 'NONE', #2470, 0.06509327318403745899 ) ;
#25544 = ORIENTED_EDGE ( 'NONE', *, *, #114338, .F. ) ;
#25545 = ORIENTED_EDGE ( 'NONE', *, *, #58877, .T. ) ;
#25546 = EDGE_LOOP ( 'NONE', ( #113161, #60180, #78056, #19470 ) ) ;
#25547 = DIRECTION ( 'NONE',  ( -0.000000000000000000, 1.000000000000000000, -0.000000000000000000 ) ) ;
#25548 = FACE_BOUND ( 'NONE', #462, .T. ) ;
#25549 = CARTESIAN_POINT ( 'NONE',  ( -9.600000000000006750, 2.500000000000000000, -0.6928203230275542523 ) ) ;
#25551 = CONICAL_SURFACE ( 'NONE', #113300, 0.1000000000000002554, 0.003490658503988666988 ) ;
#25550 = DIRECTION ( 'NONE',  ( 0.000000000000000000, 0.000000000000000000, 1.000000000000000000 ) ) ;
#25553 = CARTESIAN_POINT ( 'NONE',  ( -1.650000000000034328, 2.500000000000000000, -2.165063509461101710 ) ) ;
#25552 = CONICAL_SURFACE ( 'NONE', #94521, 0.09999999999999982514, 0.003490658503988666988 ) ;
#25554 = ADVANCED_FACE ( 'NONE', ( #68095 ), #119990, .T. ) ;
#25555 = VECTOR ( 'NONE', #103421, 1000.000000000000000 ) ;
#25556 = AXIS2_PLACEMENT_3D ( 'NONE', #93603, #112608, #94893 ) ;
#25557 = AXIS2_PLACEMENT_3D ( 'NONE', #52510, #81970, #22437 ) ;
#25558 = ORIENTED_EDGE ( 'NONE', *, *, #55661, .F. ) ;
#25559 = DIRECTION ( 'NONE',  ( 0.000000000000000000, 0.000000000000000000, -1.000000000000000000 ) ) ;
#25560 = CARTESIAN_POINT ( 'NONE',  ( -9.350000000000004974, 2.500000000000000000, 6.048780366869521252 ) ) ;
#25561 = CARTESIAN_POINT ( 'NONE',  ( -3.750000000000027534, 2.500000000000000000, -1.372243186433550033 ) ) ;
#25562 = AXIS2_PLACEMENT_3D ( 'NONE', #26880, #43474, #53925 ) ;
#25563 = DIRECTION ( 'NONE',  ( 0.000000000000000000, 0.000000000000000000, -1.000000000000000000 ) ) ;
#25564 = ORIENTED_EDGE ( 'NONE', *, *, #44274, .F. ) ;
#25565 = EDGE_CURVE ( 'NONE', #2251, #27375, #99517, .T. ) ;
#25566 = DIRECTION ( 'NONE',  ( -4.274815082592931898E-19, -0.9999939076577903929, -0.003490651415223739937 ) ) ;
#25567 = CARTESIAN_POINT ( 'NONE',  ( -11.64999999999999858, 12.50000000000000000, -5.737276932171709198 ) ) ;
#25568 = ORIENTED_EDGE ( 'NONE', *, *, #88826, .T. ) ;
#25569 = EDGE_CURVE ( 'NONE', #26682, #32011, #109618, .T. ) ;
#25570 = LINE ( 'NONE', #83853, #14558 ) ;
#25571 = EDGE_CURVE ( 'NONE', #31935, #70505, #79855, .T. ) ;
#25572 = EDGE_LOOP ( 'NONE', ( #18150, #86791 ) ) ;
#25573 = FACE_BOUND ( 'NONE', #44562, .T. ) ;
#25574 = PLANE ( 'NONE',  #13757 ) ;
#25575 = ORIENTED_EDGE ( 'NONE', *, *, #100963, .F. ) ;
#25576 = CARTESIAN_POINT ( 'NONE',  ( 13.09999999999990195, 12.50000000000000000, 3.918623584224382839 ) ) ;
#25577 = FACE_OUTER_BOUND ( 'NONE', #16915, .T. ) ;
#25578 = EDGE_CURVE ( 'NONE', #11600, #3400, #108670, .T. ) ;
#25579 = VERTEX_POINT ( 'NONE', #98203 ) ;
#25580 = ORIENTED_EDGE ( 'NONE', *, *, #81347, .T. ) ;
#25581 = ADVANCED_FACE ( 'NONE', ( #109972 ), #58937, .T. ) ;
#25582 = CARTESIAN_POINT ( 'NONE',  ( 185.2552083336747444, 6.551208109652275624, -3.782341765624998686 ) ) ;
#25583 = VERTEX_POINT ( 'NONE', #128340 ) ;
#25584 = CARTESIAN_POINT ( 'NONE',  ( 185.6718750003414016, 9.264065473108010111E-16, -7.564683531250000925 ) ) ;
#25585 = CARTESIAN_POINT ( 'NONE',  ( 8.299999999999922551, 12.50000000000000000, 4.330127018922196314 ) ) ;
#25586 = VECTOR ( 'NONE', #108333, 1000.000000000000000 ) ;
#25587 = CARTESIAN_POINT ( 'NONE',  ( -7.500000000000015099, 2.500000000000000000, -0.7928203230275542301 ) ) ;
#25588 = DIRECTION ( 'NONE',  ( -0.000000000000000000, 1.000000000000000000, -0.000000000000000000 ) ) ;
#25589 = CONICAL_SURFACE ( 'NONE', #121744, 0.1000000000000002554, 0.003490658503988666988 ) ;
#25590 = CARTESIAN_POINT ( 'NONE',  ( 1.049999999999954969, 2.500000000000000000, -6.841600689897077814 ) ) ;
#25591 = AXIS2_PLACEMENT_3D ( 'NONE', #26164, #24228, #24872 ) ;
#25593 = ORIENTED_EDGE ( 'NONE', *, *, #23377, .F. ) ;
#25592 = CIRCLE ( 'NONE', #17266, 0.1000000000000002554 ) ;
#25595 = EDGE_LOOP ( 'NONE', ( #105701, #79915 ) ) ;
#25594 = AXIS2_PLACEMENT_3D ( 'NONE', #32764, #115129, #27405 ) ;
#25596 = DIRECTION ( 'NONE',  ( 0.000000000000000000, -0.000000000000000000, 1.000000000000000000 ) ) ;
#25597 = CARTESIAN_POINT ( 'NONE',  ( -1.650000000000035216, 12.50000000000000000, -1.537336459617587581 ) ) ;
#25598 = CARTESIAN_POINT ( 'NONE',  ( -10.84999999999999964, 12.50000000000000000, 2.857883832488649301 ) ) ;
#25599 = CONICAL_SURFACE ( 'NONE', #52805, 0.1000000000000002554, 0.003490658503988666988 ) ;
#25600 = DIRECTION ( 'NONE',  ( 0.000000000000000000, 1.000000000000000000, 0.000000000000000000 ) ) ;
#25603 = ORIENTED_EDGE ( 'NONE', *, *, #45848, .T. ) ;
#25602 = ORIENTED_EDGE ( 'NONE', *, *, #2874, .F. ) ;
#25601 = CIRCLE ( 'NONE', #63187, 2.000000000000000000 ) ;
#25604 = FACE_BOUND ( 'NONE', #84333, .T. ) ;
#25605 = ORIENTED_EDGE ( 'NONE', *, *, #45859, .F. ) ;
#25606 = CARTESIAN_POINT ( 'NONE',  ( 1.249999999999950262, 2.500000000000000000, 7.188010851410848723 ) ) ;
#25607 = CARTESIAN_POINT ( 'NONE',  ( 3.299999999999942979, 2.500000000000000000, 4.430127018922196847 ) ) ;
#25608 = CONICAL_SURFACE ( 'NONE', #2623, 0.1000000000000002554, 0.003490658503988666988 ) ;
#25609 = EDGE_LOOP ( 'NONE', ( #100697, #63484, #35620, #93159 ) ) ;
#25610 = CARTESIAN_POINT ( 'NONE',  ( 3.349999999999945466, 12.50000000000000000, -7.122917578226816815 ) ) ;
#25611 = CARTESIAN_POINT ( 'NONE',  ( 9.349999999999916156, 2.500000000000000000, -2.411473670974877859 ) ) ;
#25612 = ADVANCED_FACE ( 'NONE', ( #9828 ), #51046, .T. ) ;
#25613 = DIRECTION ( 'NONE',  ( -0.000000000000000000, 1.000000000000000000, -0.000000000000000000 ) ) ;
#25614 = DIRECTION ( 'NONE',  ( 0.000000000000000000, 0.000000000000000000, -1.000000000000000000 ) ) ;
#25615 = CYLINDRICAL_SURFACE ( 'NONE', #7959, 7.700000000000000178 ) ;
#25616 = CARTESIAN_POINT ( 'NONE',  ( 10.84999999999990905, 12.50000000000000000, 2.857883832488649301 ) ) ;
#25617 = CARTESIAN_POINT ( 'NONE',  ( 186.4010416670080588, -4.367472073101520635, 7.564683531249999149 ) ) ;
#25618 = CARTESIAN_POINT ( 'NONE',  ( -0.6500000000000398792, 2.500000000000000000, -2.411473670974877859 ) ) ;
#25619 = EDGE_CURVE ( 'NONE', #5316, #76556, #39947, .T. ) ;
#25620 = DIRECTION ( 'NONE',  ( 0.000000000000000000, 0.000000000000000000, -1.000000000000000000 ) ) ;
#25621 = EDGE_CURVE ( 'NONE', #12513, #100762, #8520, .T. ) ;
#25622 = AXIS2_PLACEMENT_3D ( 'NONE', #111538, #50065, #20585 ) ;
#25623 = EDGE_LOOP ( 'NONE', ( #607, #23291, #52235, #56564 ) ) ;
#25624 = VERTEX_POINT ( 'NONE', #38672 ) ;
#25625 = PLANE ( 'NONE',  #109781 ) ;
#25626 = ORIENTED_EDGE ( 'NONE', *, *, #65456, .F. ) ;
#25627 = CARTESIAN_POINT ( 'NONE',  ( 0.8499999999999557909, 2.500000000000000000, -6.495190528383302464 ) ) ;
#25628 = ADVANCED_FACE ( 'NONE', ( #78595 ), #67746, .T. ) ;
#25630 = VERTEX_POINT ( 'NONE', #87731 ) ;
#25629 = ORIENTED_EDGE ( 'NONE', *, *, #4711, .F. ) ;
#25631 = EDGE_LOOP ( 'NONE', ( #72058, #125956, #33563, #75623 ) ) ;
#25632 = EDGE_CURVE ( 'NONE', #40733, #34370, #37999, .T. ) ;
#25633 = FACE_OUTER_BOUND ( 'NONE', #101238, .T. ) ;
#25634 = ADVANCED_FACE ( 'NONE', ( #117829 ), #55237, .T. ) ;
#25635 = CIRCLE ( 'NONE', #82077, 0.06509327318403745899 ) ;
#25636 = AXIS2_PLACEMENT_3D ( 'NONE', #112713, #11276, #51231 ) ;
#25637 = DIRECTION ( 'NONE',  ( -0.000000000000000000, -1.000000000000000000, -0.000000000000000000 ) ) ;
#25638 = FILL_AREA_STYLE_COLOUR ( '', #10014 ) ;
#25639 = EDGE_CURVE ( 'NONE', #44247, #77073, #59607, .T. ) ;
#25640 = CARTESIAN_POINT ( 'NONE',  ( 4.999999999999936939, 2.500000000000000000, -0.6928203230275541413 ) ) ;
#25641 = DIRECTION ( 'NONE',  ( -0.000000000000000000, -1.000000000000000000, -0.000000000000000000 ) ) ;
#25642 = DIRECTION ( 'NONE',  ( -0.000000000000000000, -1.000000000000000000, -0.000000000000000000 ) ) ;
#25643 = EDGE_LOOP ( 'NONE', ( #109873, #39207, #110527, #87151 ) ) ;
#25644 = CIRCLE ( 'NONE', #98800, 0.06509327318403745899 ) ;
#25645 = CONICAL_SURFACE ( 'NONE', #105056, 0.09999999999999982514, 0.003490658503988666988 ) ;
#25647 = EDGE_CURVE ( 'NONE', #86071, #33663, #28188, .T. ) ;
#25646 = DIRECTION ( 'NONE',  ( 0.000000000000000000, -0.9999939076577903929, 0.003490651415223739937 ) ) ;
#25648 = ORIENTED_EDGE ( 'NONE', *, *, #76774, .T. ) ;
#25649 = AXIS2_PLACEMENT_3D ( 'NONE', #78007, #100232, #17787 ) ;
#25650 = ADVANCED_FACE ( 'NONE', ( #2 ), #67838, .T. ) ;
#25651 = ORIENTED_EDGE ( 'NONE', *, *, #120409, .T. ) ;
#25652 = ORIENTED_EDGE ( 'NONE', *, *, #54698, .T. ) ;
#25653 = VECTOR ( 'NONE', #39580, 1000.000000000000000 ) ;
#25654 = ORIENTED_EDGE ( 'NONE', *, *, #32747, .F. ) ;
#25655 = DIRECTION ( 'NONE',  ( -0.000000000000000000, -1.000000000000000000, -0.000000000000000000 ) ) ;
#25656 = ORIENTED_EDGE ( 'NONE', *, *, #34966, .T. ) ;
#25657 = ORIENTED_EDGE ( 'NONE', *, *, #58471, .F. ) ;
#25658 = AXIS2_PLACEMENT_3D ( 'NONE', #7203, #37343, #25550 ) ;
#25659 = CARTESIAN_POINT ( 'NONE',  ( -0.4000000000000392131, 12.50000000000000000, -5.022947341949754119 ) ) ;
#25660 = AXIS2_PLACEMENT_3D ( 'NONE', #109966, #99505, #20287 ) ;
#25661 = CARTESIAN_POINT ( 'NONE',  ( -4.200000000000025935, 12.50000000000000000, -2.385244779468109755E-15 ) ) ;
#25662 = DIRECTION ( 'NONE',  ( 0.000000000000000000, 1.000000000000000000, 0.000000000000000000 ) ) ;
#25663 = DIRECTION ( 'NONE',  ( 0.000000000000000000, -0.000000000000000000, 1.000000000000000000 ) ) ;
#25664 = AXIS2_PLACEMENT_3D ( 'NONE', #52878, #103271, #51600 ) ;
#25665 = DIRECTION ( 'NONE',  ( 0.000000000000000000, 0.000000000000000000, 1.000000000000000000 ) ) ;
#25666 = VECTOR ( 'NONE', #31801, 1000.000000000000000 ) ;
#25667 = CONICAL_SURFACE ( 'NONE', #27718, 0.09999999999999982514, 0.003490658503988666988 ) ;
#25668 = CARTESIAN_POINT ( 'NONE',  ( 7.499999999999961808, 2.500000000000000000, -4.330127018922201643 ) ) ;
#25669 = ORIENTED_EDGE ( 'NONE', *, *, #72932, .T. ) ;
#25670 = AXIS2_PLACEMENT_3D ( 'NONE', #14311, #4479, #52970 ) ;
#25671 = DIRECTION ( 'NONE',  ( 0.000000000000000000, 0.000000000000000000, 1.000000000000000000 ) ) ;
#25672 = ORIENTED_EDGE ( 'NONE', *, *, #97314, .T. ) ;
#25673 = CARTESIAN_POINT ( 'NONE',  ( -12.89999999999999147, 12.50000000000000000, -5.088040615133788691 ) ) ;
#25674 = ORIENTED_EDGE ( 'NONE', *, *, #41010, .F. ) ;
#25675 = AXIS2_PLACEMENT_3D ( 'NONE', #72481, #120922, #62017 ) ;
#25676 = CARTESIAN_POINT ( 'NONE',  ( -6.900000000000019007, 2.500000000000000000, -3.983716857408426293 ) ) ;
#25677 = VERTEX_POINT ( 'NONE', #10466 ) ;
#25678 = ORIENTED_EDGE ( 'NONE', *, *, #55526, .F. ) ;
#25679 = LINE ( 'NONE', #65607, #72083 ) ;
#25680 = PLANE ( 'NONE',  #111220 ) ;
#25681 = DIRECTION ( 'NONE',  ( -0.000000000000000000, 1.000000000000000000, -0.000000000000000000 ) ) ;
#25682 = FACE_OUTER_BOUND ( 'NONE', #121917, .T. ) ;
#25683 = LINE ( 'NONE', #65611, #72153 ) ;
#25684 = ORIENTED_EDGE ( 'NONE', *, *, #123105, .T. ) ;
#25685 = CARTESIAN_POINT ( 'NONE',  ( -2.300000000000032685, 2.500000000000000000, -4.676537180435978769 ) ) ;
#25687 = AXIS2_PLACEMENT_3D ( 'NONE', #93597, #22304, #3923 ) ;
#25686 = DIRECTION ( 'NONE',  ( -0.000000000000000000, -1.000000000000000000, -0.000000000000000000 ) ) ;
#25688 = AXIS2_PLACEMENT_3D ( 'NONE', #123712, #62888, #102790 ) ;
#25689 = CARTESIAN_POINT ( 'NONE',  ( -0.4500000000000397571, 2.500000000000000000, -2.165063509461101710 ) ) ;
#25690 = DIRECTION ( 'NONE',  ( 0.000000000000000000, 1.000000000000000000, 0.000000000000000000 ) ) ;
#25692 = EDGE_CURVE ( 'NONE', #104247, #63955, #127043, .T. ) ;
#25691 = CARTESIAN_POINT ( 'NONE',  ( 6.449999999999931788, 2.500000000000000000, -2.611473670974877592 ) ) ;
#25693 = ORIENTED_EDGE ( 'NONE', *, *, #22473, .T. ) ;
#25694 = AXIS2_PLACEMENT_3D ( 'NONE', #4430, #34597, #15558 ) ;
#25695 = AXIS2_PLACEMENT_3D ( 'NONE', #37994, #38668, #97555 ) ;
#25696 = ORIENTED_EDGE ( 'NONE', *, *, #92089, .T. ) ;
#25697 = AXIS2_PLACEMENT_3D ( 'NONE', #61390, #101954, #52853 ) ;
#25698 = AXIS2_PLACEMENT_3D ( 'NONE', #25850, #34400, #74949 ) ;
#25699 = UNCERTAINTY_MEASURE_WITH_UNIT (LENGTH_MEASURE( 1.000000000000000082E-05 ), #30989, 'distance_accuracy_value', 'NONE');
#25700 = EDGE_LOOP ( 'NONE', ( #69401, #53825 ) ) ;
#25701 = FACE_OUTER_BOUND ( 'NONE', #15688, .T. ) ;
#25702 = CARTESIAN_POINT ( 'NONE',  ( -3.749999999999991562, 2.500000000000000000, 6.495190528383297135 ) ) ;
#25703 = AXIS2_PLACEMENT_3D ( 'NONE', #127768, #10554, #37476 ) ;
#25704 = AXIS2_PLACEMENT_3D ( 'NONE', #84299, #5084, #47609 ) ;
#25705 = CONICAL_SURFACE ( 'NONE', #67435, 0.1000000000000002554, 0.003490658503988666988 ) ;
#25706 = CIRCLE ( 'NONE', #90552, 0.09999999999999982514 ) ;
#25707 = CARTESIAN_POINT ( 'NONE',  ( 187.4166666666666856, 6.668395609140176816, 3.850000000000000977 ) ) ;
#25708 = DIRECTION ( 'NONE',  ( 0.000000000000000000, -0.9999939076577903929, 0.003490651415223739937 ) ) ;
#25709 = DIRECTION ( 'NONE',  ( 0.000000000000000000, 0.000000000000000000, -1.000000000000000000 ) ) ;
#25710 = DIRECTION ( 'NONE',  ( 0.000000000000000000, 0.000000000000000000, 1.000000000000000000 ) ) ;
#25711 = DIRECTION ( 'NONE',  ( 0.000000000000000000, 0.000000000000000000, 1.000000000000000000 ) ) ;
#25712 = ORIENTED_EDGE ( 'NONE', *, *, #40603, .F. ) ;
#25713 = AXIS2_PLACEMENT_3D ( 'NONE', #101198, #111663, #22011 ) ;
#25714 = FACE_OUTER_BOUND ( 'NONE', #117038, .T. ) ;
#25715 = DIRECTION ( 'NONE',  ( 1.000000000000000000, 0.000000000000000000, 0.000000000000000000 ) ) ;
#25716 = EDGE_LOOP ( 'NONE', ( #30370, #72122, #42758, #22758 ) ) ;
#25717 = DIRECTION ( 'NONE',  ( 1.000000000000000000, 0.000000000000000000, 0.000000000000000000 ) ) ;
#25718 = LINE ( 'NONE', #95117, #129206 ) ;
#25719 = DIRECTION ( 'NONE',  ( -0.000000000000000000, 1.000000000000000000, -0.000000000000000000 ) ) ;
#25720 = CIRCLE ( 'NONE', #124016, 0.09999999999999982514 ) ;
#25721 = ORIENTED_EDGE ( 'NONE', *, *, #34709, .F. ) ;
#25722 = CARTESIAN_POINT ( 'NONE',  ( -10.65000000000000391, 2.500000000000000000, -6.741600689897074616 ) ) ;
#25723 = ORIENTED_EDGE ( 'NONE', *, *, #126486, .F. ) ;
#25724 = CARTESIAN_POINT ( 'NONE',  ( 0.4499999999999569344, 2.500000000000000000, 2.165063509461097713 ) ) ;
#25725 = DIRECTION ( 'NONE',  ( 0.000000000000000000, 0.000000000000000000, 1.000000000000000000 ) ) ;
#25726 = CONICAL_SURFACE ( 'NONE', #88417, 0.1000000000000000472, 0.003490658503988666988 ) ;
#25727 = ORIENTED_EDGE ( 'NONE', *, *, #79414, .T. ) ;
#25728 = CONICAL_SURFACE ( 'NONE', #67576, 0.09999999999999982514, 0.003490658503988666988 ) ;
#25729 = ADVANCED_FACE ( 'NONE', ( #51699 ), #34418, .T. ) ;
#25730 = AXIS2_PLACEMENT_3D ( 'NONE', #79238, #89050, #99526 ) ;
#25731 = DIRECTION ( 'NONE',  ( 0.000000000000000000, -0.9999939076577903929, 0.003490651415223739937 ) ) ;
#25732 = FACE_OUTER_BOUND ( 'NONE', #76129, .T. ) ;
#25733 = ADVANCED_FACE ( 'NONE', ( #112555 ), #120432, .T. ) ;
#25734 = AXIS2_PLACEMENT_3D ( 'NONE', #84505, #99798, #120087 ) ;
#25735 = ADVANCED_FACE ( 'NONE', ( #32718 ), #121708, .T. ) ;
#25736 = ORIENTED_EDGE ( 'NONE', *, *, #32348, .F. ) ;
#25737 = VECTOR ( 'NONE', #41149, 1000.000000000000000 ) ;
#25738 = LINE ( 'NONE', #65659, #26497 ) ;
#25739 = CIRCLE ( 'NONE', #4796, 0.1000000000000000472 ) ;
#25740 = AXIS2_PLACEMENT_3D ( 'NONE', #23784, #13942, #63056 ) ;
#25741 = ORIENTED_EDGE ( 'NONE', *, *, #43845, .F. ) ;
#25742 = VERTEX_POINT ( 'NONE', #91611 ) ;
#25743 = CARTESIAN_POINT ( 'NONE',  ( -10.60000000000000142, 12.50000000000000000, 4.676537180435972552 ) ) ;
#25744 = LINE ( 'NONE', #105610, #24930 ) ;
#25745 = EDGE_CURVE ( 'NONE', #65132, #127833, #70000, .T. ) ;
#25746 = EDGE_CURVE ( 'NONE', #68456, #58840, #60863, .T. ) ;
#25747 = VERTEX_POINT ( 'NONE', #50393 ) ;
#25748 = EDGE_CURVE ( 'NONE', #111170, #9181, #128510, .T. ) ;
#25749 = DIRECTION ( 'NONE',  ( -0.000000000000000000, -1.000000000000000000, -0.000000000000000000 ) ) ;
#25750 = CARTESIAN_POINT ( 'NONE',  ( -0.8000000000000376810, 12.50000000000000000, -4.395220292106239768 ) ) ;
#25751 = AXIS2_PLACEMENT_3D ( 'NONE', #119588, #9648, #28658 ) ;
#25752 = ORIENTED_EDGE ( 'NONE', *, *, #57138, .F. ) ;
#25753 = DIRECTION ( 'NONE',  ( 0.000000000000000000, -0.000000000000000000, 1.000000000000000000 ) ) ;
#25754 = CARTESIAN_POINT ( 'NONE',  ( 4.549999999999937650, 2.500000000000000000, 2.065063509461097624 ) ) ;
#25755 = AXIS2_PLACEMENT_3D ( 'NONE', #10732, #57942, #97844 ) ;
#25756 = CONICAL_SURFACE ( 'NONE', #6949, 0.09999999999999999167, 0.003490658503988666988 ) ;
#25757 = AXIS2_PLACEMENT_3D ( 'NONE', #49004, #128197, #99385 ) ;
#25758 = CARTESIAN_POINT ( 'NONE',  ( -4.600000000000025402, 12.50000000000000000, -2.385244779468109755E-15 ) ) ;
#25759 = DIRECTION ( 'NONE',  ( 0.000000000000000000, 0.000000000000000000, -1.000000000000000000 ) ) ;
#25760 = CARTESIAN_POINT ( 'NONE',  ( -12.94999999999999218, 2.500000000000000000, -2.065063509461099844 ) ) ;
#25761 = AXIS2_PLACEMENT_3D ( 'NONE', #55392, #14782, #54729 ) ;
#25762 = DIRECTION ( 'NONE',  ( 0.000000000000000000, 0.000000000000000000, -1.000000000000000000 ) ) ;
#25763 = ORIENTED_EDGE ( 'NONE', *, *, #101964, .F. ) ;
#25764 = CIRCLE ( 'NONE', #48768, 0.09999999999999982514 ) ;
#25765 = ORIENTED_EDGE ( 'NONE', *, *, #111671, .F. ) ;
#25766 = EDGE_LOOP ( 'NONE', ( #102469, #90224 ) ) ;
#25767 = ORIENTED_EDGE ( 'NONE', *, *, #52100, .F. ) ;
#25768 = DIRECTION ( 'NONE',  ( -0.000000000000000000, 1.000000000000000000, -0.000000000000000000 ) ) ;
#25769 = DIRECTION ( 'NONE',  ( 0.000000000000000000, 0.000000000000000000, 1.000000000000000000 ) ) ;
#25770 = CARTESIAN_POINT ( 'NONE',  ( 11.64999999999990798, 2.500000000000000000, 5.902370205355745192 ) ) ;
#25771 = ORIENTED_EDGE ( 'NONE', *, *, #59049, .F. ) ;
#25772 = FACE_BOUND ( 'NONE', #83413, .T. ) ;
#25773 = DIRECTION ( 'NONE',  ( 0.000000000000000000, -0.000000000000000000, 1.000000000000000000 ) ) ;
#25774 = CARTESIAN_POINT ( 'NONE',  ( 9.799999999999917222, 12.50000000000000000, 0.3464101615137735735 ) ) ;
#25775 = PLANE ( 'NONE',  #59656 ) ;
#25776 = PLANE ( 'NONE',  #53419 ) ;
#25777 = DIRECTION ( 'NONE',  ( 0.000000000000000000, 1.000000000000000000, 0.000000000000000000 ) ) ;
#25778 = CARTESIAN_POINT ( 'NONE',  ( -13.34999999999999076, 2.500000000000000000, -2.957883832488651610 ) ) ;
#25779 = DIRECTION ( 'NONE',  ( -0.000000000000000000, -1.000000000000000000, -0.000000000000000000 ) ) ;
#25780 = CARTESIAN_POINT ( 'NONE',  ( -3.150000000000030109, 12.50000000000000000, 1.818653347947321475 ) ) ;
#25781 = CIRCLE ( 'NONE', #23740, 0.06509327318403745899 ) ;
#25782 = CIRCLE ( 'NONE', #735, 0.1000000000000002554 ) ;
#25783 = LINE ( 'NONE', #126573, #64111 ) ;
#25784 = DIRECTION ( 'NONE',  ( 0.000000000000000000, 0.000000000000000000, -1.000000000000000000 ) ) ;
#25785 = CIRCLE ( 'NONE', #9060, 7.500000000000000000 ) ;
#25786 = EDGE_LOOP ( 'NONE', ( #52745, #98241, #75770, #63968 ) ) ;
#25787 = ORIENTED_EDGE ( 'NONE', *, *, #41630, .F. ) ;
#25788 = EDGE_LOOP ( 'NONE', ( #107932, #40914 ) ) ;
#25789 = CONICAL_SURFACE ( 'NONE', #69705, 0.09999999999999999167, 0.003490658503988666988 ) ;
#25790 = ORIENTED_EDGE ( 'NONE', *, *, #56724, .F. ) ;
#25792 = CONICAL_SURFACE ( 'NONE', #113621, 0.1000000000000002554, 0.003490658503988666988 ) ;
#25791 = CARTESIAN_POINT ( 'NONE',  ( -9.550000000000007816, 12.50000000000000000, -6.560283801567334372 ) ) ;
#25793 = ORIENTED_EDGE ( 'NONE', *, *, #9634, .F. ) ;
#25795 = ADVANCED_FACE ( 'NONE', ( #71986 ), #643, .T. ) ;
#25794 = CIRCLE ( 'NONE', #59266, 0.09999999999999982514 ) ;
#25796 = DIRECTION ( 'NONE',  ( 0.000000000000000000, 1.000000000000000000, 0.000000000000000000 ) ) ;
#25797 = EDGE_CURVE ( 'NONE', #70661, #81572, #73259, .T. ) ;
#25798 = EDGE_LOOP ( 'NONE', ( #107764, #42117 ) ) ;
#25799 = VERTEX_POINT ( 'NONE', #81776 ) ;
#25800 = EDGE_CURVE ( 'NONE', #26024, #48610, #111903, .T. ) ;
#25801 = DIRECTION ( 'NONE',  ( -4.274815082592931898E-19, -0.9999939076577903929, -0.003490651415223739937 ) ) ;
#25802 = AXIS2_PLACEMENT_3D ( 'NONE', #43917, #64821, #64179 ) ;
#25803 = AXIS2_PLACEMENT_3D ( 'NONE', #40806, #89872, #30988 ) ;
#25804 = AXIS2_PLACEMENT_3D ( 'NONE', #99763, #120045, #67704 ) ;
#25805 = DIRECTION ( 'NONE',  ( 0.000000000000000000, -0.9999939076577903929, 0.003490651415223739937 ) ) ;
#25806 = CARTESIAN_POINT ( 'NONE',  ( 8.549999999999920774, 2.500000000000000000, 6.148780366869520897 ) ) ;
#25807 = LINE ( 'NONE', #53345, #101156 ) ;
#25808 = EDGE_CURVE ( 'NONE', #79392, #72341, #62170, .T. ) ;
#25809 = CARTESIAN_POINT ( 'NONE',  ( -5.000000000000026645, 2.500000000000000000, -3.737306695894649700 ) ) ;
#25810 = CIRCLE ( 'NONE', #67547, 0.06509327318403745899 ) ;
#25811 = ADVANCED_FACE ( 'NONE', ( #21583 ), #113818, .T. ) ;
#25812 = ORIENTED_EDGE ( 'NONE', *, *, #10716, .T. ) ;
#25813 = EDGE_CURVE ( 'NONE', #128257, #32927, #81158, .T. ) ;
#25814 = EDGE_CURVE ( 'NONE', #17144, #2782, #72065, .T. ) ;
#25815 = EDGE_LOOP ( 'NONE', ( #119977, #42147 ) ) ;
#25816 = ADVANCED_FACE ( 'NONE', ( #52330 ), #84570, .T. ) ;
#25817 = ORIENTED_EDGE ( 'NONE', *, *, #88142, .T. ) ;
#25818 = ORIENTED_EDGE ( 'NONE', *, *, #48110, .F. ) ;
#25819 = DIRECTION ( 'NONE',  ( 0.000000000000000000, -0.000000000000000000, 1.000000000000000000 ) ) ;
#25820 = ORIENTED_EDGE ( 'NONE', *, *, #5782, .T. ) ;
#25821 = ORIENTED_EDGE ( 'NONE', *, *, #68680, .F. ) ;
#25822 = ADVANCED_FACE ( 'NONE', ( #13026 ), #3240, .T. ) ;
#25823 = AXIS2_PLACEMENT_3D ( 'NONE', #80645, #79985, #120559 ) ;
#25824 = DIRECTION ( 'NONE',  ( -0.000000000000000000, -1.000000000000000000, -0.000000000000000000 ) ) ;
#25825 = DIRECTION ( 'NONE',  ( 0.000000000000000000, 1.000000000000000000, 0.000000000000000000 ) ) ;
#25826 = CARTESIAN_POINT ( 'NONE',  ( 10.84999999999990905, 2.500000000000000000, -6.595190528383302109 ) ) ;
#25827 = CARTESIAN_POINT ( 'NONE',  ( 0.000000000000000000, -5.000000000000000000, 0.000000000000000000 ) ) ;
#25828 = CARTESIAN_POINT ( 'NONE',  ( -4.400000000000028777, 12.50000000000000000, -4.611443907251940644 ) ) ;
#25829 = CARTESIAN_POINT ( 'NONE',  ( -11.64999999999999680, 12.50000000000000000, -7.253104124594887736 ) ) ;
#25831 = ORIENTED_EDGE ( 'NONE', *, *, #7992, .T. ) ;
#25830 = VECTOR ( 'NONE', #33305, 1000.000000000000000 ) ;
#25832 = CARTESIAN_POINT ( 'NONE',  ( 4.999999999999969802, 2.500000000000000000, 4.430127018922196847 ) ) ;
#25833 = CIRCLE ( 'NONE', #7022, 0.1000000000000002554 ) ;
#25834 = VECTOR ( 'NONE', #123443, 1000.000000000000000 ) ;
#25835 = ORIENTED_EDGE ( 'NONE', *, *, #100237, .F. ) ;
#25836 = DIRECTION ( 'NONE',  ( -0.000000000000000000, -1.000000000000000000, -0.000000000000000000 ) ) ;
#25837 = ORIENTED_EDGE ( 'NONE', *, *, #89150, .F. ) ;
#25838 = PLANE ( 'NONE',  #118404 ) ;
#25839 = DIRECTION ( 'NONE',  ( 0.000000000000000000, 0.000000000000000000, 1.000000000000000000 ) ) ;
#25840 = ADVANCED_BREP_SHAPE_REPRESENTATION ( '', ( #12695, #108296 ), #37304 ) ;
#25841 = EDGE_LOOP ( 'NONE', ( #81665, #81822, #110232, #60754 ) ) ;
#25842 = DIRECTION ( 'NONE',  ( -0.000000000000000000, 1.000000000000000000, -0.000000000000000000 ) ) ;
#25844 = AXIS2_PLACEMENT_3D ( 'NONE', #54247, #122990, #3849 ) ;
#25843 = DIRECTION ( 'NONE',  ( 0.000000000000000000, -0.9999939076577903929, 0.003490651415223739937 ) ) ;
#25845 = EDGE_LOOP ( 'NONE', ( #43217, #24510, #104370, #106616 ) ) ;
#25846 = AXIS2_PLACEMENT_3D ( 'NONE', #27274, #107116, #27926 ) ;
#25847 = VECTOR ( 'NONE', #116260, 1000.000000000000000 ) ;
#25848 = DIRECTION ( 'NONE',  ( -0.000000000000000000, 1.000000000000000000, -0.000000000000000000 ) ) ;
#25849 = CONICAL_SURFACE ( 'NONE', #21645, 0.1000000000000002554, 0.003490658503988666988 ) ;
#25850 = CARTESIAN_POINT ( 'NONE',  ( 7.899999999999923084, 12.50000000000000000, 0.6928203230275494784 ) ) ;
#25851 = ORIENTED_EDGE ( 'NONE', *, *, #57412, .T. ) ;
#25852 = EDGE_LOOP ( 'NONE', ( #55668, #46008, #90553, #95466 ) ) ;
#25853 = CARTESIAN_POINT ( 'NONE',  ( 10.64999999999990976, 12.50000000000000000, 2.511473670974873507 ) ) ;
#25854 = DIRECTION ( 'NONE',  ( 1.000000000000000000, 0.000000000000000000, 0.000000000000000000 ) ) ;
#25855 = CARTESIAN_POINT ( 'NONE',  ( 187.4218750003414016, 0.000000000000000000, 7.564683531250000925 ) ) ;
#25856 = VECTOR ( 'NONE', #14805, 1000.000000000000000 ) ;
#25857 = DIRECTION ( 'NONE',  ( -0.000000000000000000, -1.000000000000000000, -0.000000000000000000 ) ) ;
#25859 = EDGE_CURVE ( 'NONE', #109438, #49236, #123013, .T. ) ;
#25858 = CARTESIAN_POINT ( 'NONE',  ( -10.60000000000000142, 2.500000000000000000, 4.776537180435972196 ) ) ;
#25860 = AXIS2_PLACEMENT_3D ( 'NONE', #79234, #89686, #48474 ) ;
#25861 = AXIS2_PLACEMENT_3D ( 'NONE', #25301, #83612, #54772 ) ;
#25862 = DIRECTION ( 'NONE',  ( -4.274815082592931898E-19, -0.9999939076577903929, -0.003490651415223739937 ) ) ;
#25863 = CIRCLE ( 'NONE', #107331, 0.09999999999999999167 ) ;
#25864 = ORIENTED_EDGE ( 'NONE', *, *, #99936, .F. ) ;
#25865 = CONICAL_SURFACE ( 'NONE', #73982, 0.1000000000000002554, 0.003490658503988666988 ) ;
#25866 = CARTESIAN_POINT ( 'NONE',  ( 43.31345875132075918, 2.029331038885034744, -5.113051027236704016 ) ) ;
#25867 = ORIENTED_EDGE ( 'NONE', *, *, #42941, .T. ) ;
#25868 = ADVANCED_FACE ( 'NONE', ( #3871 ), #53624, .T. ) ;
#25869 = CARTESIAN_POINT ( 'NONE',  ( 13.34999999999990017, 12.50000000000000000, 2.230156782645134950 ) ) ;
#25870 = DIRECTION ( 'NONE',  ( 0.000000000000000000, 1.000000000000000000, 0.000000000000000000 ) ) ;
#25871 = CARTESIAN_POINT ( 'NONE',  ( -4.400000000000025224, 12.50000000000000000, 4.676537180435972552 ) ) ;
#25872 = VERTEX_POINT ( 'NONE', #116393 ) ;
#25873 = DIRECTION ( 'NONE',  ( -0.000000000000000000, -1.000000000000000000, -0.000000000000000000 ) ) ;
#25874 = DIRECTION ( 'NONE',  ( 0.000000000000000000, 0.000000000000000000, -1.000000000000000000 ) ) ;
#25875 = AXIS2_PLACEMENT_3D ( 'NONE', #40504, #30680, #70581 ) ;
#25876 = CIRCLE ( 'NONE', #13338, 0.09999999999999982514 ) ;
#25877 = VERTEX_POINT ( 'NONE', #125567 ) ;
#25878 = DIRECTION ( 'NONE',  ( -0.000000000000000000, -1.000000000000000000, -0.000000000000000000 ) ) ;
#25879 = AXIS2_PLACEMENT_3D ( 'NONE', #86733, #46161, #57281 ) ;
#25880 = VECTOR ( 'NONE', #28594, 1000.000000000000000 ) ;
#25881 = ORIENTED_EDGE ( 'NONE', *, *, #16942, .T. ) ;
#25882 = CIRCLE ( 'NONE', #96986, 0.1000000000000002554 ) ;
#25883 = ORIENTED_EDGE ( 'NONE', *, *, #68527, .F. ) ;
#25884 = DIRECTION ( 'NONE',  ( 0.000000000000000000, 1.000000000000000000, 0.000000000000000000 ) ) ;
#25885 = CIRCLE ( 'NONE', #2907, 0.06509327318403745899 ) ;
#25886 = AXIS2_PLACEMENT_3D ( 'NONE', #28272, #68180, #28929 ) ;
#25887 = ORIENTED_EDGE ( 'NONE', *, *, #31431, .T. ) ;
#25888 = DIRECTION ( 'NONE',  ( -4.274815082592931898E-19, -0.9999939076577903929, -0.003490651415223739937 ) ) ;
#25889 = DIRECTION ( 'NONE',  ( 0.000000000000000000, 0.000000000000000000, 1.000000000000000000 ) ) ;
#25890 = DIRECTION ( 'NONE',  ( 0.000000000000000000, 0.000000000000000000, 1.000000000000000000 ) ) ;
#25892 = ORIENTED_EDGE ( 'NONE', *, *, #25982, .F. ) ;
#25891 = CIRCLE ( 'NONE', #78227, 0.1000000000000002554 ) ;
#25893 = AXIS2_PLACEMENT_3D ( 'NONE', #16311, #15670, #125000 ) ;
#25895 = EDGE_CURVE ( 'NONE', #38108, #114128, #111759, .T. ) ;
#25894 = CONICAL_SURFACE ( 'NONE', #42646, 0.09999999999999999167, 0.003490658503988666988 ) ;
#25896 = FACE_BOUND ( 'NONE', #40108, .T. ) ;
#25898 = VERTEX_POINT ( 'NONE', #36583 ) ;
#25897 = DIRECTION ( 'NONE',  ( -0.000000000000000000, 1.000000000000000000, -0.000000000000000000 ) ) ;
#25899 = CIRCLE ( 'NONE', #53089, 0.06509327318403745899 ) ;
#25900 = LINE ( 'NONE', #75001, #500 ) ;
#25901 = LINE ( 'NONE', #65809, #119919 ) ;
#25902 = EDGE_CURVE ( 'NONE', #44383, #89842, #88776, .T. ) ;
#25903 = EDGE_LOOP ( 'NONE', ( #22178, #74515, #64398, #1244 ) ) ;
#25904 = EDGE_LOOP ( 'NONE', ( #88407, #28266 ) ) ;
#25905 = ORIENTED_EDGE ( 'NONE', *, *, #66933, .F. ) ;
#25906 = DIRECTION ( 'NONE',  ( -0.000000000000000000, -1.000000000000000000, -0.000000000000000000 ) ) ;
#25907 = FACE_OUTER_BOUND ( 'NONE', #87911, .T. ) ;
#25908 = EDGE_CURVE ( 'NONE', #60793, #7675, #118005, .T. ) ;
#25909 = EDGE_CURVE ( 'NONE', #55580, #115142, #9349, .T. ) ;
#25910 = DIRECTION ( 'NONE',  ( -0.000000000000000000, -1.000000000000000000, -0.000000000000000000 ) ) ;
#25911 = EDGE_CURVE ( 'NONE', #58191, #22696, #78329, .T. ) ;
#25912 = FACE_BOUND ( 'NONE', #34395, .T. ) ;
#25914 = EDGE_CURVE ( 'NONE', #105966, #63642, #13544, .T. ) ;
#25913 = ORIENTED_EDGE ( 'NONE', *, *, #96139, .F. ) ;
#25915 = CARTESIAN_POINT ( 'NONE',  ( 185.1927083336747160, 6.551208109652275624, -3.782341765624998686 ) ) ;
#25916 = EDGE_CURVE ( 'NONE', #31579, #127574, #5137, .T. ) ;
#25917 = CARTESIAN_POINT ( 'NONE',  ( -2.499999999999996003, 2.500000000000000000, 0.09999999999999772959 ) ) ;
#25918 = CARTESIAN_POINT ( 'NONE',  ( 108.0000000000000142, 8.500000000000000000, 0.000000000000000000 ) ) ;
#25919 = AXIS2_PLACEMENT_3D ( 'NONE', #75960, #79207, #128963 ) ;
#25920 = CARTESIAN_POINT ( 'NONE',  ( -3.750000000000026201, 12.50000000000000000, 5.802370205355744659 ) ) ;
#25921 = LINE ( 'NONE', #55380, #71576 ) ;
#25922 = PLANE ( 'NONE',  #115506 ) ;
#25923 = EDGE_CURVE ( 'NONE', #33163, #90278, #97085, .T. ) ;
#25924 = FACE_OUTER_BOUND ( 'NONE', #117770, .T. ) ;
#25925 = CARTESIAN_POINT ( 'NONE',  ( -10.65000000000000213, 2.500000000000000000, 2.611473670974873151 ) ) ;
#25927 = ADVANCED_FACE ( 'NONE', ( #55560 ), #105942, .T. ) ;
#25926 = VECTOR ( 'NONE', #88876, 1000.000000000000000 ) ;
#25928 = AXIS2_PLACEMENT_3D ( 'NONE', #117808, #56953, #35412 ) ;
#25929 = EDGE_CURVE ( 'NONE', #44028, #4134, #124284, .T. ) ;
#25930 = CARTESIAN_POINT ( 'NONE',  ( -3.750000000000025757, 12.50000000000000000, 1.407149913249508000 ) ) ;
#25931 = ORIENTED_EDGE ( 'NONE', *, *, #15820, .T. ) ;
#25932 = ORIENTED_EDGE ( 'NONE', *, *, #18717, .T. ) ;
#25933 = VERTEX_POINT ( 'NONE', #56187 ) ;
#25934 = ORIENTED_EDGE ( 'NONE', *, *, #128561, .F. ) ;
#25935 = ORIENTED_EDGE ( 'NONE', *, *, #25320, .F. ) ;
#25936 = LINE ( 'NONE', #6264, #379 ) ;
#25937 = DIRECTION ( 'NONE',  ( 0.000000000000000000, -0.9999939076577903929, 0.003490651415223739937 ) ) ;
#25938 = ORIENTED_EDGE ( 'NONE', *, *, #33960, .F. ) ;
#25939 = FACE_BOUND ( 'NONE', #440, .T. ) ;
#25940 = AXIS2_PLACEMENT_3D ( 'NONE', #12846, #41073, #31877 ) ;
#25941 = DIRECTION ( 'NONE',  ( 0.000000000000000000, 1.000000000000000000, 0.000000000000000000 ) ) ;
#25942 = VECTOR ( 'NONE', #129343, 1000.000000000000000 ) ;
#25943 = CIRCLE ( 'NONE', #122091, 0.06509327318403745899 ) ;
#25944 = CARTESIAN_POINT ( 'NONE',  ( -10.80000000000000249, 12.50000000000000000, -4.330127018922197202 ) ) ;
#25945 = LINE ( 'NONE', #56661, #11884 ) ;
#25946 = CARTESIAN_POINT ( 'NONE',  ( -6.900000000000019007, 12.50000000000000000, -0.2813168883297409439 ) ) ;
#25947 = PLANE ( 'NONE',  #89358 ) ;
#25948 = ORIENTED_EDGE ( 'NONE', *, *, #15334, .F. ) ;
#25949 = DIRECTION ( 'NONE',  ( -4.274815082592931898E-19, -0.9999939076577903929, -0.003490651415223739937 ) ) ;
#25950 = EDGE_LOOP ( 'NONE', ( #100604, #70337 ) ) ;
#25951 = CIRCLE ( 'NONE', #13413, 0.06509327318403745899 ) ;
#25952 = ORIENTED_EDGE ( 'NONE', *, *, #89020, .F. ) ;
#25953 = ORIENTED_EDGE ( 'NONE', *, *, #128507, .T. ) ;
#25954 = DIRECTION ( 'NONE',  ( 0.000000000000000000, 0.000000000000000000, 1.000000000000000000 ) ) ;
#25955 = PLANE ( 'NONE',  #64436 ) ;
#25957 = AXIS2_PLACEMENT_3D ( 'NONE', #37540, #58476, #108830 ) ;
#25956 = CARTESIAN_POINT ( 'NONE',  ( 1.449999999999952216, 2.500000000000000000, -2.611473670974877592 ) ) ;
#25958 = ORIENTED_EDGE ( 'NONE', *, *, #87960, .T. ) ;
#25959 = CARTESIAN_POINT ( 'NONE',  ( 16.04820284657640173, 2.500000000000064393, -6.585610460626884155 ) ) ;
#25960 = EDGE_CURVE ( 'NONE', #57754, #117365, #83732, .T. ) ;
#25961 = AXIS2_PLACEMENT_3D ( 'NONE', #37819, #107195, #17520 ) ;
#25962 = CARTESIAN_POINT ( 'NONE',  ( 10.64999999999990976, 2.500000000000000000, 2.511473670974873507 ) ) ;
#25963 = EDGE_CURVE ( 'NONE', #39201, #90179, #80376, .T. ) ;
#25964 = CARTESIAN_POINT ( 'NONE',  ( 6.649999999999928413, 2.500000000000000000, 1.472243186433545459 ) ) ;
#25965 = CARTESIAN_POINT ( 'NONE',  ( 187.2760416670080588, 6.551208109652274736, 3.782341765625001351 ) ) ;
#25966 = DIRECTION ( 'NONE',  ( -0.000000000000000000, -1.000000000000000000, -0.000000000000000000 ) ) ;
#25967 = LINE ( 'NONE', #37081, #39147 ) ;
#25968 = EDGE_CURVE ( 'NONE', #112183, #44934, #75827, .T. ) ;
#25969 = ORIENTED_EDGE ( 'NONE', *, *, #67033, .F. ) ;
#25970 = CARTESIAN_POINT ( 'NONE',  ( 5.399999999999932854, 12.50000000000000000, 5.022947341949748790 ) ) ;
#25971 = ADVANCED_FACE ( 'NONE', ( #104014 ), #45742, .T. ) ;
#25972 = ORIENTED_EDGE ( 'NONE', *, *, #50853, .T. ) ;
#25973 = ADVANCED_FACE ( 'NONE', ( #123632 ), #32374, .T. ) ;
#25974 = ORIENTED_EDGE ( 'NONE', *, *, #48535, .T. ) ;
#25975 = FACE_OUTER_BOUND ( 'NONE', #40821, .T. ) ;
#25976 = AXIS2_PLACEMENT_3D ( 'NONE', #11670, #63997, #22807 ) ;
#25977 = CONICAL_SURFACE ( 'NONE', #128402, 0.1000000000000002554, 0.003490658503988666988 ) ;
#25978 = CARTESIAN_POINT ( 'NONE',  ( -8.550000000000013145, 12.50000000000000000, 2.446380397790835826 ) ) ;
#25979 = CONICAL_SURFACE ( 'NONE', #42727, 0.1000000000000002554, 0.003490658503988666988 ) ;
#25980 = CARTESIAN_POINT ( 'NONE',  ( 0.1999999999999576006, 2.500000000000000000, -4.676537180435978769 ) ) ;
#25981 = VERTEX_POINT ( 'NONE', #114468 ) ;
#25982 = EDGE_CURVE ( 'NONE', #85528, #80364, #99253, .T. ) ;
#25983 = EDGE_LOOP ( 'NONE', ( #96593, #94912 ) ) ;
#25984 = DIRECTION ( 'NONE',  ( 0.000000000000000000, 1.000000000000000000, 0.000000000000000000 ) ) ;
#25985 = CIRCLE ( 'NONE', #120067, 0.4999999999999995559 ) ;
#25986 = AXIS2_PLACEMENT_3D ( 'NONE', #6334, #46283, #126139 ) ;
#25987 = VECTOR ( 'NONE', #40984, 1000.000000000000000 ) ;
#25988 = CARTESIAN_POINT ( 'NONE',  ( 8.749999999999920064, 2.500000000000000000, 5.802370205355744659 ) ) ;
#25989 = AXIS2_PLACEMENT_3D ( 'NONE', #112277, #52065, #62534 ) ;
#25990 = CARTESIAN_POINT ( 'NONE',  ( -3.950000000000026379, 2.500000000000000000, 6.741600689897071952 ) ) ;
#25991 = ORIENTED_EDGE ( 'NONE', *, *, #49032, .T. ) ;
#25992 = VERTEX_POINT ( 'NONE', #65359 ) ;
#25993 = CARTESIAN_POINT ( 'NONE',  ( 13.54999999999989591, 2.500000000000000000, -1.718653347947326049 ) ) ;
#25994 = ORIENTED_EDGE ( 'NONE', *, *, #66567, .F. ) ;
#25995 = DIRECTION ( 'NONE',  ( 0.000000000000000000, 0.000000000000000000, -1.000000000000000000 ) ) ;
#25996 = CIRCLE ( 'NONE', #13450, 0.1000000000000002554 ) ;
#25997 = CONICAL_SURFACE ( 'NONE', #65685, 0.09999999999999982514, 0.003490658503988666988 ) ;
#25998 = DIRECTION ( 'NONE',  ( -0.000000000000000000, -1.000000000000000000, -0.000000000000000000 ) ) ;
#25999 = VERTEX_POINT ( 'NONE', #57495 ) ;
#26000 = CARTESIAN_POINT ( 'NONE',  ( -9.350000000000006750, 12.50000000000000000, 2.576566944158910744 ) ) ;
#26001 = DIRECTION ( 'NONE',  ( 0.000000000000000000, 1.000000000000000000, 0.000000000000000000 ) ) ;
#26002 = DIRECTION ( 'NONE',  ( 0.000000000000000000, 1.000000000000000000, 0.000000000000000000 ) ) ;
#26003 = VECTOR ( 'NONE', #110523, 1000.000000000000000 ) ;
#26004 = EDGE_CURVE ( 'NONE', #107927, #79022, #59563, .T. ) ;
#26005 = CARTESIAN_POINT ( 'NONE',  ( 1.899999999999949507, 2.500000000000000000, 3.983716857408420964 ) ) ;
#26006 = ORIENTED_EDGE ( 'NONE', *, *, #60912, .T. ) ;
#26007 = CARTESIAN_POINT ( 'NONE',  ( -11.44999999999999751, 2.500000000000000000, 1.718653347947321386 ) ) ;
#26008 = DIRECTION ( 'NONE',  ( -4.274815082592931898E-19, -0.9999939076577903929, -0.003490651415223739937 ) ) ;
#26009 = ORIENTED_EDGE ( 'NONE', *, *, #42330, .T. ) ;
#26010 = VERTEX_POINT ( 'NONE', #41580 ) ;
#26011 = CARTESIAN_POINT ( 'NONE',  ( 185.0885416670080872, -6.551208109652273848, -3.782341765625003571 ) ) ;
#26012 = CARTESIAN_POINT ( 'NONE',  ( -7.100000000000017408, 2.500000000000000000, -3.637306695894650055 ) ) ;
#26013 = DIRECTION ( 'NONE',  ( 0.000000000000000000, 1.000000000000000000, 0.000000000000000000 ) ) ;
#26014 = CARTESIAN_POINT ( 'NONE',  ( -2.900000000000029221, 2.500000000000000000, -5.022947341949754119 ) ) ;
#26015 = VECTOR ( 'NONE', #125691, 1000.000000000000000 ) ;
#26016 = LINE ( 'NONE', #37760, #926 ) ;
#26017 = DIRECTION ( 'NONE',  ( 0.000000000000000000, 0.000000000000000000, 1.000000000000000000 ) ) ;
#26019 = EDGE_CURVE ( 'NONE', #60793, #21571, #110292, .T. ) ;
#26018 = DIRECTION ( 'NONE',  ( 0.000000000000000000, 1.000000000000000000, 0.000000000000000000 ) ) ;
#26020 = DIRECTION ( 'NONE',  ( 0.000000000000000000, -0.000000000000000000, 1.000000000000000000 ) ) ;
#26021 = DIRECTION ( 'NONE',  ( 0.000000000000000000, 1.000000000000000000, 0.000000000000000000 ) ) ;
#26023 = CONICAL_SURFACE ( 'NONE', #34438, 0.1000000000000000472, 0.003490658503988666988 ) ;
#26022 = DIRECTION ( 'NONE',  ( 0.000000000000000000, -0.000000000000000000, 1.000000000000000000 ) ) ;
#26024 = VERTEX_POINT ( 'NONE', #117025 ) ;
#26025 = CONICAL_SURFACE ( 'NONE', #34440, 0.1000000000000002554, 0.003490658503988666988 ) ;
#26026 = VERTEX_POINT ( 'NONE', #28032 ) ;
#26027 = ORIENTED_EDGE ( 'NONE', *, *, #33172, .T. ) ;
#26028 = EDGE_CURVE ( 'NONE', #94609, #124362, #73087, .T. ) ;
#26029 = DIRECTION ( 'NONE',  ( 0.000000000000000000, 0.000000000000000000, 1.000000000000000000 ) ) ;
#26030 = DIRECTION ( 'NONE',  ( 0.000000000000000000, -0.000000000000000000, 1.000000000000000000 ) ) ;
#26031 = CARTESIAN_POINT ( 'NONE',  ( -11.05000000000000249, 12.50000000000000000, -1.753560074763284682 ) ) ;
#26032 = VERTEX_POINT ( 'NONE', #77130 ) ;
#26033 = CARTESIAN_POINT ( 'NONE',  ( -2.499999999999996003, 2.500000000000000000, -0.1000000000000022815 ) ) ;
#26034 = AXIS2_PLACEMENT_3D ( 'NONE', #70322, #49408, #89313 ) ;
#26035 = AXIS2_PLACEMENT_3D ( 'NONE', #35437, #75337, #115234 ) ;
#26037 = VERTEX_POINT ( 'NONE', #81485 ) ;
#26036 = CARTESIAN_POINT ( 'NONE',  ( -14.59999999999998366, 12.50000000000000000, -1.084202172485504434E-16 ) ) ;
#26038 = DIRECTION ( 'NONE',  ( 0.000000000000000000, 0.000000000000000000, -1.000000000000000000 ) ) ;
#26039 = ORIENTED_EDGE ( 'NONE', *, *, #118236, .F. ) ;
#26040 = AXIS2_PLACEMENT_3D ( 'NONE', #41378, #112684, #31542 ) ;
#26041 = AXIS2_PLACEMENT_3D ( 'NONE', #108356, #9521, #27869 ) ;
#26042 = ORIENTED_EDGE ( 'NONE', *, *, #49644, .T. ) ;
#26043 = EDGE_LOOP ( 'NONE', ( #11044, #6468, #91181, #127283 ) ) ;
#26044 = ORIENTED_EDGE ( 'NONE', *, *, #78274, .F. ) ;
#26045 = DIRECTION ( 'NONE',  ( -0.000000000000000000, 1.000000000000000000, -0.000000000000000000 ) ) ;
#26046 = CIRCLE ( 'NONE', #88738, 0.09999999999999982514 ) ;
#26047 = CARTESIAN_POINT ( 'NONE',  ( 0.8499999999999550138, 12.50000000000000000, -5.802370205355749988 ) ) ;
#26048 = CARTESIAN_POINT ( 'NONE',  ( 2.899999999999943956, 12.50000000000000000, 4.330127018922196314 ) ) ;
#26049 = CIRCLE ( 'NONE', #46986, 0.06509327318403745899 ) ;
#26050 = CARTESIAN_POINT ( 'NONE',  ( 5.199999999999933564, 2.500000000000000000, 0.3464101615137735735 ) ) ;
#26051 = EDGE_LOOP ( 'NONE', ( #31125, #126761 ) ) ;
#26052 = EDGE_CURVE ( 'NONE', #15482, #90797, #92987, .T. ) ;
#26053 = DIRECTION ( 'NONE',  ( 0.000000000000000000, 0.000000000000000000, -1.000000000000000000 ) ) ;
#26054 = EDGE_LOOP ( 'NONE', ( #8652, #125730 ) ) ;
#26055 = CARTESIAN_POINT ( 'NONE',  ( 7.099999999999928590, 2.500000000000000000, 4.230127018922196669 ) ) ;
#26056 = CARTESIAN_POINT ( 'NONE',  ( 13.80955901367097916, -1.500000000000063061, -7.955427458311421063 ) ) ;
#26057 = DIRECTION ( 'NONE',  ( -4.274815082592931898E-19, -0.9999939076577903929, -0.003490651415223739937 ) ) ;
#26058 = CARTESIAN_POINT ( 'NONE',  ( 16.79927703354229607, -2.472530191752539075, 3.248144252804014975 ) ) ;
#26059 = EDGE_CURVE ( 'NONE', #1993, #61083, #88862, .T. ) ;
#26060 = ORIENTED_EDGE ( 'NONE', *, *, #128758, .T. ) ;
#26061 = AXIS2_PLACEMENT_3D ( 'NONE', #9094, #39239, #11013 ) ;
#26062 = ORIENTED_EDGE ( 'NONE', *, *, #82971, .T. ) ;
#26063 = AXIS2_PLACEMENT_3D ( 'NONE', #119529, #10848, #108424 ) ;
#26064 = ORIENTED_EDGE ( 'NONE', *, *, #124397, .T. ) ;
#26065 = DIRECTION ( 'NONE',  ( 0.000000000000000000, -0.9999939076577903929, 0.003490651415223739937 ) ) ;
#26066 = CARTESIAN_POINT ( 'NONE',  ( 108.0000000000000142, 9.000000000000001776, -0.2500000000000000000 ) ) ;
#26067 = EDGE_CURVE ( 'NONE', #101516, #116590, #80845, .T. ) ;
#26068 = EDGE_CURVE ( 'NONE', #87604, #65296, #107227, .T. ) ;
#26069 = CARTESIAN_POINT ( 'NONE',  ( 11.84999999999990727, 12.50000000000000000, 6.148780366869520009 ) ) ;
#26070 = ADVANCED_FACE ( 'NONE', ( #17547 ), #120759, .F. ) ;
#26071 = FACE_BOUND ( 'NONE', #122450, .T. ) ;
#26072 = ADVANCED_FACE ( 'NONE', ( #100472 ), #9452, .T. ) ;
#26073 = LINE ( 'NONE', #105919, #116264 ) ;
#26074 = CARTESIAN_POINT ( 'NONE',  ( 11.24999999999990941, 12.50000000000000000, -1.472243186433550122 ) ) ;
#26075 = LINE ( 'NONE', #52453, #43469 ) ;
#26076 = DIRECTION ( 'NONE',  ( -1.000000000000000000, 0.000000000000000000, 0.000000000000000000 ) ) ;
#26077 = AXIS2_PLACEMENT_3D ( 'NONE', #19006, #30153, #50414 ) ;
#26078 = AXIS2_PLACEMENT_3D ( 'NONE', #50006, #17937, #29072 ) ;
#26079 = EDGE_CURVE ( 'NONE', #117106, #85617, #67944, .T. ) ;
#26080 = CARTESIAN_POINT ( 'NONE',  ( 185.6718750003414016, 9.264065473108010111E-16, -7.564683531250000925 ) ) ;
#26082 = EDGE_CURVE ( 'NONE', #119417, #29857, #60574, .T. ) ;
#26081 = AXIS2_PLACEMENT_3D ( 'NONE', #41188, #12333, #81097 ) ;
#26083 = FACE_OUTER_BOUND ( 'NONE', #23112, .T. ) ;
#26084 = EDGE_CURVE ( 'NONE', #16737, #29270, #101121, .T. ) ;
#26085 = DIRECTION ( 'NONE',  ( 0.000000000000000000, 1.000000000000000000, 0.000000000000000000 ) ) ;
#26086 = EDGE_CURVE ( 'NONE', #108562, #30880, #21988, .T. ) ;
#26087 = AXIS2_PLACEMENT_3D ( 'NONE', #116298, #86849, #26651 ) ;
#26088 = AXIS2_PLACEMENT_3D ( 'NONE', #14320, #126228, #96115 ) ;
#26089 = EDGE_CURVE ( 'NONE', #32323, #112846, #90921, .T. ) ;
#26090 = DIRECTION ( 'NONE',  ( 0.000000000000000000, 1.000000000000000000, 0.000000000000000000 ) ) ;
#26091 = ORIENTED_EDGE ( 'NONE', *, *, #50618, .T. ) ;
#26092 = ORIENTED_EDGE ( 'NONE', *, *, #63674, .T. ) ;
#26093 = VERTEX_POINT ( 'NONE', #117665 ) ;
#26094 = VERTEX_POINT ( 'NONE', #58148 ) ;
#26095 = AXIS2_PLACEMENT_3D ( 'NONE', #128753, #110367, #29251 ) ;
#26096 = DIRECTION ( 'NONE',  ( 0.000000000000000000, -0.000000000000000000, 1.000000000000000000 ) ) ;
#26097 = FACE_BOUND ( 'NONE', #24302, .T. ) ;
#26098 = EDGE_CURVE ( 'NONE', #15557, #113294, #55419, .T. ) ;
#26099 = DIRECTION ( 'NONE',  ( -0.000000000000000000, -1.000000000000000000, -0.000000000000000000 ) ) ;
#26100 = ORIENTED_EDGE ( 'NONE', *, *, #109419, .F. ) ;
#26101 = CARTESIAN_POINT ( 'NONE',  ( 48.84100846696811971, 2.320798421900499342, 5.300800859553110200 ) ) ;
#26102 = DIRECTION ( 'NONE',  ( -0.000000000000000000, -1.000000000000000000, -0.000000000000000000 ) ) ;
#26104 = ORIENTED_EDGE ( 'NONE', *, *, #124792, .F. ) ;
#26103 = CIRCLE ( 'NONE', #7202, 0.1000000000000000472 ) ;
#26105 = DIRECTION ( 'NONE',  ( 0.000000000000000000, 1.000000000000000000, 0.000000000000000000 ) ) ;
#26106 = CARTESIAN_POINT ( 'NONE',  ( -3.350000000000031619, 2.500000000000000000, -5.802370205355749988 ) ) ;
#26107 = ORIENTED_EDGE ( 'NONE', *, *, #48364, .F. ) ;
#26108 = CARTESIAN_POINT ( 'NONE',  ( 1.049999999999953637, 2.500000000000000000, -1.918653347947326004 ) ) ;
#26109 = LINE ( 'NONE', #106586, #120687 ) ;
#26110 = CIRCLE ( 'NONE', #93015, 0.06509327318403745899 ) ;
#26111 = ORIENTED_EDGE ( 'NONE', *, *, #110713, .F. ) ;
#26112 = DIRECTION ( 'NONE',  ( -0.000000000000000000, 1.000000000000000000, -0.000000000000000000 ) ) ;
#26113 = DIRECTION ( 'NONE',  ( 0.000000000000000000, 0.000000000000000000, 1.000000000000000000 ) ) ;
#26114 = ORIENTED_EDGE ( 'NONE', *, *, #28757, .F. ) ;
#26115 = FACE_OUTER_BOUND ( 'NONE', #27807, .T. ) ;
#26116 = ORIENTED_EDGE ( 'NONE', *, *, #114199, .F. ) ;
#26117 = ORIENTED_EDGE ( 'NONE', *, *, #69841, .F. ) ;
#26118 = CARTESIAN_POINT ( 'NONE',  ( 187.3906250003414016, 0.000000000000000000, 7.700000000000000178 ) ) ;
#26119 = ORIENTED_EDGE ( 'NONE', *, *, #44596, .F. ) ;
#26120 = DIRECTION ( 'NONE',  ( 0.000000000000000000, 1.000000000000000000, 0.000000000000000000 ) ) ;
#26121 = FACE_OUTER_BOUND ( 'NONE', #127393, .T. ) ;
#26122 = VECTOR ( 'NONE', #105583, 1000.000000000000000 ) ;
#26123 = EDGE_CURVE ( 'NONE', #124197, #52455, #120121, .T. ) ;
#26124 = VERTEX_POINT ( 'NONE', #30468 ) ;
#26127 = EDGE_CURVE ( 'NONE', #55439, #23160, #37218, .T. ) ;
#26126 = CARTESIAN_POINT ( 'NONE',  ( -11.44999999999999751, 12.50000000000000000, 6.083687093685483660 ) ) ;
#26125 = AXIS2_PLACEMENT_3D ( 'NONE', #54270, #4488, #34654 ) ;
#26128 = DIRECTION ( 'NONE',  ( -0.000000000000000000, 1.000000000000000000, -0.000000000000000000 ) ) ;
#26129 = LINE ( 'NONE', #124324, #73710 ) ;
#26130 = CARTESIAN_POINT ( 'NONE',  ( 8.299999999999922551, 12.50000000000000000, -4.265033745738164406 ) ) ;
#26131 = CARTESIAN_POINT ( 'NONE',  ( 8.549999999999922551, 2.500000000000000000, 2.411473670974873862 ) ) ;
#26132 = DIRECTION ( 'NONE',  ( -0.000000000000000000, 1.000000000000000000, -0.000000000000000000 ) ) ;
#26133 = EDGE_CURVE ( 'NONE', #64399, #79354, #107653, .T. ) ;
#26134 = EDGE_LOOP ( 'NONE', ( #29702, #113102, #52227, #24506 ) ) ;
#26135 = VERTEX_POINT ( 'NONE', #24494 ) ;
#26136 = CARTESIAN_POINT ( 'NONE',  ( -0.4000000000000331624, 12.50000000000000000, -0.6928203230275519209 ) ) ;
#26137 = CIRCLE ( 'NONE', #5181, 0.1000000000000002554 ) ;
#26138 = AXIS2_PLACEMENT_3D ( 'NONE', #33049, #72957, #112880 ) ;
#26139 = CARTESIAN_POINT ( 'NONE',  ( 0.8499999999999553468, 12.50000000000000000, 1.407149913249508000 ) ) ;
#26140 = DIRECTION ( 'NONE',  ( 0.000000000000000000, 1.000000000000000000, 0.000000000000000000 ) ) ;
#26142 = VERTEX_POINT ( 'NONE', #73576 ) ;
#26141 = ORIENTED_EDGE ( 'NONE', *, *, #43805, .T. ) ;
#26143 = ORIENTED_EDGE ( 'NONE', *, *, #106779, .F. ) ;
#26144 = FACE_OUTER_BOUND ( 'NONE', #125156, .T. ) ;
#26145 = DIRECTION ( 'NONE',  ( 0.000000000000000000, 0.000000000000000000, -1.000000000000000000 ) ) ;
#26146 = DIRECTION ( 'NONE',  ( 0.000000000000000000, 0.000000000000000000, 1.000000000000000000 ) ) ;
#26147 = DIRECTION ( 'NONE',  ( -1.000000000000000000, 0.000000000000000000, 0.000000000000000000 ) ) ;
#26148 = DIRECTION ( 'NONE',  ( 0.000000000000000000, -0.9999939076577903929, 0.003490651415223739937 ) ) ;
#26149 = CARTESIAN_POINT ( 'NONE',  ( -14.54999999999998472, 2.500000000000000000, -2.165063509461099489 ) ) ;
#26150 = DIRECTION ( 'NONE',  ( 0.000000000000000000, 0.000000000000000000, -1.000000000000000000 ) ) ;
#26151 = DIRECTION ( 'NONE',  ( 0.000000000000000000, 1.000000000000000000, 0.000000000000000000 ) ) ;
#26152 = CARTESIAN_POINT ( 'NONE',  ( 9.149999999999915090, 2.500000000000000000, -2.065063509461102065 ) ) ;
#26153 = CIRCLE ( 'NONE', #45032, 0.06509327318403745899 ) ;
#26154 = DIRECTION ( 'NONE',  ( -0.000000000000000000, -1.000000000000000000, -0.000000000000000000 ) ) ;
#26155 = ORIENTED_EDGE ( 'NONE', *, *, #31142, .T. ) ;
#26156 = CIRCLE ( 'NONE', #99313, 0.06509327318403745899 ) ;
#26157 = AXIS2_PLACEMENT_3D ( 'NONE', #86704, #114236, #35680 ) ;
#26158 = DIRECTION ( 'NONE',  ( 0.000000000000000000, 0.000000000000000000, 1.000000000000000000 ) ) ;
#26159 = AXIS2_PLACEMENT_3D ( 'NONE', #93107, #122564, #42065 ) ;
#26160 = VERTEX_POINT ( 'NONE', #44790 ) ;
#26161 = VERTEX_POINT ( 'NONE', #84043 ) ;
#26162 = CARTESIAN_POINT ( 'NONE',  ( -11.89999999999999680, 2.500000000000000000, 0.3464101615137776813 ) ) ;
#26163 = DIRECTION ( 'NONE',  ( -4.274815082592931898E-19, -0.9999939076577903929, -0.003490651415223739937 ) ) ;
#26164 = CARTESIAN_POINT ( 'NONE',  ( 11.64999999999990443, 2.500000000000000000, 2.857883832488649301 ) ) ;
#26165 = DIRECTION ( 'NONE',  ( 0.000000000000000000, 1.000000000000000000, 0.000000000000000000 ) ) ;
#26166 = CIRCLE ( 'NONE', #44949, 0.06509327318403745899 ) ;
#26167 = DIRECTION ( 'NONE',  ( 0.000000000000000000, -0.9999939076577903929, 0.003490651415223739937 ) ) ;
#26168 = DIRECTION ( 'NONE',  ( -0.000000000000000000, -1.000000000000000000, -0.000000000000000000 ) ) ;
#26169 = FACE_OUTER_BOUND ( 'NONE', #37087, .T. ) ;
#26170 = VERTEX_POINT ( 'NONE', #84698 ) ;
#26171 = DIRECTION ( 'NONE',  ( 0.000000000000000000, 0.000000000000000000, 1.000000000000000000 ) ) ;
#26172 = AXIS2_PLACEMENT_3D ( 'NONE', #58712, #116323, #125509 ) ;
#26173 = CARTESIAN_POINT ( 'NONE',  ( -3.749999999999991118, 12.50000000000000000, 2.099970236277060032 ) ) ;
#26175 = EDGE_LOOP ( 'NONE', ( #114180, #72064, #58522, #75633 ) ) ;
#26174 = AXIS2_PLACEMENT_3D ( 'NONE', #89433, #91365, #110984 ) ;
#26176 = AXIS2_PLACEMENT_3D ( 'NONE', #64411, #2930, #23859 ) ;
#26177 = ORIENTED_EDGE ( 'NONE', *, *, #67271, .F. ) ;
#26178 = ORIENTED_EDGE ( 'NONE', *, *, #107038, .T. ) ;
#26179 = VECTOR ( 'NONE', #26348, 1000.000000000000000 ) ;
#26180 = EDGE_CURVE ( 'NONE', #86483, #117851, #12719, .T. ) ;
#26182 = VERTEX_POINT ( 'NONE', #92591 ) ;
#26181 = ADVANCED_FACE ( 'NONE', ( #33046 ), #38725, .T. ) ;
#26183 = DIRECTION ( 'NONE',  ( 0.000000000000000000, 0.000000000000000000, 1.000000000000000000 ) ) ;
#26184 = FACE_OUTER_BOUND ( 'NONE', #19331, .T. ) ;
#26185 = DIRECTION ( 'NONE',  ( 0.000000000000000000, 0.000000000000000000, 1.000000000000000000 ) ) ;
#26186 = CARTESIAN_POINT ( 'NONE',  ( -5.650000000000023448, 2.500000000000000000, -6.941600689897078347 ) ) ;
#26187 = B_SPLINE_CURVE_WITH_KNOTS ( 'NONE', 3,
 ( #19562, #7798, #88950, #98113, #99428, #18267 ),
 .UNSPECIFIED., .F., .F.,
 ( 4, 2, 4 ),
 ( 0.000000000000000000, 0.5000000000000000000, 1.000000000000000000 ),
 .UNSPECIFIED. ) ;
#26188 = DIRECTION ( 'NONE',  ( 0.000000000000000000, -0.9999939076577903929, 0.003490651415223739937 ) ) ;
#26189 = ORIENTED_EDGE ( 'NONE', *, *, #77034, .T. ) ;
#26190 = EDGE_CURVE ( 'NONE', #46899, #122246, #49182, .T. ) ;
#26191 = PLANE ( 'NONE',  #114169 ) ;
#26192 = CIRCLE ( 'NONE', #101412, 7.500000000000000000 ) ;
#26193 = LINE ( 'NONE', #106672, #85364 ) ;
#26194 = ORIENTED_EDGE ( 'NONE', *, *, #37299, .F. ) ;
#26195 = ORIENTED_EDGE ( 'NONE', *, *, #125840, .T. ) ;
#26196 = ORIENTED_EDGE ( 'NONE', *, *, #89631, .F. ) ;
#26197 = DIRECTION ( 'NONE',  ( -0.000000000000000000, -1.000000000000000000, -0.000000000000000000 ) ) ;
#26198 = CIRCLE ( 'NONE', #24144, 0.09999999999999982514 ) ;
#26199 = AXIS2_PLACEMENT_3D ( 'NONE', #35616, #75516, #125903 ) ;
#26200 = DIRECTION ( 'NONE',  ( -4.274815082592931898E-19, -0.9999939076577903929, -0.003490651415223739937 ) ) ;
#26201 = DIRECTION ( 'NONE',  ( -0.000000000000000000, -1.000000000000000000, -0.000000000000000000 ) ) ;
#26202 = AXIS2_PLACEMENT_3D ( 'NONE', #109642, #8839, #19306 ) ;
#26203 = EDGE_LOOP ( 'NONE', ( #65106, #106674, #118992, #15326 ) ) ;
#26204 = FACE_OUTER_BOUND ( 'NONE', #68119, .T. ) ;
#26205 = CARTESIAN_POINT ( 'NONE',  ( 7.499999999999925393, 2.500000000000000000, 5.122947341949749323 ) ) ;
#26206 = LINE ( 'NONE', #87690, #119408 ) ;
#26207 = DIRECTION ( 'NONE',  ( -0.000000000000000000, -1.000000000000000000, -0.000000000000000000 ) ) ;
#26208 = CARTESIAN_POINT ( 'NONE',  ( -3.350000000000028955, 12.50000000000000000, -2.230156782645139391 ) ) ;
#26209 = AXIS2_PLACEMENT_3D ( 'NONE', #113954, #72106, #14441 ) ;
#26210 = ADVANCED_FACE ( 'NONE', ( #52656 ), #28234, .T. ) ;
#26211 = EDGE_LOOP ( 'NONE', ( #46104, #23469, #7188, #36208 ) ) ;
#26212 = CARTESIAN_POINT ( 'NONE',  ( 11.04999999999990834, 2.500000000000000000, 1.818653347947321475 ) ) ;
#26213 = AXIS2_PLACEMENT_3D ( 'NONE', #65858, #33206, #14797 ) ;
#26214 = ORIENTED_EDGE ( 'NONE', *, *, #44376, .T. ) ;
#26215 = ORIENTED_EDGE ( 'NONE', *, *, #84449, .T. ) ;
#26216 = EDGE_CURVE ( 'NONE', #81046, #103611, #126523, .T. ) ;
#26217 = ORIENTED_EDGE ( 'NONE', *, *, #56637, .T. ) ;
#26218 = ADVANCED_FACE ( 'NONE', ( #74239 ), #44960, .T. ) ;
#26219 = DIRECTION ( 'NONE',  ( 0.000000000000000000, 0.000000000000000000, 1.000000000000000000 ) ) ;
#26220 = EDGE_CURVE ( 'NONE', #118224, #46019, #104342, .T. ) ;
#26221 = FACE_BOUND ( 'NONE', #107634, .T. ) ;
#26222 = EDGE_CURVE ( 'NONE', #106042, #101934, #120171, .T. ) ;
#26223 = FACE_OUTER_BOUND ( 'NONE', #111516, .T. ) ;
#26224 = LINE ( 'NONE', #67394, #73674 ) ;
#26225 = CARTESIAN_POINT ( 'NONE',  ( 3.749999999999942268, 2.500000000000000000, -1.472243186433550122 ) ) ;
#26226 = CIRCLE ( 'NONE', #65922, 0.06509327318403745899 ) ;
#26227 = VECTOR ( 'NONE', #104344, 1000.000000000000000 ) ;
#26228 = ADVANCED_FACE ( 'NONE', ( #124627 ), #62504, .T. ) ;
#26229 = ORIENTED_EDGE ( 'NONE', *, *, #57386, .F. ) ;
#26230 = FACE_OUTER_BOUND ( 'NONE', #78502, .T. ) ;
#26231 = CARTESIAN_POINT ( 'NONE',  ( -7.950000000000012612, 2.500000000000000000, 2.065063509461097624 ) ) ;
#26232 = EDGE_CURVE ( 'NONE', #126222, #92046, #19922, .T. ) ;
#26233 = DIRECTION ( 'NONE',  ( -0.000000000000000000, 1.000000000000000000, -0.000000000000000000 ) ) ;
#26234 = DIRECTION ( 'NONE',  ( 0.000000000000000000, -0.000000000000000000, 1.000000000000000000 ) ) ;
#26235 = ORIENTED_EDGE ( 'NONE', *, *, #49500, .T. ) ;
#26236 = DIRECTION ( 'NONE',  ( -0.000000000000000000, 1.000000000000000000, -0.000000000000000000 ) ) ;
#26237 = EDGE_CURVE ( 'NONE', #18715, #95681, #103537, .T. ) ;
#26238 = DIRECTION ( 'NONE',  ( -0.000000000000000000, -1.000000000000000000, -0.000000000000000000 ) ) ;
#26239 = AXIS2_PLACEMENT_3D ( 'NONE', #109840, #60741, #89549 ) ;
#26240 = ORIENTED_EDGE ( 'NONE', *, *, #14862, .T. ) ;
#26241 = FACE_OUTER_BOUND ( 'NONE', #14272, .T. ) ;
#26242 = EDGE_CURVE ( 'NONE', #108236, #50883, #101393, .T. ) ;
#26243 = VECTOR ( 'NONE', #98100, 1000.000000000000000 ) ;
#26244 = FACE_BOUND ( 'NONE', #4216, .T. ) ;
#26245 = EDGE_CURVE ( 'NONE', #47855, #74712, #122060, .T. ) ;
#26246 = CARTESIAN_POINT ( 'NONE',  ( 0.3999999999999568345, 12.50000000000000000, -4.957854068765716882 ) ) ;
#26247 = AXIS2_PLACEMENT_3D ( 'NONE', #5479, #85347, #3564 ) ;
#26248 = ORIENTED_EDGE ( 'NONE', *, *, #25468, .F. ) ;
#26249 = DIRECTION ( 'NONE',  ( -0.000000000000000000, -1.000000000000000000, -0.000000000000000000 ) ) ;
#26250 = CARTESIAN_POINT ( 'NONE',  ( 1.649999999999951061, 2.500000000000000000, -6.495190528383302464 ) ) ;
#26251 = AXIS2_PLACEMENT_3D ( 'NONE', #34252, #116005, #26355 ) ;
#26252 = ORIENTED_EDGE ( 'NONE', *, *, #81441, .T. ) ;
#26253 = ORIENTED_EDGE ( 'NONE', *, *, #37788, .T. ) ;
#26254 = CARTESIAN_POINT ( 'NONE',  ( 186.5416666666666856, -4.445597072760122614, 7.699999999999998401 ) ) ;
#26255 = ORIENTED_EDGE ( 'NONE', *, *, #79539, .T. ) ;
#26256 = CARTESIAN_POINT ( 'NONE',  ( 186.0052083336747444, -6.551208109652278289, 3.782341765624995134 ) ) ;
#26257 = CARTESIAN_POINT ( 'NONE',  ( -6.450000000000014388, 2.500000000000000000, 6.148780366869520897 ) ) ;
#26258 = CONICAL_SURFACE ( 'NONE', #116126, 0.1000000000000002554, 0.003490658503988666988 ) ;
#26259 = CARTESIAN_POINT ( 'NONE',  ( 1.849999999999951017, 12.50000000000000000, -6.083687093685488989 ) ) ;
#26260 = CARTESIAN_POINT ( 'NONE',  ( 11.89999999999990798, 2.500000000000000000, 4.576537180435972019 ) ) ;
#26261 = AXIS2_PLACEMENT_3D ( 'NONE', #9608, #412, #109072 ) ;
#26262 = DIRECTION ( 'NONE',  ( 0.000000000000000000, 1.000000000000000000, 0.000000000000000000 ) ) ;
#26263 = AXIS2_PLACEMENT_3D ( 'NONE', #68991, #9438, #50027 ) ;
#26264 = AXIS2_PLACEMENT_3D ( 'NONE', #48012, #116090, #16581 ) ;
#26265 = ORIENTED_EDGE ( 'NONE', *, *, #21941, .T. ) ;
#26266 = VECTOR ( 'NONE', #68298, 1000.000000000000000 ) ;
#26267 = FACE_OUTER_BOUND ( 'NONE', #90055, .T. ) ;
#26268 = DIRECTION ( 'NONE',  ( 0.000000000000000000, 0.000000000000000000, 1.000000000000000000 ) ) ;
#26269 = DIRECTION ( 'NONE',  ( 0.000000000000000000, 0.000000000000000000, -1.000000000000000000 ) ) ;
#26270 = AXIS2_PLACEMENT_3D ( 'NONE', #42621, #51782, #82539 ) ;
#26271 = DIRECTION ( 'NONE',  ( 0.000000000000000000, 0.000000000000000000, 1.000000000000000000 ) ) ;
#26273 = ORIENTED_EDGE ( 'NONE', *, *, #19615, .T. ) ;
#26272 = EDGE_LOOP ( 'NONE', ( #117452, #118165 ) ) ;
#26274 = FACE_BOUND ( 'NONE', #21919, .T. ) ;
#26275 = VERTEX_POINT ( 'NONE', #82124 ) ;
#26276 = CARTESIAN_POINT ( 'NONE',  ( 4.399999999999937295, 12.50000000000000000, 4.048810130592458201 ) ) ;
#26277 = FACE_OUTER_BOUND ( 'NONE', #23924, .T. ) ;
#26278 = EDGE_LOOP ( 'NONE', ( #61470, #17760, #112952, #96892 ) ) ;
#26279 = LINE ( 'NONE', #45276, #51419 ) ;
#26280 = DIRECTION ( 'NONE',  ( 0.000000000000000000, -0.9999939076577903929, 0.003490651415223739937 ) ) ;
#26281 = EDGE_CURVE ( 'NONE', #408, #70330, #63738, .T. ) ;
#26282 = DIRECTION ( 'NONE',  ( 0.000000000000000000, 1.000000000000000000, 0.000000000000000000 ) ) ;
#26283 = CARTESIAN_POINT ( 'NONE',  ( 8.349999999999923261, 12.50000000000000000, -5.802370205355749988 ) ) ;
#26284 = EDGE_LOOP ( 'NONE', ( #116974, #79430, #82301, #111110 ) ) ;
#26286 = EDGE_CURVE ( 'NONE', #82577, #1029, #47019, .T. ) ;
#26285 = CARTESIAN_POINT ( 'NONE',  ( 0.8499999999999536815, 2.500000000000000000, 5.702370205355745014 ) ) ;
#26287 = CARTESIAN_POINT ( 'NONE',  ( -7.499999999999980460, 2.500000000000000000, -4.430127018922202176 ) ) ;
#26288 = FACE_OUTER_BOUND ( 'NONE', #74506, .T. ) ;
#26289 = CARTESIAN_POINT ( 'NONE',  ( -11.25000000000000000, 2.500000000000000000, -7.188010851410850499 ) ) ;
#26290 = CIRCLE ( 'NONE', #1142, 0.1000000000000002554 ) ;
#26291 = DIRECTION ( 'NONE',  ( 0.000000000000000000, 0.000000000000000000, 1.000000000000000000 ) ) ;
#26292 = ORIENTED_EDGE ( 'NONE', *, *, #30641, .T. ) ;
#26293 = ORIENTED_EDGE ( 'NONE', *, *, #17985, .F. ) ;
#26294 = DIRECTION ( 'NONE',  ( 0.000000000000000000, 1.000000000000000000, 0.000000000000000000 ) ) ;
#26295 = ORIENTED_EDGE ( 'NONE', *, *, #112260, .T. ) ;
#26296 = DIRECTION ( 'NONE',  ( 0.000000000000000000, 0.000000000000000000, -1.000000000000000000 ) ) ;
#26298 = ORIENTED_EDGE ( 'NONE', *, *, #86084, .T. ) ;
#26297 = VERTEX_POINT ( 'NONE', #72317 ) ;
#26299 = AXIS2_PLACEMENT_3D ( 'NONE', #90983, #664, #31432 ) ;
#26300 = VERTEX_POINT ( 'NONE', #22585 ) ;
#26301 = CARTESIAN_POINT ( 'NONE',  ( -10.60000000000000142, 12.50000000000000000, 0.2813168883297362810 ) ) ;
#26302 = CIRCLE ( 'NONE', #103577, 0.06509327318403745899 ) ;
#26303 = CIRCLE ( 'NONE', #49297, 0.1000000000000002554 ) ;
#26304 = PLANE ( 'NONE',  #6614 ) ;
#26305 = FACE_OUTER_BOUND ( 'NONE', #6140, .T. ) ;
#26306 = CIRCLE ( 'NONE', #114310, 0.06509327318403745899 ) ;
#26307 =( LENGTH_UNIT ( ) NAMED_UNIT ( * ) SI_UNIT ( .MILLI., .METRE. ) );
#26308 = CARTESIAN_POINT ( 'NONE',  ( 165.4999999999999716, 0.000000000000000000, 1.500000000000000000 ) ) ;
#26309 = CARTESIAN_POINT ( 'NONE',  ( 7.099999999999928590, 12.50000000000000000, 3.702399969078682407 ) ) ;
#26310 = CARTESIAN_POINT ( 'NONE',  ( -11.44999999999999751, 12.50000000000000000, -2.576566944158911188 ) ) ;
#26311 = EDGE_LOOP ( 'NONE', ( #30418, #1571, #79543, #122096 ) ) ;
#26312 = CARTESIAN_POINT ( 'NONE',  ( -0.8000000000000381251, 2.500000000000000000, 4.330127018922196314 ) ) ;
#26313 = ORIENTED_EDGE ( 'NONE', *, *, #56596, .T. ) ;
#26314 = AXIS2_PLACEMENT_3D ( 'NONE', #39919, #20264, #70018 ) ;
#26315 = ORIENTED_EDGE ( 'NONE', *, *, #85064, .T. ) ;
#26316 = EDGE_LOOP ( 'NONE', ( #101164, #38719, #89883, #98867 ) ) ;
#26317 = ORIENTED_EDGE ( 'NONE', *, *, #5782, .F. ) ;
#26319 = CONICAL_SURFACE ( 'NONE', #103677, 0.1000000000000000056, 0.003490658503988666988 ) ;
#26318 = AXIS2_PLACEMENT_3D ( 'NONE', #62836, #24843, #4522 ) ;
#26320 = LINE ( 'NONE', #76056, #111145 ) ;
#26321 = ORIENTED_EDGE ( 'NONE', *, *, #72050, .T. ) ;
#26322 = VERTEX_POINT ( 'NONE', #102415 ) ;
#26323 = ADVANCED_FACE ( 'NONE', ( #123339 ), #7412, .T. ) ;
#26325 = CIRCLE ( 'NONE', #28378, 0.06509327318403741736 ) ;
#26324 = CARTESIAN_POINT ( 'NONE',  ( 5.599999999999931255, 2.500000000000000000, 3.983716857408420076 ) ) ;
#26326 = DIRECTION ( 'NONE',  ( 0.000000000000000000, 0.000000000000000000, 1.000000000000000000 ) ) ;
#26327 = CIRCLE ( 'NONE', #109949, 0.09999999999999982514 ) ;
#26328 = DIRECTION ( 'NONE',  ( 0.000000000000000000, 0.000000000000000000, 1.000000000000000000 ) ) ;
#26329 = DIRECTION ( 'NONE',  ( 0.000000000000000000, 0.000000000000000000, 1.000000000000000000 ) ) ;
#26330 = DIRECTION ( 'NONE',  ( 0.000000000000000000, 1.000000000000000000, 0.000000000000000000 ) ) ;
#26331 = ORIENTED_EDGE ( 'NONE', *, *, #110716, .F. ) ;
#26332 = DIRECTION ( 'NONE',  ( 0.000000000000000000, 1.000000000000000000, 0.000000000000000000 ) ) ;
#26333 = EDGE_CURVE ( 'NONE', #100404, #2990, #15937, .T. ) ;
#26334 = ORIENTED_EDGE ( 'NONE', *, *, #23375, .F. ) ;
#26335 = DIRECTION ( 'NONE',  ( -0.000000000000000000, -1.000000000000000000, -0.000000000000000000 ) ) ;
#26336 = ORIENTED_EDGE ( 'NONE', *, *, #40722, .F. ) ;
#26337 = DIRECTION ( 'NONE',  ( 0.000000000000000000, 0.000000000000000000, -1.000000000000000000 ) ) ;
#26338 = ORIENTED_EDGE ( 'NONE', *, *, #54845, .T. ) ;
#26339 = EDGE_CURVE ( 'NONE', #120297, #102116, #7282, .T. ) ;
#26340 = ADVANCED_FACE ( 'NONE', ( #6125 ), #25775, .T. ) ;
#26341 = VERTEX_POINT ( 'NONE', #57169 ) ;
#26342 = LINE ( 'NONE', #66245, #23950 ) ;
#26343 = CARTESIAN_POINT ( 'NONE',  ( -11.89999999999999503, 12.50000000000000000, 3.983716857408420076 ) ) ;
#26344 = CIRCLE ( 'NONE', #28401, 0.1000000000000002554 ) ;
#26345 = DIRECTION ( 'NONE',  ( 0.000000000000000000, 0.000000000000000000, 1.000000000000000000 ) ) ;
#26347 = FACE_OUTER_BOUND ( 'NONE', #61603, .T. ) ;
#26346 = AXIS2_PLACEMENT_3D ( 'NONE', #93007, #72712, #101530 ) ;
#26348 = DIRECTION ( 'NONE',  ( 0.000000000000000000, -0.9999939076577903929, 0.003490651415223739937 ) ) ;
#26349 = VERTEX_POINT ( 'NONE', #74886 ) ;
#26350 = LINE ( 'NONE', #63697, #70736 ) ;
#26351 = PLANE ( 'NONE',  #36828 ) ;
#26352 =( REPRESENTATION_RELATIONSHIP ('NONE','NONE', #102928, #71195 ) REPRESENTATION_RELATIONSHIP_WITH_TRANSFORMATION ( #111800 )SHAPE_REPRESENTATION_RELATIONSHIP( ) );
#26353 = EDGE_CURVE ( 'NONE', #33200, #68126, #13635, .T. ) ;
#26354 = DIRECTION ( 'NONE',  ( 0.000000000000000000, 0.000000000000000000, -1.000000000000000000 ) ) ;
#26355 = DIRECTION ( 'NONE',  ( 0.000000000000000000, -0.000000000000000000, 1.000000000000000000 ) ) ;
#26356 = AXIS2_PLACEMENT_3D ( 'NONE', #94168, #23492, #33347 ) ;
#26357 = CARTESIAN_POINT ( 'NONE',  ( -4.150000000000024336, 12.50000000000000000, 1.472243186433545459 ) ) ;
#26358 = ORIENTED_EDGE ( 'NONE', *, *, #88826, .F. ) ;
#26359 = EDGE_LOOP ( 'NONE', ( #22098, #95205, #63547, #46513 ) ) ;
#26360 = VECTOR ( 'NONE', #6211, 1000.000000000000000 ) ;
#26361 = CARTESIAN_POINT ( 'NONE',  ( -8.350000000000012079, 2.500000000000000000, 2.957883832488649389 ) ) ;
#26362 = ORIENTED_EDGE ( 'NONE', *, *, #99245, .T. ) ;
#26363 = CONICAL_SURFACE ( 'NONE', #126706, 0.09999999999999982514, 0.003490658503988666988 ) ;
#26364 = DIRECTION ( 'NONE',  ( -0.000000000000000000, -1.000000000000000000, -0.000000000000000000 ) ) ;
#26365 = CARTESIAN_POINT ( 'NONE',  ( -11.89999999999999680, 12.50000000000000000, -3.983716857408423628 ) ) ;
#26366 = AXIS2_PLACEMENT_3D ( 'NONE', #98136, #68034, #106034 ) ;
#26367 = EDGE_LOOP ( 'NONE', ( #44365, #47601 ) ) ;
#26368 = CARTESIAN_POINT ( 'NONE',  ( 185.0000000000000000, 0.000000000000000000, 7.700000000000000178 ) ) ;
#26369 = CARTESIAN_POINT ( 'NONE',  ( -7.100000000000013856, 2.500000000000000000, 3.637306695894644726 ) ) ;
#26370 = DIRECTION ( 'NONE',  ( -0.000000000000000000, 1.000000000000000000, -0.000000000000000000 ) ) ;
#26371 = CARTESIAN_POINT ( 'NONE',  ( -7.100000000000014744, 2.500000000000000000, 4.230127018922196669 ) ) ;
#26372 = CARTESIAN_POINT ( 'NONE',  ( 2.099999999999950351, 2.500000000000000000, -0.6928203230275541413 ) ) ;
#26373 = VERTEX_POINT ( 'NONE', #114795 ) ;
#26374 = EDGE_CURVE ( 'NONE', #51199, #12366, #1035, .T. ) ;
#26375 = DIRECTION ( 'NONE',  ( -0.000000000000000000, 1.000000000000000000, -0.000000000000000000 ) ) ;
#26376 = CARTESIAN_POINT ( 'NONE',  ( -4.350000000000023626, 2.500000000000000000, 1.718653347947321386 ) ) ;
#26377 = EDGE_LOOP ( 'NONE', ( #81708, #19550, #106611, #116865 ) ) ;
#26378 = EDGE_CURVE ( 'NONE', #71123, #1406, #34508, .T. ) ;
#26379 = FACE_OUTER_BOUND ( 'NONE', #54168, .T. ) ;
#26380 = CIRCLE ( 'NONE', #38929, 0.1000000000000002554 ) ;
#26381 = DIRECTION ( 'NONE',  ( 0.000000000000000000, 0.000000000000000000, 1.000000000000000000 ) ) ;
#26382 = ADVANCED_FACE ( 'NONE', ( #25129 ), #65036, .T. ) ;
#26383 = CARTESIAN_POINT ( 'NONE',  ( 6.249999999999930722, 2.500000000000000000, 1.472243186433545459 ) ) ;
#26384 = ORIENTED_EDGE ( 'NONE', *, *, #15756, .T. ) ;
#26385 = AXIS2_PLACEMENT_3D ( 'NONE', #74621, #94908, #124375 ) ;
#26386 = PLANE ( 'NONE',  #23933 ) ;
#26387 = EDGE_CURVE ( 'NONE', #17860, #77344, #124380, .T. ) ;
#26388 = EDGE_CURVE ( 'NONE', #36126, #92622, #126621, .T. ) ;
#26389 = ORIENTED_EDGE ( 'NONE', *, *, #10116, .F. ) ;
#26390 = FACE_OUTER_BOUND ( 'NONE', #125557, .T. ) ;
#26391 = PLANE ( 'NONE',  #55063 ) ;
#26392 = ADVANCED_FACE ( 'NONE', ( #75511 ), #80560, .T. ) ;
#26393 = AXIS2_PLACEMENT_3D ( 'NONE', #55231, #107548, #37528 ) ;
#26394 = ADVANCED_FACE ( 'NONE', ( #66970 ), #40869, .T. ) ;
#26395 = CARTESIAN_POINT ( 'NONE',  ( 4.999999999999973355, 2.500000000000000000, -4.430127018922202176 ) ) ;
#26396 = CIRCLE ( 'NONE', #15902, 0.09999999999999982514 ) ;
#26397 = ORIENTED_EDGE ( 'NONE', *, *, #40731, .F. ) ;
#26398 = CARTESIAN_POINT ( 'NONE',  ( 1.449999999999952216, 2.500000000000000000, -2.511473670974877948 ) ) ;
#26399 = CIRCLE ( 'NONE', #7501, 0.06509327318403745899 ) ;
#26400 = ADVANCED_FACE ( 'NONE', ( #87899 ), #36900, .T. ) ;
#26401 = DIRECTION ( 'NONE',  ( -0.000000000000000000, 1.000000000000000000, -0.000000000000000000 ) ) ;
#26402 = ORIENTED_EDGE ( 'NONE', *, *, #81135, .F. ) ;
#26403 = VERTEX_POINT ( 'NONE', #17213 ) ;
#26404 = EDGE_CURVE ( 'NONE', #79731, #48343, #116136, .T. ) ;
#26406 = VECTOR ( 'NONE', #125544, 1000.000000000000000 ) ;
#26405 = DIRECTION ( 'NONE',  ( -0.000000000000000000, 1.000000000000000000, -0.000000000000000000 ) ) ;
#26407 = CIRCLE ( 'NONE', #112173, 0.1000000000000000472 ) ;
#26408 = ORIENTED_EDGE ( 'NONE', *, *, #37320, .F. ) ;
#26409 = PLANE ( 'NONE',  #50511 ) ;
#26410 = CARTESIAN_POINT ( 'NONE',  ( -6.450000000000017941, 2.500000000000000000, -2.611473670974877592 ) ) ;
#26411 = ORIENTED_EDGE ( 'NONE', *, *, #97949, .F. ) ;
#26412 = DIRECTION ( 'NONE',  ( 0.000000000000000000, 0.000000000000000000, 1.000000000000000000 ) ) ;
#26413 = CARTESIAN_POINT ( 'NONE',  ( -5.850000000000018296, 2.500000000000000000, 1.472243186433545459 ) ) ;
#26414 = EDGE_LOOP ( 'NONE', ( #41732, #84710 ) ) ;
#26415 = DIRECTION ( 'NONE',  ( -4.274815082592931898E-19, -0.9999939076577903929, -0.003490651415223739937 ) ) ;
#26416 = CARTESIAN_POINT ( 'NONE',  ( -6.650000000000014566, 12.50000000000000000, 6.430097255199259010 ) ) ;
#26417 = CARTESIAN_POINT ( 'NONE',  ( 6.449999999999931788, 12.50000000000000000, -2.446380397790840266 ) ) ;
#26418 = CARTESIAN_POINT ( 'NONE',  ( -10.20000000000000284, 12.50000000000000000, -0.3464101615137782364 ) ) ;
#26419 = FACE_OUTER_BOUND ( 'NONE', #8504, .T. ) ;
#26420 = DIRECTION ( 'NONE',  ( 0.000000000000000000, 0.000000000000000000, 1.000000000000000000 ) ) ;
#26421 = EDGE_LOOP ( 'NONE', ( #67660, #73413, #98808, #117231 ) ) ;
#26422 = VERTEX_POINT ( 'NONE', #126566 ) ;
#26423 = ORIENTED_EDGE ( 'NONE', *, *, #65849, .F. ) ;
#26424 = EDGE_LOOP ( 'NONE', ( #17000, #20360 ) ) ;
#26425 = DIRECTION ( 'NONE',  ( -0.000000000000000000, -1.000000000000000000, -0.000000000000000000 ) ) ;
#26426 = DIRECTION ( 'NONE',  ( 0.000000000000000000, 0.000000000000000000, -1.000000000000000000 ) ) ;
#26427 = DIRECTION ( 'NONE',  ( -0.000000000000000000, 1.000000000000000000, -0.000000000000000000 ) ) ;
#26428 = ORIENTED_EDGE ( 'NONE', *, *, #78090, .T. ) ;
#26429 = FACE_BOUND ( 'NONE', #43201, .T. ) ;
#26430 = LINE ( 'NONE', #15288, #12376 ) ;
#26431 = DIRECTION ( 'NONE',  ( 0.000000000000000000, 1.000000000000000000, 0.000000000000000000 ) ) ;
#26432 = DIRECTION ( 'NONE',  ( -0.000000000000000000, -1.000000000000000000, -0.000000000000000000 ) ) ;
#26433 = CIRCLE ( 'NONE', #124629, 0.1000000000000000056 ) ;
#26434 = EDGE_CURVE ( 'NONE', #30880, #108562, #59735, .T. ) ;
#26435 = DIRECTION ( 'NONE',  ( 0.000000000000000000, 0.000000000000000000, 1.000000000000000000 ) ) ;
#26436 = AXIS2_PLACEMENT_3D ( 'NONE', #69314, #126326, #117120 ) ;
#26437 = DIRECTION ( 'NONE',  ( 0.000000000000000000, 0.000000000000000000, 1.000000000000000000 ) ) ;
#26438 = DIRECTION ( 'NONE',  ( 0.000000000000000000, -0.9999939076577903929, 0.003490651415223739937 ) ) ;
#26439 = DIRECTION ( 'NONE',  ( 0.000000000000000000, 0.000000000000000000, -1.000000000000000000 ) ) ;
#26440 = DIRECTION ( 'NONE',  ( -0.000000000000000000, -1.000000000000000000, -0.000000000000000000 ) ) ;
#26441 = CARTESIAN_POINT ( 'NONE',  ( 13.74999999999993072, 12.50000000000000000, -2.230156782645139391 ) ) ;
#26442 = DIRECTION ( 'NONE',  ( -0.000000000000000000, -1.000000000000000000, -0.000000000000000000 ) ) ;
#26444 = CONICAL_SURFACE ( 'NONE', #120435, 0.09999999999999999167, 0.003490658503988666988 ) ;
#26443 = AXIS2_PLACEMENT_3D ( 'NONE', #32184, #30249, #81880 ) ;
#26445 = EDGE_CURVE ( 'NONE', #36155, #114467, #55511, .T. ) ;
#26446 = ORIENTED_EDGE ( 'NONE', *, *, #42037, .F. ) ;
#26447 = ORIENTED_EDGE ( 'NONE', *, *, #53888, .T. ) ;
#26448 = ORIENTED_EDGE ( 'NONE', *, *, #89382, .F. ) ;
#26449 = VERTEX_POINT ( 'NONE', #97736 ) ;
#26450 = DIRECTION ( 'NONE',  ( -0.000000000000000000, 1.000000000000000000, -0.000000000000000000 ) ) ;
#26451 = ORIENTED_EDGE ( 'NONE', *, *, #93004, .T. ) ;
#26452 = PLANE ( 'NONE',  #123800 ) ;
#26453 = ORIENTED_EDGE ( 'NONE', *, *, #98320, .T. ) ;
#26454 = VERTEX_POINT ( 'NONE', #34982 ) ;
#26455 = CARTESIAN_POINT ( 'NONE',  ( -6.650000000000018119, 2.500000000000000000, -2.857883832488653741 ) ) ;
#26457 = AXIS2_PLACEMENT_3D ( 'NONE', #110100, #91106, #12532 ) ;
#26456 = VECTOR ( 'NONE', #34080, 1000.000000000000000 ) ;
#26458 = AXIS2_PLACEMENT_3D ( 'NONE', #89725, #30180, #70095 ) ;
#26459 = DIRECTION ( 'NONE',  ( -4.274815082592931898E-19, -0.9999939076577903929, -0.003490651415223739937 ) ) ;
#26460 = DIRECTION ( 'NONE',  ( 0.000000000000000000, -0.000000000000000000, 1.000000000000000000 ) ) ;
#26461 = DIRECTION ( 'NONE',  ( 0.000000000000000000, -0.9999939076577903929, 0.003490651415223739937 ) ) ;
#26462 = DIRECTION ( 'NONE',  ( 0.000000000000000000, 0.000000000000000000, 1.000000000000000000 ) ) ;
#26463 = EDGE_LOOP ( 'NONE', ( #37109, #61945, #87932, #62838 ) ) ;
#26464 = ORIENTED_EDGE ( 'NONE', *, *, #111511, .F. ) ;
#26465 = ORIENTED_EDGE ( 'NONE', *, *, #94648, .F. ) ;
#26466 = ORIENTED_EDGE ( 'NONE', *, *, #69688, .F. ) ;
#26467 = DIRECTION ( 'NONE',  ( 0.000000000000000000, -0.9999939076577903929, 0.003490651415223739937 ) ) ;
#26468 = ORIENTED_EDGE ( 'NONE', *, *, #129082, .F. ) ;
#26469 = AXIS2_PLACEMENT_3D ( 'NONE', #38535, #128852, #20157 ) ;
#26470 = ORIENTED_EDGE ( 'NONE', *, *, #69634, .F. ) ;
#26472 = PLANE ( 'NONE',  #19282 ) ;
#26471 = AXIS2_PLACEMENT_3D ( 'NONE', #27083, #125280, #55256 ) ;
#26473 = EDGE_CURVE ( 'NONE', #2289, #23967, #114000, .T. ) ;
#26474 = FACE_OUTER_BOUND ( 'NONE', #29956, .T. ) ;
#26476 = CIRCLE ( 'NONE', #57874, 0.06509327318403745899 ) ;
#26475 = CARTESIAN_POINT ( 'NONE',  ( -5.600000000000020073, 2.500000000000000000, 4.776537180435972196 ) ) ;
#26477 = DIRECTION ( 'NONE',  ( -0.000000000000000000, -1.000000000000000000, -0.000000000000000000 ) ) ;
#26478 = CARTESIAN_POINT ( 'NONE',  ( -6.450000000000019718, 2.500000000000000000, -1.818653347947326138 ) ) ;
#26479 = CONICAL_SURFACE ( 'NONE', #89161, 0.1000000000000002554, 0.003490658503988666988 ) ;
#26480 = DIRECTION ( 'NONE',  ( -0.000000000000000000, 1.000000000000000000, -0.000000000000000000 ) ) ;
#26481 = ORIENTED_EDGE ( 'NONE', *, *, #3200, .T. ) ;
#26483 = AXIS2_PLACEMENT_3D ( 'NONE', #103532, #13841, #33511 ) ;
#26482 = DIRECTION ( 'NONE',  ( 0.000000000000000000, -0.9999939076577903929, 0.003490651415223739937 ) ) ;
#26484 = EDGE_CURVE ( 'NONE', #53810, #47637, #49315, .T. ) ;
#26485 = EDGE_LOOP ( 'NONE', ( #28987, #25712 ) ) ;
#26486 = VECTOR ( 'NONE', #14937, 1000.000000000000000 ) ;
#26487 = FACE_OUTER_BOUND ( 'NONE', #53735, .T. ) ;
#26488 = ORIENTED_EDGE ( 'NONE', *, *, #101270, .F. ) ;
#26489 = FACE_OUTER_BOUND ( 'NONE', #36565, .T. ) ;
#26490 = DIRECTION ( 'NONE',  ( 0.000000000000000000, 0.000000000000000000, -1.000000000000000000 ) ) ;
#26491 = ORIENTED_EDGE ( 'NONE', *, *, #88953, .F. ) ;
#26493 = EDGE_CURVE ( 'NONE', #96953, #40128, #24117, .T. ) ;
#26492 = CARTESIAN_POINT ( 'NONE',  ( 0.6499999999999561684, 12.50000000000000000, 1.818653347947321475 ) ) ;
#26494 = DIRECTION ( 'NONE',  ( 0.000000000000000000, 0.000000000000000000, 1.000000000000000000 ) ) ;
#26495 = EDGE_CURVE ( 'NONE', #117877, #112541, #89210, .T. ) ;
#26496 = VERTEX_POINT ( 'NONE', #129167 ) ;
#26497 = VECTOR ( 'NONE', #15251, 1000.000000000000000 ) ;
#26499 = AXIS2_PLACEMENT_3D ( 'NONE', #83115, #51084, #73277 ) ;
#26498 = AXIS2_PLACEMENT_3D ( 'NONE', #57374, #125462, #65892 ) ;
#26500 = EDGE_CURVE ( 'NONE', #54255, #120320, #22072, .T. ) ;
#26501 = DIRECTION ( 'NONE',  ( 0.000000000000000000, 0.000000000000000000, -1.000000000000000000 ) ) ;
#26502 = ORIENTED_EDGE ( 'NONE', *, *, #40395, .T. ) ;
#26503 = EDGE_LOOP ( 'NONE', ( #31760, #6279 ) ) ;
#26504 = DIRECTION ( 'NONE',  ( -4.274815082592931898E-19, -0.9999939076577903929, -0.003490651415223739937 ) ) ;
#26505 = CARTESIAN_POINT ( 'NONE',  ( -7.100000000000013856, 2.500000000000000000, 5.122947341949749323 ) ) ;
#26506 = EDGE_CURVE ( 'NONE', #3071, #89429, #128702, .T. ) ;
#26507 = CARTESIAN_POINT ( 'NONE',  ( 186.1302083336747444, -4.367472073101514418, -7.564683531250002702 ) ) ;
#26508 = DIRECTION ( 'NONE',  ( -0.000000000000000000, -1.000000000000000000, -0.000000000000000000 ) ) ;
#26509 = CARTESIAN_POINT ( 'NONE',  ( -13.74999999999998934, 12.50000000000000000, 2.857883832488652853 ) ) ;
#26510 = DIRECTION ( 'NONE',  ( 0.000000000000000000, -0.000000000000000000, 1.000000000000000000 ) ) ;
#26511 = AXIS2_PLACEMENT_3D ( 'NONE', #86130, #63943, #85511 ) ;
#26512 = ORIENTED_EDGE ( 'NONE', *, *, #58446, .T. ) ;
#26513 = DIRECTION ( 'NONE',  ( -0.000000000000000000, -1.000000000000000000, -0.000000000000000000 ) ) ;
#26514 = EDGE_LOOP ( 'NONE', ( #58663, #124004 ) ) ;
#26515 = CARTESIAN_POINT ( 'NONE',  ( -4.400000000000025224, 12.50000000000000000, 4.741630453620009789 ) ) ;
#26516 = DIRECTION ( 'NONE',  ( 0.000000000000000000, -0.000000000000000000, 1.000000000000000000 ) ) ;
#26517 = CARTESIAN_POINT ( 'NONE',  ( -6.900000000000015454, 2.500000000000000000, 4.676537180435972552 ) ) ;
#26518 = EDGE_LOOP ( 'NONE', ( #46587, #64317 ) ) ;
#26519 = VECTOR ( 'NONE', #53014, 1000.000000000000000 ) ;
#26520 = CIRCLE ( 'NONE', #62129, 0.06509327318403745899 ) ;
#26521 = CARTESIAN_POINT ( 'NONE',  ( 8.549999999999922551, 2.500000000000000000, -6.148780366869526226 ) ) ;
#26522 = CARTESIAN_POINT ( 'NONE',  ( 8.349999999999919709, 2.500000000000000000, -1.472243186433550122 ) ) ;
#26523 = ORIENTED_EDGE ( 'NONE', *, *, #22518, .F. ) ;
#26525 = AXIS2_PLACEMENT_3D ( 'NONE', #30934, #62949, #72138 ) ;
#26524 = AXIS2_PLACEMENT_3D ( 'NONE', #109266, #110559, #20251 ) ;
#26526 = CARTESIAN_POINT ( 'NONE',  ( 0.1999999999999576006, 12.50000000000000000, -4.611443907251940644 ) ) ;
#26527 = VERTEX_POINT ( 'NONE', #70222 ) ;
#26528 = VERTEX_POINT ( 'NONE', #29651 ) ;
#26529 = DIRECTION ( 'NONE',  ( 0.000000000000000000, -0.000000000000000000, 1.000000000000000000 ) ) ;
#26530 = EDGE_CURVE ( 'NONE', #115201, #137, #20011, .T. ) ;
#26531 = EDGE_CURVE ( 'NONE', #120872, #42274, #97268, .T. ) ;
#26532 = ORIENTED_EDGE ( 'NONE', *, *, #81790, .F. ) ;
#26533 = DIRECTION ( 'NONE',  ( 0.000000000000000000, 0.000000000000000000, 1.000000000000000000 ) ) ;
#26535 = EDGE_CURVE ( 'NONE', #13812, #82111, #34603, .T. ) ;
#26534 = DIRECTION ( 'NONE',  ( -4.274815082592931898E-19, -0.9999939076577903929, -0.003490651415223739937 ) ) ;
#26537 = ADVANCED_FACE ( 'NONE', ( #90484 ), #127845, .T. ) ;
#26536 = AXIS2_PLACEMENT_3D ( 'NONE', #119541, #104724, #77681 ) ;
#26538 = DIRECTION ( 'NONE',  ( -0.000000000000000000, 1.000000000000000000, -0.000000000000000000 ) ) ;
#26539 = EDGE_LOOP ( 'NONE', ( #119856, #97790, #124865, #117989 ) ) ;
#26540 = AXIS2_PLACEMENT_3D ( 'NONE', #23185, #51390, #99838 ) ;
#26541 = FACE_BOUND ( 'NONE', #124401, .T. ) ;
#26542 = EDGE_CURVE ( 'NONE', #1788, #40995, #48649, .T. ) ;
#26544 = VERTEX_POINT ( 'NONE', #40784 ) ;
#26543 = LINE ( 'NONE', #67071, #66715 ) ;
#26545 = DIRECTION ( 'NONE',  ( -4.274815082592931898E-19, -0.9999939076577903929, -0.003490651415223739937 ) ) ;
#26546 = DIRECTION ( 'NONE',  ( 0.000000000000000000, 1.000000000000000000, 0.000000000000000000 ) ) ;
#26547 = ORIENTED_EDGE ( 'NONE', *, *, #15606, .F. ) ;
#26548 = EDGE_CURVE ( 'NONE', #47717, #69367, #108838, .T. ) ;
#26549 = EDGE_CURVE ( 'NONE', #95831, #10375, #167, .T. ) ;
#26550 = ORIENTED_EDGE ( 'NONE', *, *, #96694, .T. ) ;
#26551 = ORIENTED_EDGE ( 'NONE', *, *, #27127, .T. ) ;
#26552 = DIRECTION ( 'NONE',  ( 0.000000000000000000, 1.000000000000000000, 0.000000000000000000 ) ) ;
#26553 = CARTESIAN_POINT ( 'NONE',  ( -8.749999999999975131, 12.50000000000000000, 2.165063509461097713 ) ) ;
#26554 = CARTESIAN_POINT ( 'NONE',  ( 4.549999999999935874, 12.50000000000000000, 6.495190528383297135 ) ) ;
#26555 = FACE_BOUND ( 'NONE', #14511, .T. ) ;
#26556 = ORIENTED_EDGE ( 'NONE', *, *, #116498, .T. ) ;
#26557 = CIRCLE ( 'NONE', #97558, 0.1000000000000002554 ) ;
#26558 = CARTESIAN_POINT ( 'NONE',  ( 185.6927083336747160, 6.551208109652275624, -3.782341765624998686 ) ) ;
#26559 = VECTOR ( 'NONE', #113197, 1000.000000000000000 ) ;
#26560 = DIRECTION ( 'NONE',  ( 0.000000000000000000, 1.000000000000000000, 0.000000000000000000 ) ) ;
#26561 = CARTESIAN_POINT ( 'NONE',  ( -13.34999999999999076, 12.50000000000000000, 2.165063509461101265 ) ) ;
#26562 = AXIS2_PLACEMENT_3D ( 'NONE', #76673, #96941, #87123 ) ;
#26563 = CARTESIAN_POINT ( 'NONE',  ( -1.850000000000033840, 2.500000000000000000, 6.741600689897071952 ) ) ;
#26564 = AXIS2_PLACEMENT_3D ( 'NONE', #116051, #64998, #76132 ) ;
#26565 = DIRECTION ( 'NONE',  ( 0.000000000000000000, -0.000000000000000000, 1.000000000000000000 ) ) ;
#26566 = DIRECTION ( 'NONE',  ( 0.000000000000000000, -0.000000000000000000, 1.000000000000000000 ) ) ;
#26567 = DIRECTION ( 'NONE',  ( -0.000000000000000000, 1.000000000000000000, -0.000000000000000000 ) ) ;
#26568 = CIRCLE ( 'NONE', #110094, 0.06509327318403745899 ) ;
#26569 = CARTESIAN_POINT ( 'NONE',  ( 9.149999999999916866, 2.500000000000000000, 7.188010851410848723 ) ) ;
#26570 = AXIS2_PLACEMENT_3D ( 'NONE', #86784, #44944, #46219 ) ;
#26571 = DIRECTION ( 'NONE',  ( -0.000000000000000000, -1.000000000000000000, -0.000000000000000000 ) ) ;
#26572 = CIRCLE ( 'NONE', #74596, 0.1000000000000000472 ) ;
#26573 = ORIENTED_EDGE ( 'NONE', *, *, #68946, .T. ) ;
#26574 = ORIENTED_EDGE ( 'NONE', *, *, #10283, .T. ) ;
#26575 = ORIENTED_EDGE ( 'NONE', *, *, #31527, .T. ) ;
#26576 = VERTEX_POINT ( 'NONE', #88558 ) ;
#26577 = ORIENTED_EDGE ( 'NONE', *, *, #12360, .T. ) ;
#26578 = DIRECTION ( 'NONE',  ( -4.274815082592931898E-19, -0.9999939076577903929, -0.003490651415223739937 ) ) ;
#26579 = CARTESIAN_POINT ( 'NONE',  ( 2.049999999999950084, 2.500000000000000000, -6.395190528383301931 ) ) ;
#26580 = AXIS2_PLACEMENT_3D ( 'NONE', #23544, #62834, #42571 ) ;
#26581 = VERTEX_POINT ( 'NONE', #100329 ) ;
#26582 = FACE_BOUND ( 'NONE', #3885, .T. ) ;
#26584 = CARTESIAN_POINT ( 'NONE',  ( -11.89999999999999680, 12.50000000000000000, -3.983716857408423628 ) ) ;
#26583 = CIRCLE ( 'NONE', #101803, 0.06509327318403745899 ) ;
#26585 = CONICAL_SURFACE ( 'NONE', #30803, 0.1000000000000002554, 0.003490658503988666988 ) ;
#26586 = DIRECTION ( 'NONE',  ( -0.000000000000000000, -1.000000000000000000, -0.000000000000000000 ) ) ;
#26587 = DIRECTION ( 'NONE',  ( -0.000000000000000000, -1.000000000000000000, -0.000000000000000000 ) ) ;
#26588 = DIRECTION ( 'NONE',  ( -0.000000000000000000, 1.000000000000000000, -0.000000000000000000 ) ) ;
#26589 = DIRECTION ( 'NONE',  ( 0.000000000000000000, 0.000000000000000000, 1.000000000000000000 ) ) ;
#26590 = EDGE_LOOP ( 'NONE', ( #68858, #41799, #119359, #2877 ) ) ;
#26591 = CARTESIAN_POINT ( 'NONE',  ( 16.32360670575004491, -2.500000000000000000, 4.874197301685487815 ) ) ;
#26592 = ORIENTED_EDGE ( 'NONE', *, *, #35766, .F. ) ;
#26593 = EDGE_CURVE ( 'NONE', #125242, #59372, #57578, .T. ) ;
#26594 = VERTEX_POINT ( 'NONE', #49958 ) ;
#26595 = EDGE_LOOP ( 'NONE', ( #68809, #24883, #49799, #34005 ) ) ;
#26596 = DIRECTION ( 'NONE',  ( -0.000000000000000000, 1.000000000000000000, -0.000000000000000000 ) ) ;
#26597 = DIRECTION ( 'NONE',  ( -0.000000000000000000, 1.000000000000000000, -0.000000000000000000 ) ) ;
#26598 = CARTESIAN_POINT ( 'NONE',  ( 0.8499999999999553468, 2.500000000000000000, 1.472243186433545459 ) ) ;
#26599 = ORIENTED_EDGE ( 'NONE', *, *, #30228, .F. ) ;
#26600 = CIRCLE ( 'NONE', #7704, 0.06509327318403745899 ) ;
#26601 = LINE ( 'NONE', #66508, #87205 ) ;
#26602 = LINE ( 'NONE', #66511, #63724 ) ;
#26603 = DIRECTION ( 'NONE',  ( -0.000000000000000000, 1.000000000000000000, -0.000000000000000000 ) ) ;
#26604 = CARTESIAN_POINT ( 'NONE',  ( 184.6562500006828031, 8.891194145520236347, 5.444286225454521982E-16 ) ) ;
#26605 = CARTESIAN_POINT ( 'NONE',  ( -12.89999999999999147, 12.50000000000000000, 3.637306695894644726 ) ) ;
#26606 = DIRECTION ( 'NONE',  ( 0.000000000000000000, 0.000000000000000000, 1.000000000000000000 ) ) ;
#26607 = EDGE_LOOP ( 'NONE', ( #79685, #16950, #6915, #87391 ) ) ;
#26608 = CARTESIAN_POINT ( 'NONE',  ( -3.100000000000028511, 12.50000000000000000, -4.048810130592463530 ) ) ;
#26609 = CONICAL_SURFACE ( 'NONE', #68366, 0.1000000000000002554, 0.003490658503988666988 ) ;
#26610 = VERTEX_POINT ( 'NONE', #89849 ) ;
#26611 = AXIS2_PLACEMENT_3D ( 'NONE', #93185, #92518, #42812 ) ;
#26612 = ORIENTED_EDGE ( 'NONE', *, *, #2401, .T. ) ;
#26613 = CARTESIAN_POINT ( 'NONE',  ( 107.5000000000000142, 0.000000000000000000, 0.000000000000000000 ) ) ;
#26614 = CARTESIAN_POINT ( 'NONE',  ( -7.300000000000018474, 2.500000000000000000, 0.2464101615137735679 ) ) ;
#26615 = DIRECTION ( 'NONE',  ( -0.000000000000000000, 1.000000000000000000, -0.000000000000000000 ) ) ;
#26616 = ORIENTED_EDGE ( 'NONE', *, *, #32378, .T. ) ;
#26619 = VERTEX_POINT ( 'NONE', #78769 ) ;
#26618 = CIRCLE ( 'NONE', #68374, 0.09999999999999982514 ) ;
#26617 = AXIS2_PLACEMENT_3D ( 'NONE', #88992, #108622, #39280 ) ;
#26620 = DIRECTION ( 'NONE',  ( 0.000000000000000000, 1.000000000000000000, 0.000000000000000000 ) ) ;
#26621 = CIRCLE ( 'NONE', #108174, 0.06509327318403743123 ) ;
#26622 = CARTESIAN_POINT ( 'NONE',  ( 8.949999999999917577, 2.500000000000000000, -2.611473670974877592 ) ) ;
#26623 = FACE_OUTER_BOUND ( 'NONE', #45978, .T. ) ;
#26624 = VERTEX_POINT ( 'NONE', #80694 ) ;
#26625 = VERTEX_POINT ( 'NONE', #68922 ) ;
#26626 = DIRECTION ( 'NONE',  ( -4.274815082592931898E-19, -0.9999939076577903929, -0.003490651415223739937 ) ) ;
#26627 = AXIS2_PLACEMENT_3D ( 'NONE', #10248, #32493, #1703 ) ;
#26628 = ORIENTED_EDGE ( 'NONE', *, *, #30506, .F. ) ;
#26629 = DIRECTION ( 'NONE',  ( 0.000000000000000000, 0.000000000000000000, -1.000000000000000000 ) ) ;
#26631 = EDGE_CURVE ( 'NONE', #92524, #35250, #80037, .T. ) ;
#26630 = CONICAL_SURFACE ( 'NONE', #101846, 0.1000000000000002554, 0.003490658503988666988 ) ;
#26632 = DIRECTION ( 'NONE',  ( 0.000000000000000000, 0.000000000000000000, 1.000000000000000000 ) ) ;
#26633 = VERTEX_POINT ( 'NONE', #9364 ) ;
#26634 = CARTESIAN_POINT ( 'NONE',  ( -5.400000000000019895, 2.500000000000000000, 4.430127018922196847 ) ) ;
#26635 = CARTESIAN_POINT ( 'NONE',  ( 7.949999999999922018, 12.50000000000000000, 6.495190528383297135 ) ) ;
#26636 = DIRECTION ( 'NONE',  ( 0.000000000000000000, 1.000000000000000000, 0.000000000000000000 ) ) ;
#26637 = EDGE_CURVE ( 'NONE', #49409, #8476, #119964, .T. ) ;
#26638 = DIRECTION ( 'NONE',  ( -0.000000000000000000, 1.000000000000000000, -0.000000000000000000 ) ) ;
#26639 = EDGE_CURVE ( 'NONE', #23744, #112624, #70865, .T. ) ;
#26640 = EDGE_LOOP ( 'NONE', ( #18304, #11001 ) ) ;
#26642 = CONICAL_SURFACE ( 'NONE', #47580, 0.09999999999999982514, 0.003490658503988666988 ) ;
#26641 = DIRECTION ( 'NONE',  ( -0.000000000000000000, -1.000000000000000000, -0.000000000000000000 ) ) ;
#26643 = CARTESIAN_POINT ( 'NONE',  ( -10.85000000000000142, 12.50000000000000000, 2.099970236277060032 ) ) ;
#26644 = AXIS2_PLACEMENT_3D ( 'NONE', #15318, #34355, #64431 ) ;
#26645 = EDGE_CURVE ( 'NONE', #75709, #40954, #42053, .T. ) ;
#26646 = EDGE_LOOP ( 'NONE', ( #66835, #22642 ) ) ;
#26647 = ADVANCED_FACE ( 'NONE', ( #103555 ), #1120, .T. ) ;
#26648 = EDGE_LOOP ( 'NONE', ( #75190, #111674 ) ) ;
#26649 = EDGE_CURVE ( 'NONE', #24362, #75483, #63831, .T. ) ;
#26650 = CARTESIAN_POINT ( 'NONE',  ( 185.6718750003414016, 9.264065473108010111E-16, -7.564683531250000925 ) ) ;
#26652 = EDGE_CURVE ( 'NONE', #75419, #125967, #2104, .T. ) ;
#26651 = DIRECTION ( 'NONE',  ( 0.000000000000000000, -0.000000000000000000, 1.000000000000000000 ) ) ;
#26653 = CARTESIAN_POINT ( 'NONE',  ( 2.500000000000002220, 1.499999999999999334, 10.00000000000000178 ) ) ;
#26654 = EDGE_CURVE ( 'NONE', #3051, #97481, #122547, .T. ) ;
#26655 = CARTESIAN_POINT ( 'NONE',  ( -3.150000000000033218, 12.50000000000000000, -6.841600689897078702 ) ) ;
#26656 = CIRCLE ( 'NONE', #49652, 0.06509327318403745899 ) ;
#26657 = FACE_OUTER_BOUND ( 'NONE', #99553, .T. ) ;
#26658 = FACE_OUTER_BOUND ( 'NONE', #14856, .T. ) ;
#26659 = DIRECTION ( 'NONE',  ( 0.000000000000000000, -0.000000000000000000, 1.000000000000000000 ) ) ;
#26660 = DIRECTION ( 'NONE',  ( 0.000000000000000000, 0.000000000000000000, -1.000000000000000000 ) ) ;
#26661 = FACE_OUTER_BOUND ( 'NONE', #69533, .T. ) ;
#26662 = ADVANCED_FACE ( 'NONE', ( #83270 ), #72163, .T. ) ;
#26663 = AXIS2_PLACEMENT_3D ( 'NONE', #49470, #128006, #10779 ) ;
#26664 = DIRECTION ( 'NONE',  ( 0.000000000000000000, 1.000000000000000000, 0.000000000000000000 ) ) ;
#26665 = EDGE_LOOP ( 'NONE', ( #83174, #59887 ) ) ;
#26666 = AXIS2_PLACEMENT_3D ( 'NONE', #75903, #5224, #86359 ) ;
#26667 = AXIS2_PLACEMENT_3D ( 'NONE', #28143, #88320, #6519 ) ;
#26668 = ORIENTED_EDGE ( 'NONE', *, *, #6268, .T. ) ;
#26669 = CARTESIAN_POINT ( 'NONE',  ( 11.04999999999991012, 2.500000000000000000, -1.818653347947326138 ) ) ;
#26670 = ORIENTED_EDGE ( 'NONE', *, *, #71686, .F. ) ;
#26671 = DIRECTION ( 'NONE',  ( -4.274815082592931898E-19, -0.9999939076577903929, -0.003490651415223739937 ) ) ;
#26672 = FACE_OUTER_BOUND ( 'NONE', #107663, .T. ) ;
#26673 = CARTESIAN_POINT ( 'NONE',  ( -6.850000000000013856, 2.500000000000000000, 1.818653347947321475 ) ) ;
#26674 = ORIENTED_EDGE ( 'NONE', *, *, #47124, .F. ) ;
#26675 = CARTESIAN_POINT ( 'NONE',  ( 13.74999999999989342, 12.50000000000000000, -1.472243186433550122 ) ) ;
#26676 = DIRECTION ( 'NONE',  ( 0.000000000000000000, 0.000000000000000000, -1.000000000000000000 ) ) ;
#26678 = VERTEX_POINT ( 'NONE', #123811 ) ;
#26677 = DIRECTION ( 'NONE',  ( 0.000000000000000000, 0.000000000000000000, 1.000000000000000000 ) ) ;
#26679 = CARTESIAN_POINT ( 'NONE',  ( 8.749999999999921840, 2.500000000000000000, -5.702370205355749455 ) ) ;
#26680 = EDGE_LOOP ( 'NONE', ( #119051, #81086 ) ) ;
#26681 = VERTEX_POINT ( 'NONE', #4040 ) ;
#26682 = VERTEX_POINT ( 'NONE', #112080 ) ;
#26683 = ORIENTED_EDGE ( 'NONE', *, *, #88795, .F. ) ;
#26684 = CARTESIAN_POINT ( 'NONE',  ( 8.349999999999919709, 12.50000000000000000, -2.857883832488653741 ) ) ;
#26685 = EDGE_CURVE ( 'NONE', #48167, #77843, #122418, .T. ) ;
#26686 = CIRCLE ( 'NONE', #14147, 0.06509327318403743123 ) ;
#26687 = PLANE ( 'NONE',  #50980 ) ;
#26689 = EDGE_CURVE ( 'NONE', #47998, #50950, #53792, .T. ) ;
#26688 = DIRECTION ( 'NONE',  ( 0.000000000000000000, 1.000000000000000000, 0.000000000000000000 ) ) ;
#26690 = DIRECTION ( 'NONE',  ( 0.000000000000000000, 0.000000000000000000, 1.000000000000000000 ) ) ;
#26691 = ORIENTED_EDGE ( 'NONE', *, *, #119322, .F. ) ;
#26692 = ADVANCED_FACE ( 'NONE', ( #33529 ), #124460, .T. ) ;
#26693 = PLANE ( 'NONE',  #64890 ) ;
#26694 = ORIENTED_EDGE ( 'NONE', *, *, #10991, .F. ) ;
#26695 = CARTESIAN_POINT ( 'NONE',  ( 32.15727368891349158, -2.842525632570966909, -4.549395963660428421 ) ) ;
#26696 = LINE ( 'NONE', #7680, #89446 ) ;
#26697 = DIRECTION ( 'NONE',  ( 0.000000000000000000, -0.000000000000000000, 1.000000000000000000 ) ) ;
#26698 = CARTESIAN_POINT ( 'NONE',  ( 16.53754090007008770, -0.4856821978169225673, 6.114873053042319206 ) ) ;
#26699 = EDGE_CURVE ( 'NONE', #70253, #37568, #92430, .T. ) ;
#26700 = ADVANCED_FACE ( 'NONE', ( #104185 ), #111954, .T. ) ;
#26701 = EDGE_LOOP ( 'NONE', ( #70362, #46423, #80679, #24396 ) ) ;
#26703 = ADVANCED_FACE ( 'NONE', ( #13212 ), #81962, .T. ) ;
#26702 = VECTOR ( 'NONE', #92789, 1000.000000000000000 ) ;
#26704 = AXIS2_PLACEMENT_3D ( 'NONE', #67552, #119898, #117949 ) ;
#26705 = EDGE_CURVE ( 'NONE', #119406, #65807, #45059, .T. ) ;
#26706 = ORIENTED_EDGE ( 'NONE', *, *, #76930, .T. ) ;
#26707 = ORIENTED_EDGE ( 'NONE', *, *, #104129, .T. ) ;
#26708 = DIRECTION ( 'NONE',  ( 0.000000000000000000, 0.000000000000000000, 1.000000000000000000 ) ) ;
#26709 = FACE_OUTER_BOUND ( 'NONE', #49765, .T. ) ;
#26710 = CARTESIAN_POINT ( 'NONE',  ( -13.34999999999999076, 2.500000000000000000, 2.065063509461101621 ) ) ;
#26711 = FACE_BOUND ( 'NONE', #92932, .T. ) ;
#26712 = DIRECTION ( 'NONE',  ( 0.000000000000000000, 0.000000000000000000, 1.000000000000000000 ) ) ;
#26713 = DIRECTION ( 'NONE',  ( 0.000000000000000000, 0.000000000000000000, 1.000000000000000000 ) ) ;
#26714 = EDGE_CURVE ( 'NONE', #87768, #104203, #121893, .T. ) ;
#26715 = AXIS2_PLACEMENT_3D ( 'NONE', #111971, #72048, #101503 ) ;
#26716 = DIRECTION ( 'NONE',  ( 0.000000000000000000, 0.000000000000000000, 1.000000000000000000 ) ) ;
#26717 = CARTESIAN_POINT ( 'NONE',  ( -10.45000000000000107, 2.500000000000000000, 2.065063509461097624 ) ) ;
#26718 = AXIS2_PLACEMENT_3D ( 'NONE', #7432, #29035, #18547 ) ;
#26719 = CARTESIAN_POINT ( 'NONE',  ( 185.7968750003414300, 8.734944146203032389, 5.348610694689227483E-16 ) ) ;
#26720 = CARTESIAN_POINT ( 'NONE',  ( 10.39999999999991331, 2.500000000000000000, -2.385244779468109755E-15 ) ) ;
#26721 = CARTESIAN_POINT ( 'NONE',  ( 12.89999999999989910, 2.500000000000000000, -0.6928203230275542523 ) ) ;
#26722 = AXIS2_PLACEMENT_3D ( 'NONE', #123183, #82619, #33519 ) ;
#26723 = LINE ( 'NONE', #87560, #51683 ) ;
#26724 = VERTEX_POINT ( 'NONE', #121252 ) ;
#26725 = ORIENTED_EDGE ( 'NONE', *, *, #21037, .F. ) ;
#26726 = ORIENTED_EDGE ( 'NONE', *, *, #1179, .T. ) ;
#26727 = EDGE_LOOP ( 'NONE', ( #119706, #48181, #55827, #53966 ) ) ;
#26728 = FACE_OUTER_BOUND ( 'NONE', #10876, .T. ) ;
#26729 = EDGE_CURVE ( 'NONE', #5370, #127196, #111411, .T. ) ;
#26730 = FACE_BOUND ( 'NONE', #12871, .T. ) ;
#26731 = DIRECTION ( 'NONE',  ( 0.000000000000000000, 1.000000000000000000, 0.000000000000000000 ) ) ;
#26732 = CARTESIAN_POINT ( 'NONE',  ( 1.249999999999952038, 12.50000000000000000, 2.857883832488649301 ) ) ;
#26733 = AXIS2_PLACEMENT_3D ( 'NONE', #13159, #123142, #126853 ) ;
#26734 = ORIENTED_EDGE ( 'NONE', *, *, #117792, .F. ) ;
#26735 = DIRECTION ( 'NONE',  ( -0.000000000000000000, -1.000000000000000000, -0.000000000000000000 ) ) ;
#26736 = FACE_OUTER_BOUND ( 'NONE', #3537, .T. ) ;
#26737 = AXIS2_PLACEMENT_3D ( 'NONE', #43382, #103582, #22457 ) ;
#26738 = ORIENTED_EDGE ( 'NONE', *, *, #111770, .F. ) ;
#26739 = DIRECTION ( 'NONE',  ( 0.000000000000000000, 0.000000000000000000, 1.000000000000000000 ) ) ;
#26740 = CIRCLE ( 'NONE', #91586, 0.06509327318403745899 ) ;
#26741 = DIRECTION ( 'NONE',  ( 0.000000000000000000, 0.000000000000000000, 1.000000000000000000 ) ) ;
#26742 = CIRCLE ( 'NONE', #101963, 0.06509327318403745899 ) ;
#26743 = EDGE_CURVE ( 'NONE', #123664, #68434, #72053, .T. ) ;
#26744 = EDGE_LOOP ( 'NONE', ( #19866, #63870 ) ) ;
#26745 = CARTESIAN_POINT ( 'NONE',  ( -8.550000000000013145, 2.500000000000000000, -6.841600689897073373 ) ) ;
#26746 = CARTESIAN_POINT ( 'NONE',  ( -13.94999999999998863, 12.50000000000000000, 2.576566944158914740 ) ) ;
#26747 = CIRCLE ( 'NONE', #12072, 0.06509327318403745899 ) ;
#26748 = CONICAL_SURFACE ( 'NONE', #70381, 0.1000000000000002554, 0.003490658503988666988 ) ;
#26749 = ORIENTED_EDGE ( 'NONE', *, *, #92145, .T. ) ;
#26750 = CIRCLE ( 'NONE', #93655, 0.09999999999999982514 ) ;
#26751 = LINE ( 'NONE', #39178, #101277 ) ;
#26752 = PLANE ( 'NONE',  #89602 ) ;
#26753 = ORIENTED_EDGE ( 'NONE', *, *, #42280, .F. ) ;
#26754 = CARTESIAN_POINT ( 'NONE',  ( -11.25000000000000000, 2.500000000000000000, 2.957883832488649389 ) ) ;
#26755 = EDGE_LOOP ( 'NONE', ( #120071, #39704 ) ) ;
#26756 = EDGE_LOOP ( 'NONE', ( #75788, #66354 ) ) ;
#26757 = CIRCLE ( 'NONE', #116633, 0.06509327318403745899 ) ;
#26758 = EDGE_CURVE ( 'NONE', #12831, #2276, #97359, .T. ) ;
#26759 = DIRECTION ( 'NONE',  ( -0.000000000000000000, 1.000000000000000000, -0.000000000000000000 ) ) ;
#26760 = ORIENTED_EDGE ( 'NONE', *, *, #92525, .T. ) ;
#26761 = CARTESIAN_POINT ( 'NONE',  ( 13.74999999999989875, 12.50000000000000000, 1.537336459617582918 ) ) ;
#26762 = CARTESIAN_POINT ( 'NONE',  ( 3.349999999999943689, 2.500000000000000000, 2.165063509461097713 ) ) ;
#26764 = AXIS2_PLACEMENT_3D ( 'NONE', #68443, #99215, #88060 ) ;
#26763 = AXIS2_PLACEMENT_3D ( 'NONE', #117902, #70592, #86510 ) ;
#26765 = ORIENTED_EDGE ( 'NONE', *, *, #32122, .T. ) ;
#26766 = PLANE ( 'NONE',  #120730 ) ;
#26767 = DIRECTION ( 'NONE',  ( -4.274815082592931898E-19, -0.9999939076577903929, -0.003490651415223739937 ) ) ;
#26768 = DIRECTION ( 'NONE',  ( 0.000000000000000000, 0.000000000000000000, 1.000000000000000000 ) ) ;
#26769 = CARTESIAN_POINT ( 'NONE',  ( -6.650000000000018119, 2.500000000000000000, -2.265063509461101798 ) ) ;
#26770 = CARTESIAN_POINT ( 'NONE',  ( -2.900000000000030109, 2.500000000000000000, 0.6928203230275494784 ) ) ;
#26771 = CARTESIAN_POINT ( 'NONE',  ( 17.50000000000000000, 2.500000000000000000, -2.922290670089280340 ) ) ;
#26772 = EDGE_LOOP ( 'NONE', ( #28512, #123108, #38210, #65440 ) ) ;
#26773 = VERTEX_POINT ( 'NONE', #53164 ) ;
#26774 = DIRECTION ( 'NONE',  ( -0.000000000000000000, -1.000000000000000000, -0.000000000000000000 ) ) ;
#26775 = CARTESIAN_POINT ( 'NONE',  ( 19.52519901027821803, -0.5909487300084481642, 4.333354523369975730 ) ) ;
#26776 = DIRECTION ( 'NONE',  ( 0.000000000000000000, 0.000000000000000000, -1.000000000000000000 ) ) ;
#26778 = ORIENTED_EDGE ( 'NONE', *, *, #117868, .F. ) ;
#26777 = ORIENTED_EDGE ( 'NONE', *, *, #34528, .F. ) ;
#26779 = ORIENTED_EDGE ( 'NONE', *, *, #50906, .F. ) ;
#26780 = CARTESIAN_POINT ( 'NONE',  ( -6.250000000000017764, 2.500000000000000000, 2.757883832488649656 ) ) ;
#26781 = DIRECTION ( 'NONE',  ( 0.000000000000000000, 0.000000000000000000, 1.000000000000000000 ) ) ;
#26782 = CARTESIAN_POINT ( 'NONE',  ( 3.949999999999938893, 12.50000000000000000, 6.148780366869520009 ) ) ;
#26783 = EDGE_CURVE ( 'NONE', #75562, #76998, #26279, .T. ) ;
#26784 = PRODUCT_CONTEXT ( 'NONE', #51407, 'mechanical' ) ;
#26785 = DIRECTION ( 'NONE',  ( -4.274815082592931898E-19, -0.9999939076577903929, -0.003490651415223739937 ) ) ;
#26786 = CARTESIAN_POINT ( 'NONE',  ( 187.1666666666666856, -6.668395609140176816, -3.850000000000003642 ) ) ;
#26787 = AXIS2_PLACEMENT_3D ( 'NONE', #70709, #61548, #20964 ) ;
#26788 = DIRECTION ( 'NONE',  ( -0.000000000000000000, -1.000000000000000000, -0.000000000000000000 ) ) ;
#26789 = DIRECTION ( 'NONE',  ( -0.000000000000000000, 1.000000000000000000, -0.000000000000000000 ) ) ;
#26790 = DIRECTION ( 'NONE',  ( 0.000000000000000000, 1.000000000000000000, 0.000000000000000000 ) ) ;
#26791 = AXIS2_PLACEMENT_3D ( 'NONE', #12247, #82946, #40456 ) ;
#26792 = CARTESIAN_POINT ( 'NONE',  ( -8.300000000000009592, 2.500000000000000000, 4.230127018922196669 ) ) ;
#26793 = ADVANCED_FACE ( 'NONE', ( #4666 ), #65547, .T. ) ;
#26795 = ORIENTED_EDGE ( 'NONE', *, *, #89891, .F. ) ;
#26794 = VECTOR ( 'NONE', #83920, 1000.000000000000000 ) ;
#26796 = DIRECTION ( 'NONE',  ( -0.000000000000000000, 1.000000000000000000, -0.000000000000000000 ) ) ;
#26797 = EDGE_CURVE ( 'NONE', #94293, #98576, #101287, .T. ) ;
#26798 = ORIENTED_EDGE ( 'NONE', *, *, #22890, .T. ) ;
#26799 = ADVANCED_FACE ( 'NONE', ( #7252 ), #106119, .T. ) ;
#26800 = VERTEX_POINT ( 'NONE', #77300 ) ;
#26801 = ADVANCED_FACE ( 'NONE', ( #114640 ), #76011, .T. ) ;
#26802 = LINE ( 'NONE', #66710, #77638 ) ;
#26804 = EDGE_CURVE ( 'NONE', #109687, #10308, #34412, .T. ) ;
#26803 = DIRECTION ( 'NONE',  ( 0.000000000000000000, 0.000000000000000000, 1.000000000000000000 ) ) ;
#26805 = CARTESIAN_POINT ( 'NONE',  ( -13.54999999999998828, 2.500000000000000000, 1.818653347947325472 ) ) ;
#26806 = AXIS2_PLACEMENT_3D ( 'NONE', #94153, #16214, #74523 ) ;
#26807 = DIRECTION ( 'NONE',  ( -0.000000000000000000, 1.000000000000000000, -0.000000000000000000 ) ) ;
#26808 = CONICAL_SURFACE ( 'NONE', #83250, 0.1000000000000002554, 0.003490658503988666988 ) ;
#26809 = CARTESIAN_POINT ( 'NONE',  ( 3.099999999999943245, 12.50000000000000000, 3.918623584224382839 ) ) ;
#26810 = CARTESIAN_POINT ( 'NONE',  ( 5.399999999999936406, 2.500000000000000000, -5.022947341949754119 ) ) ;
#26811 = CARTESIAN_POINT ( 'NONE',  ( 9.199999999999915801, 12.50000000000000000, 4.330127018922196314 ) ) ;
#26812 = VERTEX_POINT ( 'NONE', #115936 ) ;
#26813 = DIRECTION ( 'NONE',  ( -0.000000000000000000, 1.000000000000000000, -0.000000000000000000 ) ) ;
#26814 = EDGE_CURVE ( 'NONE', #7354, #15198, #65768, .T. ) ;
#26816 = EDGE_CURVE ( 'NONE', #103269, #27784, #15589, .T. ) ;
#26815 = CARTESIAN_POINT ( 'NONE',  ( 2.949999999999946887, 12.50000000000000000, -6.560283801567339701 ) ) ;
#26817 = ORIENTED_EDGE ( 'NONE', *, *, #117795, .F. ) ;
#26818 = VECTOR ( 'NONE', #9195, 1000.000000000000000 ) ;
#26819 = EDGE_CURVE ( 'NONE', #44204, #80466, #96282, .T. ) ;
#26820 = ORIENTED_EDGE ( 'NONE', *, *, #115442, .F. ) ;
#26821 = ORIENTED_EDGE ( 'NONE', *, *, #67216, .F. ) ;
#26822 = VECTOR ( 'NONE', #74158, 1000.000000000000000 ) ;
#26823 = ORIENTED_EDGE ( 'NONE', *, *, #33540, .F. ) ;
#26824 = ORIENTED_EDGE ( 'NONE', *, *, #67126, .T. ) ;
#26825 = DIRECTION ( 'NONE',  ( 0.000000000000000000, -0.000000000000000000, 1.000000000000000000 ) ) ;
#26826 = DIRECTION ( 'NONE',  ( -0.000000000000000000, 1.000000000000000000, -0.000000000000000000 ) ) ;
#26827 = AXIS2_PLACEMENT_3D ( 'NONE', #28754, #8438, #28102 ) ;
#26828 = EDGE_LOOP ( 'NONE', ( #117604, #6142 ) ) ;
#26829 = DIRECTION ( 'NONE',  ( -4.274815082592931898E-19, -0.9999939076577903929, -0.003490651415223739937 ) ) ;
#26830 = CARTESIAN_POINT ( 'NONE',  ( 17.50000000000000000, 2.750000000000000000, -2.864912725862979848 ) ) ;
#26831 = PRESENTATION_LAYER_ASSIGNMENT (  '', '', ( #28984 ) ) ;
#26832 = CARTESIAN_POINT ( 'NONE',  ( -6.650000000000019007, 12.50000000000000000, -5.867463478539787225 ) ) ;
#26833 = VERTEX_POINT ( 'NONE', #6588 ) ;
#26834 = CARTESIAN_POINT ( 'NONE',  ( -3.150000000000030553, 12.50000000000000000, 6.148780366869520009 ) ) ;
#26835 = CIRCLE ( 'NONE', #45718, 0.06509327318403745899 ) ;
#26836 = CARTESIAN_POINT ( 'NONE',  ( 3.099999999999945466, 2.500000000000000000, 0.4464101615137735513 ) ) ;
#26837 = ORIENTED_EDGE ( 'NONE', *, *, #37139, .F. ) ;
#26838 = CIRCLE ( 'NONE', #51980, 0.09999999999999982514 ) ;
#26839 = ORIENTED_EDGE ( 'NONE', *, *, #48495, .T. ) ;
#26840 = ORIENTED_EDGE ( 'NONE', *, *, #116215, .T. ) ;
#26841 = CARTESIAN_POINT ( 'NONE',  ( 11.64999999999990798, 12.50000000000000000, -1.407149913249512663 ) ) ;
#26842 = AXIS2_PLACEMENT_3D ( 'NONE', #100327, #10621, #50565 ) ;
#26843 = DIRECTION ( 'NONE',  ( 0.000000000000000000, -0.000000000000000000, 1.000000000000000000 ) ) ;
#26844 = ORIENTED_EDGE ( 'NONE', *, *, #51171, .F. ) ;
#26845 = CARTESIAN_POINT ( 'NONE',  ( 4.199999999999939782, 2.500000000000000000, 0.09999999999999772959 ) ) ;
#26847 = AXIS2_PLACEMENT_3D ( 'NONE', #58135, #56176, #18187 ) ;
#26846 = CARTESIAN_POINT ( 'NONE',  ( 11.24999999999994316, 2.500000000000000000, -6.495190528383302464 ) ) ;
#26848 = CARTESIAN_POINT ( 'NONE',  ( -10.65000000000000391, 2.500000000000000000, -6.248780366869523206 ) ) ;
#26849 = CARTESIAN_POINT ( 'NONE',  ( -7.100000000000018296, 2.500000000000000000, -4.330127018922201643 ) ) ;
#26850 = ADVANCED_FACE ( 'NONE', ( #46541 ), #105496, .T. ) ;
#26851 = ADVANCED_FACE ( 'NONE', ( #125118 ), #36753, .T. ) ;
#26852 = VERTEX_POINT ( 'NONE', #15793 ) ;
#26854 = CONICAL_SURFACE ( 'NONE', #108320, 0.1000000000000002554, 0.003490658503988666988 ) ;
#26853 = CONICAL_SURFACE ( 'NONE', #70673, 0.09999999999999999167, 0.003490658503988666988 ) ;
#26855 = CARTESIAN_POINT ( 'NONE',  ( 10.79999999999991012, 2.500000000000000000, -4.330127018922201643 ) ) ;
#26856 = ADVANCED_FACE ( 'NONE', ( #107405 ), #1216, .T. ) ;
#26857 = ORIENTED_EDGE ( 'NONE', *, *, #104116, .T. ) ;
#26858 = EDGE_LOOP ( 'NONE', ( #27315, #79820, #33786, #99002 ) ) ;
#26859 = ORIENTED_EDGE ( 'NONE', *, *, #74417, .T. ) ;
#26860 = CARTESIAN_POINT ( 'NONE',  ( -3.749999999999994671, 2.500000000000000000, -6.495190528383302464 ) ) ;
#26861 = FACE_BOUND ( 'NONE', #9223, .T. ) ;
#26862 = CARTESIAN_POINT ( 'NONE',  ( 2.099999999999950351, 12.50000000000000000, -5.022947341949754119 ) ) ;
#26863 = DIRECTION ( 'NONE',  ( 0.000000000000000000, 1.000000000000000000, 0.000000000000000000 ) ) ;
#26864 = EDGE_CURVE ( 'NONE', #23494, #100363, #26916, .T. ) ;
#26865 = DIRECTION ( 'NONE',  ( 0.000000000000000000, 1.000000000000000000, 0.000000000000000000 ) ) ;
#26866 = AXIS2_PLACEMENT_3D ( 'NONE', #796, #91759, #120579 ) ;
#26867 = ORIENTED_EDGE ( 'NONE', *, *, #108103, .F. ) ;
#26868 = LINE ( 'NONE', #9162, #56787 ) ;
#26869 = DIRECTION ( 'NONE',  ( 1.000000000000000000, 0.000000000000000000, 0.000000000000000000 ) ) ;
#26870 = DIRECTION ( 'NONE',  ( 0.000000000000000000, 0.000000000000000000, 1.000000000000000000 ) ) ;
#26871 = CARTESIAN_POINT ( 'NONE',  ( 6.249999999999932498, 2.500000000000000000, -2.757883832488654097 ) ) ;
#26872 = ORIENTED_EDGE ( 'NONE', *, *, #9854, .T. ) ;
#26873 = DIRECTION ( 'NONE',  ( 0.000000000000000000, 1.000000000000000000, 0.000000000000000000 ) ) ;
#26874 = CONICAL_SURFACE ( 'NONE', #22960, 0.1000000000000002554, 0.003490658503988666988 ) ;
#26875 = AXIS2_PLACEMENT_3D ( 'NONE', #125963, #35665, #16001 ) ;
#26876 = PLANE ( 'NONE',  #62057 ) ;
#26877 = CIRCLE ( 'NONE', #43617, 0.1000000000000002554 ) ;
#26878 = ORIENTED_EDGE ( 'NONE', *, *, #62134, .F. ) ;
#26879 = CARTESIAN_POINT ( 'NONE',  ( -6.650000000000014566, 2.500000000000000000, 5.802370205355744659 ) ) ;
#26880 = CARTESIAN_POINT ( 'NONE',  ( 195.0000000000000000, 4.286263797015736595E-16, 3.500000000000000000 ) ) ;
#26881 = ADVANCED_FACE ( 'NONE', ( #57002 ), #114092, .T. ) ;
#26882 = FACE_BOUND ( 'NONE', #41541, .T. ) ;
#26883 = CARTESIAN_POINT ( 'NONE',  ( 3.677964504776915167, -2.500000000000000444, -9.000000000000001776 ) ) ;
#26884 = CIRCLE ( 'NONE', #83333, 0.1000000000000002554 ) ;
#26885 = AXIS2_PLACEMENT_3D ( 'NONE', #79286, #119195, #69438 ) ;
#26886 = VECTOR ( 'NONE', #4591, 1000.000000000000000 ) ;
#26887 = ORIENTED_EDGE ( 'NONE', *, *, #68618, .T. ) ;
#26888 = DIRECTION ( 'NONE',  ( 0.000000000000000000, 0.000000000000000000, 1.000000000000000000 ) ) ;
#26889 = AXIS2_PLACEMENT_3D ( 'NONE', #116730, #27080, #69569 ) ;
#26890 = ORIENTED_EDGE ( 'NONE', *, *, #127897, .F. ) ;
#26891 = VERTEX_POINT ( 'NONE', #5331 ) ;
#26892 = PLANE ( 'NONE',  #25695 ) ;
#26893 = CARTESIAN_POINT ( 'NONE',  ( 187.0833333333333144, -6.668395609140180369, 3.849999999999994760 ) ) ;
#26894 = VECTOR ( 'NONE', #76944, 1000.000000000000000 ) ;
#26895 = ORIENTED_EDGE ( 'NONE', *, *, #121367, .T. ) ;
#26896 = CARTESIAN_POINT ( 'NONE',  ( 7.499999999999925393, 2.500000000000000000, -3.637306695894650055 ) ) ;
#26897 = LINE ( 'NONE', #36730, #103598 ) ;
#26898 = CONICAL_SURFACE ( 'NONE', #43640, 0.09999999999999982514, 0.003490658503988666988 ) ;
#26899 = ADVANCED_FACE ( 'NONE', ( #35459 ), #47207, .T. ) ;
#26900 = FACE_OUTER_BOUND ( 'NONE', #96403, .T. ) ;
#26901 = DIRECTION ( 'NONE',  ( 0.000000000000000000, 0.000000000000000000, 1.000000000000000000 ) ) ;
#26902 = CIRCLE ( 'NONE', #95864, 0.06509327318403745899 ) ;
#26903 = VERTEX_POINT ( 'NONE', #25610 ) ;
#26904 = DIRECTION ( 'NONE',  ( 0.000000000000000000, 0.000000000000000000, 1.000000000000000000 ) ) ;
#26905 = DIRECTION ( 'NONE',  ( 0.000000000000000000, -0.9999939076577903929, 0.003490651415223739937 ) ) ;
#26906 = LINE ( 'NONE', #17711, #86818 ) ;
#26907 = CIRCLE ( 'NONE', #89606, 0.06509327318403745899 ) ;
#26908 = DIRECTION ( 'NONE',  ( -0.000000000000000000, 1.000000000000000000, -0.000000000000000000 ) ) ;
#26909 = ORIENTED_EDGE ( 'NONE', *, *, #61117, .T. ) ;
#26910 = CARTESIAN_POINT ( 'NONE',  ( -5.850000000000018296, 12.50000000000000000, 5.802370205355744659 ) ) ;
#26911 = ORIENTED_EDGE ( 'NONE', *, *, #122127, .F. ) ;
#26912 = EDGE_CURVE ( 'NONE', #72066, #28200, #119156, .T. ) ;
#26913 = CARTESIAN_POINT ( 'NONE',  ( 16.32360670575071993, 2.500000000000000000, 4.874197301689103590 ) ) ;
#26914 = LINE ( 'NONE', #25607, #24789 ) ;
#26915 = EDGE_LOOP ( 'NONE', ( #87120, #18272 ) ) ;
#26916 = LINE ( 'NONE', #74728, #61876 ) ;
#26917 = CARTESIAN_POINT ( 'NONE',  ( 6.699999999999930012, 2.500000000000000000, -4.330127018922201643 ) ) ;
#26918 = CARTESIAN_POINT ( 'NONE',  ( 10.59999999999990905, 12.50000000000000000, 4.676537180435972552 ) ) ;
#26919 = DIRECTION ( 'NONE',  ( 0.000000000000000000, 0.000000000000000000, 1.000000000000000000 ) ) ;
#26920 = ORIENTED_EDGE ( 'NONE', *, *, #77354, .F. ) ;
#26921 = DIRECTION ( 'NONE',  ( -0.000000000000000000, -1.000000000000000000, -0.000000000000000000 ) ) ;
#26922 = LINE ( 'NONE', #106756, #2471 ) ;
#26923 = EDGE_CURVE ( 'NONE', #113934, #74025, #57657, .T. ) ;
#26924 = CARTESIAN_POINT ( 'NONE',  ( 185.3593750003413732, 0.000000000000000000, 7.564683531250000925 ) ) ;
#26925 = CARTESIAN_POINT ( 'NONE',  ( 1.049999999999954525, 2.500000000000000000, -2.611473670974877592 ) ) ;
#26927 = CONICAL_SURFACE ( 'NONE', #99801, 0.1000000000000000472, 0.003490658503988666988 ) ;
#26926 = AXIS2_PLACEMENT_3D ( 'NONE', #100371, #61087, #120011 ) ;
#26928 = FACE_OUTER_BOUND ( 'NONE', #9734, .T. ) ;
#26930 = ORIENTED_EDGE ( 'NONE', *, *, #113745, .T. ) ;
#26929 = CIRCLE ( 'NONE', #58338, 0.06509327318403745899 ) ;
#26931 = EDGE_LOOP ( 'NONE', ( #82854, #12856, #25505, #94019 ) ) ;
#26932 = DIRECTION ( 'NONE',  ( -0.000000000000000000, 1.000000000000000000, -0.000000000000000000 ) ) ;
#26933 = ORIENTED_EDGE ( 'NONE', *, *, #107201, .F. ) ;
#26934 = FACE_OUTER_BOUND ( 'NONE', #51590, .T. ) ;
#26936 = ORIENTED_EDGE ( 'NONE', *, *, #13933, .T. ) ;
#26935 = VERTEX_POINT ( 'NONE', #80535 ) ;
#26937 = ORIENTED_EDGE ( 'NONE', *, *, #29397, .F. ) ;
#26938 = CIRCLE ( 'NONE', #18613, 0.09999999999999982514 ) ;
#26939 = CARTESIAN_POINT ( 'NONE',  ( -3.350000000000028955, 12.50000000000000000, 7.188010851410848723 ) ) ;
#26940 = CARTESIAN_POINT ( 'NONE',  ( 5.399999999999934630, 12.50000000000000000, 0.6928203230275494784 ) ) ;
#26941 = CARTESIAN_POINT ( 'NONE',  ( -15.39999999999997904, 12.50000000000000000, 0.06509327318403743123 ) ) ;
#26942 = ADVANCED_FACE ( 'NONE', ( #9852 ), #38694, .T. ) ;
#26943 =( NAMED_UNIT ( * ) SI_UNIT ( $, .STERADIAN. ) SOLID_ANGLE_UNIT ( ) );
#26945 = AXIS2_PLACEMENT_3D ( 'NONE', #95457, #15587, #78411 ) ;
#26944 = AXIS2_PLACEMENT_3D ( 'NONE', #1379, #49868, #118575 ) ;
#26946 = DIRECTION ( 'NONE',  ( 0.000000000000000000, 0.000000000000000000, -1.000000000000000000 ) ) ;
#26947 = DIRECTION ( 'NONE',  ( -0.000000000000000000, -1.000000000000000000, -0.000000000000000000 ) ) ;
#26948 = DIRECTION ( 'NONE',  ( -1.000000000000000000, 0.000000000000000000, -0.000000000000000000 ) ) ;
#26949 = ORIENTED_EDGE ( 'NONE', *, *, #77663, .T. ) ;
#26950 = PLANE ( 'NONE',  #31028 ) ;
#26951 = VERTEX_POINT ( 'NONE', #29497 ) ;
#26952 = EDGE_CURVE ( 'NONE', #115797, #60131, #78613, .T. ) ;
#26953 = VECTOR ( 'NONE', #11669, 1000.000000000000000 ) ;
#26954 = ORIENTED_EDGE ( 'NONE', *, *, #108410, .F. ) ;
#26955 = EDGE_LOOP ( 'NONE', ( #43415, #36488 ) ) ;
#26956 = EDGE_LOOP ( 'NONE', ( #8190, #17373, #76492, #37350 ) ) ;
#26957 = DIRECTION ( 'NONE',  ( 0.000000000000000000, 1.000000000000000000, 0.000000000000000000 ) ) ;
#26958 = ADVANCED_FACE ( 'NONE', ( #57672 ), #74375, .T. ) ;
#26959 = EDGE_LOOP ( 'NONE', ( #89965, #33716 ) ) ;
#26960 = ADVANCED_FACE ( 'NONE', ( #109337 ), #61594, .T. ) ;
#26961 = ORIENTED_EDGE ( 'NONE', *, *, #116023, .F. ) ;
#26962 = EDGE_CURVE ( 'NONE', #74901, #43052, #49074, .T. ) ;
#26963 = EDGE_CURVE ( 'NONE', #56285, #39602, #99535, .T. ) ;
#26964 = DIRECTION ( 'NONE',  ( 0.000000000000000000, 0.000000000000000000, -1.000000000000000000 ) ) ;
#26965 = DIRECTION ( 'NONE',  ( 0.000000000000000000, -0.9999939076577903929, 0.003490651415223739937 ) ) ;
#26966 = CARTESIAN_POINT ( 'NONE',  ( 5.449999999999934452, 2.500000000000000000, 2.265063509461097357 ) ) ;
#26967 = CARTESIAN_POINT ( 'NONE',  ( -2.500000000000032863, 2.500000000000000000, 5.022947341949748790 ) ) ;
#26968 = EDGE_CURVE ( 'NONE', #39915, #80214, #7905, .T. ) ;
#26970 = CONICAL_SURFACE ( 'NONE', #10242, 0.1000000000000002554, 0.003490658503988666988 ) ;
#26969 = DIRECTION ( 'NONE',  ( 0.000000000000000000, -0.9999939076577903929, 0.003490651415223739937 ) ) ;
#26971 = ORIENTED_EDGE ( 'NONE', *, *, #13553, .F. ) ;
#26972 = EDGE_CURVE ( 'NONE', #104158, #85752, #124564, .T. ) ;
#26973 = PLANE ( 'NONE',  #93072 ) ;
#26974 = ADVANCED_FACE ( 'NONE', ( #39964 ), #129011, .T. ) ;
#26975 = ORIENTED_EDGE ( 'NONE', *, *, #90892, .F. ) ;
#26977 = CARTESIAN_POINT ( 'NONE',  ( 7.099999999999926814, 12.50000000000000000, -2.276824562219559311E-15 ) ) ;
#26976 = CIRCLE ( 'NONE', #110586, 0.06509327318403745899 ) ;
#26978 = EDGE_CURVE ( 'NONE', #12736, #122222, #55324, .T. ) ;
#26980 = ORIENTED_EDGE ( 'NONE', *, *, #118862, .T. ) ;
#26979 = CONICAL_SURFACE ( 'NONE', #100135, 0.1000000000000000056, 0.003490658503988666988 ) ;
#26981 = FACE_BOUND ( 'NONE', #98836, .T. ) ;
#26982 = ORIENTED_EDGE ( 'NONE', *, *, #10836, .F. ) ;
#26983 = ORIENTED_EDGE ( 'NONE', *, *, #61075, .T. ) ;
#26984 = EDGE_CURVE ( 'NONE', #82307, #127462, #9340, .T. ) ;
#26986 = AXIS2_PLACEMENT_3D ( 'NONE', #1539, #59199, #108905 ) ;
#26985 = FACE_OUTER_BOUND ( 'NONE', #49810, .T. ) ;
#26987 = FACE_OUTER_BOUND ( 'NONE', #45738, .T. ) ;
#26988 = VECTOR ( 'NONE', #20198, 1000.000000000000000 ) ;
#26989 = VECTOR ( 'NONE', #118877, 1000.000000000000000 ) ;
#26990 = DIRECTION ( 'NONE',  ( 0.000000000000000000, 1.000000000000000000, 0.000000000000000000 ) ) ;
#26991 = DIRECTION ( 'NONE',  ( 0.000000000000000000, 0.000000000000000000, 1.000000000000000000 ) ) ;
#26992 = FACE_OUTER_BOUND ( 'NONE', #120973, .T. ) ;
#26993 = ORIENTED_EDGE ( 'NONE', *, *, #3459, .T. ) ;
#26994 = LINE ( 'NONE', #57746, #129253 ) ;
#26995 = DIRECTION ( 'NONE',  ( -0.000000000000000000, -1.000000000000000000, -0.000000000000000000 ) ) ;
#26996 = DIRECTION ( 'NONE',  ( -0.000000000000000000, 1.000000000000000000, -0.000000000000000000 ) ) ;
#26997 = CARTESIAN_POINT ( 'NONE',  ( 13.34999999999990017, 2.500000000000000000, 2.757883832488649656 ) ) ;
#26998 = AXIS2_PLACEMENT_3D ( 'NONE', #10136, #50082, #288 ) ;
#26999 = DIRECTION ( 'NONE',  ( 0.000000000000000000, 0.000000000000000000, -1.000000000000000000 ) ) ;
#27000 = ORIENTED_EDGE ( 'NONE', *, *, #21140, .T. ) ;
#27001 = ORIENTED_EDGE ( 'NONE', *, *, #18056, .F. ) ;
#27002 = DIRECTION ( 'NONE',  ( 0.000000000000000000, 0.000000000000000000, -1.000000000000000000 ) ) ;
#27003 = ORIENTED_EDGE ( 'NONE', *, *, #80200, .T. ) ;
#27004 = DIRECTION ( 'NONE',  ( 0.000000000000000000, 0.000000000000000000, 1.000000000000000000 ) ) ;
#27006 = CONICAL_SURFACE ( 'NONE', #62235, 0.1000000000000000472, 0.003490658503988666988 ) ;
#27005 = DIRECTION ( 'NONE',  ( 0.000000000000000000, 0.000000000000000000, -1.000000000000000000 ) ) ;
#27007 = AXIS2_PLACEMENT_3D ( 'NONE', #26455, #35631, #76843 ) ;
#27008 = ORIENTED_EDGE ( 'NONE', *, *, #34812, .T. ) ;
#27009 = CARTESIAN_POINT ( 'NONE',  ( 184.4583333333333428, 4.445597072760117285, 7.699999999999999289 ) ) ;
#27010 = CARTESIAN_POINT ( 'NONE',  ( -8.550000000000013145, 12.50000000000000000, -6.841600689897073373 ) ) ;
#27011 = CARTESIAN_POINT ( 'NONE',  ( 6.449999999999933564, 2.500000000000000000, -6.741600689897078169 ) ) ;
#27012 = SURFACE_SIDE_STYLE ('',( #58415 ) ) ;
#27013 = FACE_OUTER_BOUND ( 'NONE', #47181, .T. ) ;
#27014 = ORIENTED_EDGE ( 'NONE', *, *, #57837, .F. ) ;
#27015 = ADVANCED_FACE ( 'NONE', ( #108044 ), #68102, .T. ) ;
#27016 = DIRECTION ( 'NONE',  ( 0.000000000000000000, 0.000000000000000000, 1.000000000000000000 ) ) ;
#27017 = CARTESIAN_POINT ( 'NONE',  ( -11.24999999999996447, 2.500000000000000000, -2.165063509461097713 ) ) ;
#27018 = ADVANCED_FACE ( 'NONE', ( #117853 ), #28205, .T. ) ;
#27019 = ORIENTED_EDGE ( 'NONE', *, *, #122862, .T. ) ;
#27020 = DIRECTION ( 'NONE',  ( 0.000000000000000000, 1.000000000000000000, 0.000000000000000000 ) ) ;
#27021 = CIRCLE ( 'NONE', #56254, 0.06509327318403745899 ) ;
#27022 = LINE ( 'NONE', #28307, #110295 ) ;
#27023 = DIRECTION ( 'NONE',  ( -0.000000000000000000, 1.000000000000000000, -0.000000000000000000 ) ) ;
#27024 = VERTEX_POINT ( 'NONE', #17718 ) ;
#27025 = DIRECTION ( 'NONE',  ( 0.000000000000000000, -0.000000000000000000, 1.000000000000000000 ) ) ;
#27026 = ORIENTED_EDGE ( 'NONE', *, *, #46038, .T. ) ;
#27028 = CIRCLE ( 'NONE', #33398, 0.09999999999999982514 ) ;
#27027 = CARTESIAN_POINT ( 'NONE',  ( -11.24999999999996447, 2.500000000000000000, -2.165063509461097713 ) ) ;
#27029 = CARTESIAN_POINT ( 'NONE',  ( -11.84999999999999609, 12.50000000000000000, 6.083687093685483660 ) ) ;
#27030 = DIRECTION ( 'NONE',  ( 0.000000000000000000, -0.000000000000000000, 1.000000000000000000 ) ) ;
#27031 = ORIENTED_EDGE ( 'NONE', *, *, #94496, .T. ) ;
#27032 = CARTESIAN_POINT ( 'NONE',  ( -4.076600168545496672E-14, 12.50000000000000000, -4.957854068765716882 ) ) ;
#27033 = AXIS2_PLACEMENT_3D ( 'NONE', #22022, #61290, #62584 ) ;
#27034 = CARTESIAN_POINT ( 'NONE',  ( 4.149999999999939959, 2.500000000000000000, 1.372243186433545370 ) ) ;
#27035 = AXIS2_PLACEMENT_3D ( 'NONE', #120758, #120119, #91296 ) ;
#27036 = ORIENTED_EDGE ( 'NONE', *, *, #64476, .T. ) ;
#27037 = FACE_OUTER_BOUND ( 'NONE', #126088, .T. ) ;
#27038 = ORIENTED_EDGE ( 'NONE', *, *, #30386, .F. ) ;
#27039 = CARTESIAN_POINT ( 'NONE',  ( -6.650000000000014566, 12.50000000000000000, 5.802370205355744659 ) ) ;
#27041 = CIRCLE ( 'NONE', #41647, 0.06509327318403741736 ) ;
#27040 = CIRCLE ( 'NONE', #102357, 0.1000000000000002554 ) ;
#27042 = ORIENTED_EDGE ( 'NONE', *, *, #24356, .T. ) ;
#27043 = DIRECTION ( 'NONE',  ( 0.000000000000000000, 1.000000000000000000, 0.000000000000000000 ) ) ;
#27044 = DIRECTION ( 'NONE',  ( 0.000000000000000000, 0.000000000000000000, 1.000000000000000000 ) ) ;
#27045 = ORIENTED_EDGE ( 'NONE', *, *, #95567, .T. ) ;
#27046 = ORIENTED_EDGE ( 'NONE', *, *, #90165, .T. ) ;
#27047 = DIRECTION ( 'NONE',  ( 0.000000000000000000, 0.000000000000000000, 1.000000000000000000 ) ) ;
#27048 = CARTESIAN_POINT ( 'NONE',  ( 0.8499999999999545697, 12.50000000000000000, -1.537336459617587581 ) ) ;
#27049 = ORIENTED_EDGE ( 'NONE', *, *, #63430, .T. ) ;
#27051 = EDGE_CURVE ( 'NONE', #106061, #20100, #82522, .T. ) ;
#27050 = CARTESIAN_POINT ( 'NONE',  ( -2.900000000000029221, 2.500000000000000000, -4.330127018922201643 ) ) ;
#27052 = CARTESIAN_POINT ( 'NONE',  ( 5.649999999999934630, 2.500000000000000000, 6.248780366869521430 ) ) ;
#27053 = CARTESIAN_POINT ( 'NONE',  ( 2.299999999999948752, 2.500000000000000000, 0.4464101615137735513 ) ) ;
#27054 = CONICAL_SURFACE ( 'NONE', #81439, 0.1000000000000000472, 0.003490658503988666988 ) ;
#27055 = FACE_OUTER_BOUND ( 'NONE', #93708, .T. ) ;
#27056 = DIRECTION ( 'NONE',  ( 0.000000000000000000, 0.000000000000000000, -1.000000000000000000 ) ) ;
#27057 = DIRECTION ( 'NONE',  ( 0.000000000000000000, 1.000000000000000000, 0.000000000000000000 ) ) ;
#27058 = AXIS2_PLACEMENT_3D ( 'NONE', #85593, #16819, #5727 ) ;
#27059 = AXIS2_PLACEMENT_3D ( 'NONE', #96041, #27290, #117586 ) ;
#27060 = EDGE_LOOP ( 'NONE', ( #41004, #31663 ) ) ;
#27061 = VERTEX_POINT ( 'NONE', #58957 ) ;
#27062 = ORIENTED_EDGE ( 'NONE', *, *, #79299, .T. ) ;
#27063 = ORIENTED_EDGE ( 'NONE', *, *, #74779, .T. ) ;
#27064 = DIRECTION ( 'NONE',  ( 0.000000000000000000, -0.000000000000000000, 1.000000000000000000 ) ) ;
#27065 = DIRECTION ( 'NONE',  ( -0.000000000000000000, 1.000000000000000000, -0.000000000000000000 ) ) ;
#27066 = ADVANCED_FACE ( 'NONE', ( #98868 ), #9203, .T. ) ;
#27067 = CARTESIAN_POINT ( 'NONE',  ( -5.000000000000023093, 2.500000000000000000, 0.6928203230275494784 ) ) ;
#27068 = EDGE_LOOP ( 'NONE', ( #102907, #120811, #63877, #109014 ) ) ;
#27069 = FACE_BOUND ( 'NONE', #109814, .T. ) ;
#27070 = EDGE_CURVE ( 'NONE', #74183, #48277, #20958, .T. ) ;
#27071 = CARTESIAN_POINT ( 'NONE',  ( 9.399999999999918643, 2.500000000000000000, -0.2464101615137782308 ) ) ;
#27072 = DIRECTION ( 'NONE',  ( -4.274815082592931898E-19, -0.9999939076577903929, -0.003490651415223739937 ) ) ;
#27073 = AXIS2_PLACEMENT_3D ( 'NONE', #55168, #57752, #45356 ) ;
#27074 = CIRCLE ( 'NONE', #1924, 0.09999999999999982514 ) ;
#27075 = DIRECTION ( 'NONE',  ( -0.000000000000000000, 1.000000000000000000, -0.000000000000000000 ) ) ;
#27076 = CONICAL_SURFACE ( 'NONE', #60458, 0.1000000000000002554, 0.003490658503988666988 ) ;
#27077 = CARTESIAN_POINT ( 'NONE',  ( 8.549999999999922551, 2.500000000000000000, 2.511473670974873507 ) ) ;
#27078 = CARTESIAN_POINT ( 'NONE',  ( -1.700000000000035261, 12.50000000000000000, 4.330127018922196314 ) ) ;
#27079 = DIRECTION ( 'NONE',  ( 0.000000000000000000, 0.000000000000000000, 1.000000000000000000 ) ) ;
#27080 = DIRECTION ( 'NONE',  ( -0.000000000000000000, -1.000000000000000000, -0.000000000000000000 ) ) ;
#27081 = CARTESIAN_POINT ( 'NONE',  ( 6.649999999999928413, 12.50000000000000000, 1.472243186433545459 ) ) ;
#27082 = EDGE_CURVE ( 'NONE', #78758, #35838, #101571, .T. ) ;
#27083 = CARTESIAN_POINT ( 'NONE',  ( -1.650000000000034772, 2.500000000000000000, 5.802370205355744659 ) ) ;
#27084 = CONICAL_SURFACE ( 'NONE', #20907, 0.09999999999999982514, 0.003490658503988666988 ) ;
#27085 = CARTESIAN_POINT ( 'NONE',  ( 14.34999999999989306, 12.50000000000000000, -1.818653347947326138 ) ) ;
#27086 = CIRCLE ( 'NONE', #35502, 7.700000000000000178 ) ;
#27087 = EDGE_LOOP ( 'NONE', ( #64865, #113798 ) ) ;
#27088 = ORIENTED_EDGE ( 'NONE', *, *, #92381, .T. ) ;
#27089 = AXIS2_PLACEMENT_3D ( 'NONE', #104296, #74194, #94459 ) ;
#27090 = ORIENTED_EDGE ( 'NONE', *, *, #116959, .T. ) ;
#27091 = VERTEX_POINT ( 'NONE', #81798 ) ;
#27092 = CARTESIAN_POINT ( 'NONE',  ( 17.17276927100552442, -1.352216491744406834, -5.266219974095527334 ) ) ;
#27093 = DIRECTION ( 'NONE',  ( 0.000000000000000000, 0.000000000000000000, 1.000000000000000000 ) ) ;
#27095 = VERTEX_POINT ( 'NONE', #51083 ) ;
#27094 = ORIENTED_EDGE ( 'NONE', *, *, #49852, .T. ) ;
#27096 = ORIENTED_EDGE ( 'NONE', *, *, #73653, .F. ) ;
#27097 = DIRECTION ( 'NONE',  ( -0.000000000000000000, -1.000000000000000000, -0.000000000000000000 ) ) ;
#27098 = CARTESIAN_POINT ( 'NONE',  ( 2.500000000000002220, -2.500000000000000444, 9.000000000000001776 ) ) ;
#27099 = LINE ( 'NONE', #78141, #1971 ) ;
#27100 = CARTESIAN_POINT ( 'NONE',  ( -8.750000000000008882, 2.500000000000000000, 1.372243186433545370 ) ) ;
#27101 = VECTOR ( 'NONE', #99709, 1000.000000000000000 ) ;
#27102 = CARTESIAN_POINT ( 'NONE',  ( 187.0729166673494603, 4.445597072760113733, -7.700000000000009948 ) ) ;
#27103 = ORIENTED_EDGE ( 'NONE', *, *, #37918, .F. ) ;
#27104 = ORIENTED_EDGE ( 'NONE', *, *, #67709, .T. ) ;
#27105 = EDGE_CURVE ( 'NONE', #42322, #38829, #45149, .T. ) ;
#27106 = VERTEX_POINT ( 'NONE', #100788 ) ;
#27107 = EDGE_LOOP ( 'NONE', ( #20685, #93283 ) ) ;
#27108 = FACE_OUTER_BOUND ( 'NONE', #63317, .T. ) ;
#27109 = ORIENTED_EDGE ( 'NONE', *, *, #3610, .F. ) ;
#27110 = EDGE_CURVE ( 'NONE', #16232, #47037, #53005, .T. ) ;
#27111 = EDGE_LOOP ( 'NONE', ( #26887, #29128 ) ) ;
#27112 = EDGE_CURVE ( 'NONE', #34236, #12327, #32089, .T. ) ;
#27113 = CARTESIAN_POINT ( 'NONE',  ( 1.649999999999949729, 12.50000000000000000, 5.867463478539781896 ) ) ;
#27114 = LINE ( 'NONE', #85387, #14038 ) ;
#27115 = DIRECTION ( 'NONE',  ( 0.000000000000000000, 0.000000000000000000, 1.000000000000000000 ) ) ;
#27116 = DIRECTION ( 'NONE',  ( -0.000000000000000000, -1.000000000000000000, -0.000000000000000000 ) ) ;
#27117 = EDGE_CURVE ( 'NONE', #26581, #125089, #51216, .T. ) ;
#27118 = ADVANCED_FACE ( 'NONE', ( #72005 ), #40762, .T. ) ;
#27119 = CARTESIAN_POINT ( 'NONE',  ( 176.5000000000000000, 4.898587196589412829E-16, 4.000000000000000000 ) ) ;
#27120 = AXIS2_PLACEMENT_3D ( 'NONE', #85041, #86325, #36619 ) ;
#27121 = ADVANCED_FACE ( 'NONE', ( #83747 ), #21608, .T. ) ;
#27122 = EDGE_LOOP ( 'NONE', ( #80049, #65049, #77633, #99071 ) ) ;
#27123 = DIRECTION ( 'NONE',  ( 0.000000000000000000, 0.000000000000000000, -1.000000000000000000 ) ) ;
#27124 = EDGE_LOOP ( 'NONE', ( #66394, #100874 ) ) ;
#27125 = DIRECTION ( 'NONE',  ( -0.000000000000000000, -1.000000000000000000, -0.000000000000000000 ) ) ;
#27127 = EDGE_CURVE ( 'NONE', #29239, #55712, #99329, .T. ) ;
#27126 = AXIS2_PLACEMENT_3D ( 'NONE', #73664, #44881, #113604 ) ;
#27128 = ORIENTED_EDGE ( 'NONE', *, *, #117518, .T. ) ;
#27129 = CARTESIAN_POINT ( 'NONE',  ( 14.39999999999989555, 12.50000000000000000, -0.4115034346978156399 ) ) ;
#27130 = CARTESIAN_POINT ( 'NONE',  ( 7.299999999999927880, 2.500000000000000000, 3.983716857408420964 ) ) ;
#27131 = EDGE_LOOP ( 'NONE', ( #23207, #86488, #17903, #29356 ) ) ;
#27132 = AXIS2_PLACEMENT_3D ( 'NONE', #40783, #18532, #81332 ) ;
#27133 = CARTESIAN_POINT ( 'NONE',  ( -0.4500000000000402012, 12.50000000000000000, 6.430097255199259010 ) ) ;
#27134 = CARTESIAN_POINT ( 'NONE',  ( -1.700000000000034817, 2.500000000000000000, -2.385244779468109755E-15 ) ) ;
#27135 = ORIENTED_EDGE ( 'NONE', *, *, #15225, .F. ) ;
#27136 = ADVANCED_FACE ( 'NONE', ( #121727 ), #61679, .T. ) ;
#27138 = AXIS2_PLACEMENT_3D ( 'NONE', #25553, #93032, #85129 ) ;
#27137 = AXIS2_PLACEMENT_3D ( 'NONE', #71084, #110986, #111661 ) ;
#27139 = DIRECTION ( 'NONE',  ( 0.000000000000000000, 1.000000000000000000, 0.000000000000000000 ) ) ;
#27140 = ORIENTED_EDGE ( 'NONE', *, *, #303, .T. ) ;
#27141 = ORIENTED_EDGE ( 'NONE', *, *, #108780, .T. ) ;
#27142 = DIRECTION ( 'NONE',  ( 0.000000000000000000, 0.000000000000000000, -1.000000000000000000 ) ) ;
#27143 = CARTESIAN_POINT ( 'NONE',  ( -4.119968255444916849E-14, 2.500000000000000000, 3.637306695894644726 ) ) ;
#27144 = CARTESIAN_POINT ( 'NONE',  ( 183.9427083336747160, -6.551208109652278289, 3.782341765624995134 ) ) ;
#27145 = CARTESIAN_POINT ( 'NONE',  ( -10.40000000000000391, 2.500000000000000000, -3.637306695894645614 ) ) ;
#27146 = PLANE ( 'NONE',  #62502 ) ;
#27147 = DIRECTION ( 'NONE',  ( -0.000000000000000000, 1.000000000000000000, -0.000000000000000000 ) ) ;
#27148 = ORIENTED_EDGE ( 'NONE', *, *, #116079, .F. ) ;
#27149 = FACE_OUTER_BOUND ( 'NONE', #82157, .T. ) ;
#27150 = CIRCLE ( 'NONE', #33430, 0.06509327318403745899 ) ;
#27151 = ORIENTED_EDGE ( 'NONE', *, *, #21058, .F. ) ;
#27152 = DIRECTION ( 'NONE',  ( 0.000000000000000000, 0.000000000000000000, 1.000000000000000000 ) ) ;
#27153 = DIRECTION ( 'NONE',  ( 0.000000000000000000, 1.000000000000000000, 0.000000000000000000 ) ) ;
#27154 = CARTESIAN_POINT ( 'NONE',  ( 1.899999999999951283, 2.500000000000000000, -3.983716857408426293 ) ) ;
#27155 = FACE_OUTER_BOUND ( 'NONE', #115714, .T. ) ;
#27156 = CARTESIAN_POINT ( 'NONE',  ( 3.949999999999941558, 2.500000000000000000, -6.248780366869526759 ) ) ;
#27157 = EDGE_LOOP ( 'NONE', ( #33847, #119219 ) ) ;
#27158 = AXIS2_PLACEMENT_3D ( 'NONE', #51905, #122574, #64283 ) ;
#27159 = ADVANCED_FACE ( 'NONE', ( #81173 ), #3889, .T. ) ;
#27160 = CARTESIAN_POINT ( 'NONE',  ( 10.84999999999990905, 12.50000000000000000, 2.165063509461097713 ) ) ;
#27161 = FACE_OUTER_BOUND ( 'NONE', #64288, .T. ) ;
#27162 = CIRCLE ( 'NONE', #104528, 0.09999999999999999167 ) ;
#27163 = ORIENTED_EDGE ( 'NONE', *, *, #42509, .F. ) ;
#27164 = CARTESIAN_POINT ( 'NONE',  ( 8.349999999999919709, 2.500000000000000000, 7.188010851410848723 ) ) ;
#27165 = ADVANCED_FACE ( 'NONE', ( #43847 ), #115951, .T. ) ;
#27166 = CIRCLE ( 'NONE', #43911, 0.06509327318403745899 ) ;
#27167 = CIRCLE ( 'NONE', #108733, 0.1000000000000002554 ) ;
#27168 = ORIENTED_EDGE ( 'NONE', *, *, #122381, .F. ) ;
#27169 = ORIENTED_EDGE ( 'NONE', *, *, #78851, .T. ) ;
#27170 = CARTESIAN_POINT ( 'NONE',  ( -4.293440603042597559E-14, 12.50000000000000000, 5.022947341949748790 ) ) ;
#27171 = ORIENTED_EDGE ( 'NONE', *, *, #14565, .T. ) ;
#27172 = DIRECTION ( 'NONE',  ( -0.000000000000000000, -1.000000000000000000, -0.000000000000000000 ) ) ;
#27173 = DIRECTION ( 'NONE',  ( 0.000000000000000000, -0.000000000000000000, 1.000000000000000000 ) ) ;
#27174 = AXIS2_PLACEMENT_3D ( 'NONE', #77066, #84943, #75129 ) ;
#27175 = PLANE ( 'NONE',  #75162 ) ;
#27176 = VERTEX_POINT ( 'NONE', #123648 ) ;
#27177 = FACE_BOUND ( 'NONE', #72497, .T. ) ;
#27179 = EDGE_LOOP ( 'NONE', ( #116456, #119569 ) ) ;
#27178 = CARTESIAN_POINT ( 'NONE',  ( 7.699999999999923794, 2.500000000000000000, -0.2464101615137783419 ) ) ;
#27180 = CARTESIAN_POINT ( 'NONE',  ( -9.550000000000007816, 2.500000000000000000, -6.595190528383296780 ) ) ;
#27181 = CARTESIAN_POINT ( 'NONE',  ( -8.300000000000011369, 12.50000000000000000, -4.265033745738164406 ) ) ;
#27182 = ORIENTED_EDGE ( 'NONE', *, *, #103171, .F. ) ;
#27183 = EDGE_LOOP ( 'NONE', ( #52562, #70624, #101635, #65915 ) ) ;
#27184 = ORIENTED_EDGE ( 'NONE', *, *, #44877, .F. ) ;
#27185 = CARTESIAN_POINT ( 'NONE',  ( -0.2000000000000399791, 12.50000000000000000, -4.741630453620015118 ) ) ;
#27186 = DIRECTION ( 'NONE',  ( -4.274815082592931898E-19, -0.9999939076577903929, -0.003490651415223739937 ) ) ;
#27187 = DIRECTION ( 'NONE',  ( 0.000000000000000000, 1.000000000000000000, 0.000000000000000000 ) ) ;
#27188 = FACE_BOUND ( 'NONE', #64721, .T. ) ;
#27189 = VERTEX_POINT ( 'NONE', #33378 ) ;
#27190 = DIRECTION ( 'NONE',  ( 0.000000000000000000, 1.000000000000000000, 0.000000000000000000 ) ) ;
#27191 = DIRECTION ( 'NONE',  ( 0.000000000000000000, 0.000000000000000000, -1.000000000000000000 ) ) ;
#27192 = VERTEX_POINT ( 'NONE', #103392 ) ;
#27193 = EDGE_CURVE ( 'NONE', #48991, #58714, #67921, .T. ) ;
#27194 = DIRECTION ( 'NONE',  ( 0.000000000000000000, 0.000000000000000000, -1.000000000000000000 ) ) ;
#27195 = CARTESIAN_POINT ( 'NONE',  ( 7.899999999999924860, 2.500000000000000000, -5.122947341949753763 ) ) ;
#27196 = DIRECTION ( 'NONE',  ( 0.000000000000000000, 1.000000000000000000, 0.000000000000000000 ) ) ;
#27197 = AXIS2_PLACEMENT_3D ( 'NONE', #89561, #18880, #524 ) ;
#27198 = CARTESIAN_POINT ( 'NONE',  ( 14.54999999999989235, 12.50000000000000000, -2.165063509461101710 ) ) ;
#27199 = DIRECTION ( 'NONE',  ( 0.000000000000000000, -0.000000000000000000, 1.000000000000000000 ) ) ;
#27200 = EDGE_CURVE ( 'NONE', #93869, #91958, #101384, .T. ) ;
#27202 = AXIS2_PLACEMENT_3D ( 'NONE', #59908, #19962, #293 ) ;
#27201 = AXIS2_PLACEMENT_3D ( 'NONE', #127303, #37637, #77536 ) ;
#27203 = ORIENTED_EDGE ( 'NONE', *, *, #32506, .F. ) ;
#27204 = VERTEX_POINT ( 'NONE', #93570 ) ;
#27205 = ORIENTED_EDGE ( 'NONE', *, *, #44883, .T. ) ;
#27206 = ORIENTED_EDGE ( 'NONE', *, *, #69665, .T. ) ;
#27207 = ORIENTED_EDGE ( 'NONE', *, *, #3242, .T. ) ;
#27208 = DIRECTION ( 'NONE',  ( -4.274815082592931898E-19, -0.9999939076577903929, -0.003490651415223739937 ) ) ;
#27209 = ADVANCED_FACE ( 'NONE', ( #110624 ), #128598, .T. ) ;
#27210 = CARTESIAN_POINT ( 'NONE',  ( -2.500000000000032419, 12.50000000000000000, -3.637306695894650055 ) ) ;
#27211 = ORIENTED_EDGE ( 'NONE', *, *, #101283, .F. ) ;
#27212 = FACE_BOUND ( 'NONE', #95823, .T. ) ;
#27213 = ADVANCED_FACE ( 'NONE', ( #11775 ), #32454, .T. ) ;
#27214 = LINE ( 'NONE', #127366, #35276 ) ;
#27215 = CONICAL_SURFACE ( 'NONE', #87751, 0.1000000000000002554, 0.003490658503988666988 ) ;
#27216 = EDGE_CURVE ( 'NONE', #124539, #104801, #26166, .T. ) ;
#27217 = DIRECTION ( 'NONE',  ( 0.000000000000000000, 1.000000000000000000, 0.000000000000000000 ) ) ;
#27218 = CARTESIAN_POINT ( 'NONE',  ( -3.150000000000029221, 2.500000000000000000, -1.818653347947326138 ) ) ;
#27219 = CARTESIAN_POINT ( 'NONE',  ( -11.64999999999999680, 2.500000000000000000, -2.165063509461097713 ) ) ;
#27220 = EDGE_CURVE ( 'NONE', #100479, #71602, #95499, .T. ) ;
#27221 = DIRECTION ( 'NONE',  ( 0.000000000000000000, -0.9999939076577903929, 0.003490651415223739937 ) ) ;
#27222 = VERTEX_POINT ( 'NONE', #64102 ) ;
#27223 = DIRECTION ( 'NONE',  ( 0.000000000000000000, 0.000000000000000000, 1.000000000000000000 ) ) ;
#27224 = ORIENTED_EDGE ( 'NONE', *, *, #86047, .F. ) ;
#27225 = EDGE_LOOP ( 'NONE', ( #56125, #73003, #40779, #3489 ) ) ;
#27226 = VERTEX_POINT ( 'NONE', #113857 ) ;
#27227 = CARTESIAN_POINT ( 'NONE',  ( -7.499999999999980460, 2.500000000000000000, -2.276824562219559311E-15 ) ) ;
#27228 = CARTESIAN_POINT ( 'NONE',  ( 15.62876697814534133, 2.499999999999999112, 5.624417669420174626 ) ) ;
#27229 = DIRECTION ( 'NONE',  ( 0.000000000000000000, -0.9999939076577903929, 0.003490651415223739937 ) ) ;
#27230 = ORIENTED_EDGE ( 'NONE', *, *, #128621, .T. ) ;
#27231 = CARTESIAN_POINT ( 'NONE',  ( 12.64862127267500114, 2.500000000000000444, -8.430718249866270497 ) ) ;
#27232 = CIRCLE ( 'NONE', #81610, 0.06509327318403745899 ) ;
#27233 = CARTESIAN_POINT ( 'NONE',  ( 105.5000000000000142, 2.449293598294706414E-16, -2.000000000000000000 ) ) ;
#27234 = VECTOR ( 'NONE', #57178, 1000.000000000000000 ) ;
#27235 = FACE_OUTER_BOUND ( 'NONE', #7983, .T. ) ;
#27236 = CARTESIAN_POINT ( 'NONE',  ( 184.9895833340161175, -4.445597072760115509, -7.700000000000001954 ) ) ;
#27237 = FACE_OUTER_BOUND ( 'NONE', #55911, .T. ) ;
#27238 = DIRECTION ( 'NONE',  ( 0.000000000000000000, 0.000000000000000000, 1.000000000000000000 ) ) ;
#27239 = LINE ( 'NONE', #7599, #74622 ) ;
#27240 = VERTEX_POINT ( 'NONE', #64743 ) ;
#27241 = CARTESIAN_POINT ( 'NONE',  ( -0.8000000000000315747, 2.500000000000000000, -0.1000000000000000056 ) ) ;
#27242 = AXIS2_PLACEMENT_3D ( 'NONE', #14901, #43140, #33939 ) ;
#27243 = VERTEX_POINT ( 'NONE', #54918 ) ;
#27244 = ADVANCED_FACE ( 'NONE', ( #35933 ), #78413, .T. ) ;
#27245 = VERTEX_POINT ( 'NONE', #46383 ) ;
#27246 = CARTESIAN_POINT ( 'NONE',  ( -9.200000000000009948, 2.500000000000000000, -4.230127018922197557 ) ) ;
#27247 = DIRECTION ( 'NONE',  ( 0.000000000000000000, 0.000000000000000000, 1.000000000000000000 ) ) ;
#27248 = FACE_OUTER_BOUND ( 'NONE', #8516, .T. ) ;
#27249 = ORIENTED_EDGE ( 'NONE', *, *, #14352, .F. ) ;
#27251 = EDGE_CURVE ( 'NONE', #44951, #14963, #107642, .T. ) ;
#27250 = ORIENTED_EDGE ( 'NONE', *, *, #94826, .F. ) ;
#27252 = DIRECTION ( 'NONE',  ( 0.000000000000000000, 0.000000000000000000, -1.000000000000000000 ) ) ;
#27253 = CARTESIAN_POINT ( 'NONE',  ( -2.050000000000032685, 12.50000000000000000, -6.495190528383302464 ) ) ;
#27254 = LINE ( 'NONE', #10209, #87915 ) ;
#27255 = EDGE_LOOP ( 'NONE', ( #11006, #90893, #115057, #83284 ) ) ;
#27256 = ORIENTED_EDGE ( 'NONE', *, *, #50270, .T. ) ;
#27257 = ADVANCED_FACE ( 'NONE', ( #96769 ), #59555, .T. ) ;
#27258 = DIRECTION ( 'NONE',  ( -0.000000000000000000, -1.000000000000000000, -0.000000000000000000 ) ) ;
#27259 = ADVANCED_FACE ( 'NONE', ( #124962 ), #21977, .T. ) ;
#27261 = EDGE_CURVE ( 'NONE', #1609, #74070, #106600, .T. ) ;
#27260 = CIRCLE ( 'NONE', #12593, 0.06509327318403745899 ) ;
#27262 = VERTEX_POINT ( 'NONE', #35304 ) ;
#27263 = DIRECTION ( 'NONE',  ( -0.000000000000000000, 1.000000000000000000, -0.000000000000000000 ) ) ;
#27264 = CARTESIAN_POINT ( 'NONE',  ( -1.650000000000034772, 12.50000000000000000, 6.430097255199259010 ) ) ;
#27265 = ORIENTED_EDGE ( 'NONE', *, *, #69092, .T. ) ;
#27266 = LINE ( 'NONE', #18093, #73296 ) ;
#27267 = ADVANCED_FACE ( 'NONE', ( #75213 ), #3093, .T. ) ;
#27268 = DIRECTION ( 'NONE',  ( 0.000000000000000000, -0.000000000000000000, 1.000000000000000000 ) ) ;
#27269 = AXIS2_PLACEMENT_3D ( 'NONE', #32057, #72613, #100753 ) ;
#27270 = DIRECTION ( 'NONE',  ( 0.000000000000000000, 0.000000000000000000, 1.000000000000000000 ) ) ;
#27271 = DIRECTION ( 'NONE',  ( -4.274815082592931898E-19, -0.9999939076577903929, -0.003490651415223739937 ) ) ;
#27272 = VERTEX_POINT ( 'NONE', #26761 ) ;
#27273 = EDGE_CURVE ( 'NONE', #120531, #2500, #118094, .T. ) ;
#27274 = CARTESIAN_POINT ( 'NONE',  ( 10.84999999999990905, 2.500000000000000000, -7.188010851410854052 ) ) ;
#27275 = EDGE_CURVE ( 'NONE', #115252, #112245, #28222, .T. ) ;
#27276 = CARTESIAN_POINT ( 'NONE',  ( 8.349999999999919709, 12.50000000000000000, 6.495190528383297135 ) ) ;
#27277 = VERTEX_POINT ( 'NONE', #5169 ) ;
#27278 = ORIENTED_EDGE ( 'NONE', *, *, #42244, .T. ) ;
#27279 = CARTESIAN_POINT ( 'NONE',  ( 185.9218750003414016, 0.000000000000000000, 7.564683531250000925 ) ) ;
#27280 = DIRECTION ( 'NONE',  ( -0.000000000000000000, -1.000000000000000000, -0.000000000000000000 ) ) ;
#27281 = DIRECTION ( 'NONE',  ( 0.000000000000000000, 1.000000000000000000, 0.000000000000000000 ) ) ;
#27282 = DIRECTION ( 'NONE',  ( -4.274815082592931898E-19, -0.9999939076577903929, -0.003490651415223739937 ) ) ;
#27283 = CARTESIAN_POINT ( 'NONE',  ( 149.5981739382431783, 0.5000000000000000000, 1.703575533167231537 ) ) ;
#27284 = DIRECTION ( 'NONE',  ( -0.000000000000000000, -1.000000000000000000, -0.000000000000000000 ) ) ;
#27285 = CARTESIAN_POINT ( 'NONE',  ( -5.450000000000023270, 12.50000000000000000, -6.495190528383302464 ) ) ;
#27286 = DIRECTION ( 'NONE',  ( 0.000000000000000000, 0.000000000000000000, 1.000000000000000000 ) ) ;
#27287 = DIRECTION ( 'NONE',  ( 0.000000000000000000, 0.000000000000000000, -1.000000000000000000 ) ) ;
#27288 = CIRCLE ( 'NONE', #8409, 0.06509327318403745899 ) ;
#27289 = AXIS2_PLACEMENT_3D ( 'NONE', #34531, #35799, #73780 ) ;
#27290 = DIRECTION ( 'NONE',  ( -0.000000000000000000, 1.000000000000000000, -0.000000000000000000 ) ) ;
#27291 = CIRCLE ( 'NONE', #23180, 0.06509327318403745899 ) ;
#27292 = ORIENTED_EDGE ( 'NONE', *, *, #53560, .T. ) ;
#27293 = CARTESIAN_POINT ( 'NONE',  ( 7.099999999999928590, 2.500000000000000000, -5.022947341949754119 ) ) ;
#27294 = DIRECTION ( 'NONE',  ( -0.000000000000000000, -1.000000000000000000, -0.000000000000000000 ) ) ;
#27295 = CARTESIAN_POINT ( 'NONE',  ( 9.349999999999919709, 12.50000000000000000, 2.511473670974873507 ) ) ;
#27296 = DIRECTION ( 'NONE',  ( 0.000000000000000000, 1.000000000000000000, 0.000000000000000000 ) ) ;
#27297 = VERTEX_POINT ( 'NONE', #115110 ) ;
#27298 = DIRECTION ( 'NONE',  ( 0.000000000000000000, 1.000000000000000000, 0.000000000000000000 ) ) ;
#27299 = CARTESIAN_POINT ( 'NONE',  ( 8.549999999999918998, 2.500000000000000000, -1.718653347947326049 ) ) ;
#27301 = EDGE_LOOP ( 'NONE', ( #65119, #27505 ) ) ;
#27300 = DIRECTION ( 'NONE',  ( 0.000000000000000000, 1.000000000000000000, 0.000000000000000000 ) ) ;
#27302 = EDGE_LOOP ( 'NONE', ( #110395, #49845 ) ) ;
#27303 = EDGE_CURVE ( 'NONE', #120069, #53996, #125587, .T. ) ;
#27304 = ORIENTED_EDGE ( 'NONE', *, *, #6011, .F. ) ;
#27305 = ORIENTED_EDGE ( 'NONE', *, *, #88739, .T. ) ;
#27306 = ORIENTED_EDGE ( 'NONE', *, *, #93980, .F. ) ;
#27307 = FACE_OUTER_BOUND ( 'NONE', #69277, .T. ) ;
#27308 = DIRECTION ( 'NONE',  ( -0.000000000000000000, -1.000000000000000000, -0.000000000000000000 ) ) ;
#27309 = DIRECTION ( 'NONE',  ( 0.000000000000000000, 0.000000000000000000, 1.000000000000000000 ) ) ;
#27310 = DIRECTION ( 'NONE',  ( -0.000000000000000000, 1.000000000000000000, -0.000000000000000000 ) ) ;
#27311 = AXIS2_PLACEMENT_3D ( 'NONE', #20382, #102162, #51143 ) ;
#27312 = ORIENTED_EDGE ( 'NONE', *, *, #9051, .T. ) ;
#27313 = AXIS2_PLACEMENT_3D ( 'NONE', #119669, #534, #52236 ) ;
#27314 = DIRECTION ( 'NONE',  ( 0.000000000000000000, 0.000000000000000000, 1.000000000000000000 ) ) ;
#27315 = ORIENTED_EDGE ( 'NONE', *, *, #113985, .F. ) ;
#27316 = CARTESIAN_POINT ( 'NONE',  ( 48.83465639049822471, -3.619824997336297034, -4.313881469032290639 ) ) ;
#27317 = CARTESIAN_POINT ( 'NONE',  ( 7.899999999999923084, 12.50000000000000000, 0.6928203230275494784 ) ) ;
#27318 = CYLINDRICAL_SURFACE ( 'NONE', #12884, 1.000000000000000888 ) ;
#27319 = DIRECTION ( 'NONE',  ( -0.000000000000000000, -1.000000000000000000, -0.000000000000000000 ) ) ;
#27320 = FACE_OUTER_BOUND ( 'NONE', #103058, .T. ) ;
#27321 = AXIS2_PLACEMENT_3D ( 'NONE', #41689, #81586, #41048 ) ;
#27322 = ORIENTED_EDGE ( 'NONE', *, *, #121067, .F. ) ;
#27323 = ORIENTED_EDGE ( 'NONE', *, *, #69970, .F. ) ;
#27324 = ORIENTED_EDGE ( 'NONE', *, *, #34857, .F. ) ;
#27325 = ORIENTED_EDGE ( 'NONE', *, *, #13362, .T. ) ;
#27326 = PLANE ( 'NONE',  #39807 ) ;
#27327 = CARTESIAN_POINT ( 'NONE',  ( 8.149999999999920419, 2.500000000000000000, 6.148780366869520897 ) ) ;
#27328 = CARTESIAN_POINT ( 'NONE',  ( 11.44999999999990692, 12.50000000000000000, 1.818653347947321475 ) ) ;
#27329 = FACE_BOUND ( 'NONE', #8427, .T. ) ;
#27330 = DIRECTION ( 'NONE',  ( 0.000000000000000000, 1.000000000000000000, 0.000000000000000000 ) ) ;
#27331 = DIRECTION ( 'NONE',  ( 0.000000000000000000, 0.000000000000000000, 1.000000000000000000 ) ) ;
#27332 = DIRECTION ( 'NONE',  ( -0.000000000000000000, -1.000000000000000000, -0.000000000000000000 ) ) ;
#27333 = FACE_OUTER_BOUND ( 'NONE', #46042, .T. ) ;
#27334 = AXIS2_PLACEMENT_3D ( 'NONE', #48413, #18302, #88987 ) ;
#27335 = CIRCLE ( 'NONE', #4338, 0.06509327318403745899 ) ;
#27336 = CARTESIAN_POINT ( 'NONE',  ( 186.0885416670080872, -6.551208109652273848, -3.782341765625003571 ) ) ;
#27337 = DIRECTION ( 'NONE',  ( 0.000000000000000000, 0.000000000000000000, 1.000000000000000000 ) ) ;
#27338 = PLANE ( 'NONE',  #76200 ) ;
#27339 = VECTOR ( 'NONE', #64693, 1000.000000000000000 ) ;
#27340 = EDGE_CURVE ( 'NONE', #94406, #55939, #4503, .T. ) ;
#27341 = DIRECTION ( 'NONE',  ( -0.000000000000000000, -1.000000000000000000, -0.000000000000000000 ) ) ;
#27342 = EDGE_LOOP ( 'NONE', ( #109241, #57851, #47838, #41683 ) ) ;
#27343 = CIRCLE ( 'NONE', #108914, 0.1000000000000002554 ) ;
#27344 = VERTEX_POINT ( 'NONE', #84389 ) ;
#27345 = EDGE_LOOP ( 'NONE', ( #71703, #113714 ) ) ;
#27346 = ORIENTED_EDGE ( 'NONE', *, *, #114143, .T. ) ;
#27347 = EDGE_CURVE ( 'NONE', #59613, #42850, #122320, .T. ) ;
#27348 = CARTESIAN_POINT ( 'NONE',  ( -10.00000000000000533, 12.50000000000000000, 5.022947341949748790 ) ) ;
#27349 = FACE_BOUND ( 'NONE', #41552, .T. ) ;
#27350 = EDGE_CURVE ( 'NONE', #58766, #33854, #65862, .T. ) ;
#27351 = DIRECTION ( 'NONE',  ( 0.000000000000000000, -0.000000000000000000, 1.000000000000000000 ) ) ;
#27352 = DIRECTION ( 'NONE',  ( -0.000000000000000000, 1.000000000000000000, -0.000000000000000000 ) ) ;
#27353 = EDGE_CURVE ( 'NONE', #10496, #94042, #109702, .T. ) ;
#27354 = ADVANCED_FACE ( 'NONE', ( #104657 ), #14968, .T. ) ;
#27355 = EDGE_LOOP ( 'NONE', ( #109821, #10068, #67069, #25256 ) ) ;
#27356 = CARTESIAN_POINT ( 'NONE',  ( -3.550000000000027356, 2.500000000000000000, 1.918653347947321564 ) ) ;
#27357 = ADVANCED_FACE ( 'NONE', ( #10339 ), #47012, .T. ) ;
#27358 = DIRECTION ( 'NONE',  ( -0.000000000000000000, -1.000000000000000000, -0.000000000000000000 ) ) ;
#27359 = ADVANCED_FACE ( 'NONE', ( #18861 ), #80463, .T. ) ;
#27360 = CARTESIAN_POINT ( 'NONE',  ( 0.6499999999999566125, 12.50000000000000000, -6.148780366869526226 ) ) ;
#27361 = VERTEX_POINT ( 'NONE', #109834 ) ;
#27362 = CARTESIAN_POINT ( 'NONE',  ( 13.34999999999989662, 12.50000000000000000, -2.857883832488653741 ) ) ;
#27363 = DIRECTION ( 'NONE',  ( -4.274815082592931898E-19, -0.9999939076577903929, -0.003490651415223739937 ) ) ;
#27364 = AXIS2_PLACEMENT_3D ( 'NONE', #74292, #114210, #4876 ) ;
#27365 = ORIENTED_EDGE ( 'NONE', *, *, #23355, .T. ) ;
#27366 = VECTOR ( 'NONE', #31642, 1000.000000000000000 ) ;
#27367 = DIRECTION ( 'NONE',  ( 0.000000000000000000, 0.000000000000000000, 1.000000000000000000 ) ) ;
#27368 = CARTESIAN_POINT ( 'NONE',  ( -7.100000000000013856, 12.50000000000000000, 3.702399969078682407 ) ) ;
#27369 = ORIENTED_EDGE ( 'NONE', *, *, #128795, .T. ) ;
#27370 = DIRECTION ( 'NONE',  ( -4.274815082592931898E-19, -0.9999939076577903929, -0.003490651415223739937 ) ) ;
#27371 = CIRCLE ( 'NONE', #79717, 0.06509327318403745899 ) ;
#27372 = DIRECTION ( 'NONE',  ( 0.000000000000000000, -0.000000000000000000, 1.000000000000000000 ) ) ;
#27373 = VERTEX_POINT ( 'NONE', #88904 ) ;
#27374 = DIRECTION ( 'NONE',  ( -0.000000000000000000, -1.000000000000000000, -0.000000000000000000 ) ) ;
#27375 = VERTEX_POINT ( 'NONE', #37239 ) ;
#27376 = AXIS2_PLACEMENT_3D ( 'NONE', #20027, #38391, #355 ) ;
#27377 = ORIENTED_EDGE ( 'NONE', *, *, #109507, .T. ) ;
#27378 = FACE_OUTER_BOUND ( 'NONE', #78331, .T. ) ;
#27379 = ORIENTED_EDGE ( 'NONE', *, *, #83031, .F. ) ;
#27380 = CARTESIAN_POINT ( 'NONE',  ( 14.99999999999992895, 2.500000000000000000, -2.276824562219559311E-15 ) ) ;
#27381 = FACE_BOUND ( 'NONE', #70810, .T. ) ;
#27382 = ORIENTED_EDGE ( 'NONE', *, *, #94549, .F. ) ;
#27383 = DIRECTION ( 'NONE',  ( 0.000000000000000000, 0.000000000000000000, -1.000000000000000000 ) ) ;
#27384 = ORIENTED_EDGE ( 'NONE', *, *, #47813, .T. ) ;
#27385 = FACE_OUTER_BOUND ( 'NONE', #40599, .T. ) ;
#27386 = LINE ( 'NONE', #56212, #23641 ) ;
#27387 = DIRECTION ( 'NONE',  ( 0.000000000000000000, 0.000000000000000000, 1.000000000000000000 ) ) ;
#27388 = ADVANCED_FACE ( 'NONE', ( #8393 ), #74286, .T. ) ;
#27389 = CARTESIAN_POINT ( 'NONE',  ( -7.900000000000014566, 2.500000000000000000, -2.276824562219559311E-15 ) ) ;
#27390 = LINE ( 'NONE', #16908, #51667 ) ;
#27391 = ORIENTED_EDGE ( 'NONE', *, *, #91843, .T. ) ;
#27392 = ORIENTED_EDGE ( 'NONE', *, *, #85889, .F. ) ;
#27393 = AXIS2_PLACEMENT_3D ( 'NONE', #509, #80389, #119644 ) ;
#27394 = FACE_OUTER_BOUND ( 'NONE', #72156, .T. ) ;
#27395 = DIRECTION ( 'NONE',  ( 0.000000000000000000, 0.000000000000000000, 1.000000000000000000 ) ) ;
#27397 = EDGE_CURVE ( 'NONE', #122201, #12963, #34592, .T. ) ;
#27396 = CARTESIAN_POINT ( 'NONE',  ( 4.349999999999941025, 2.500000000000000000, -6.148780366869526226 ) ) ;
#27399 = VERTEX_POINT ( 'NONE', #98701 ) ;
#27398 = ORIENTED_EDGE ( 'NONE', *, *, #122605, .T. ) ;
#27400 = ORIENTED_EDGE ( 'NONE', *, *, #31111, .T. ) ;
#27401 = ADVANCED_FACE ( 'NONE', ( #57516 ), #126512, .T. ) ;
#27402 = DIRECTION ( 'NONE',  ( 0.000000000000000000, 0.000000000000000000, -1.000000000000000000 ) ) ;
#27403 = EDGE_CURVE ( 'NONE', #3522, #110270, #59641, .T. ) ;
#27404 = VECTOR ( 'NONE', #53700, 1000.000000000000000 ) ;
#27405 = DIRECTION ( 'NONE',  ( 0.000000000000000000, 0.000000000000000000, -1.000000000000000000 ) ) ;
#27406 = AXIS2_PLACEMENT_3D ( 'NONE', #16782, #15509, #76386 ) ;
#27407 = CARTESIAN_POINT ( 'NONE',  ( 3.149999999999944400, 12.50000000000000000, 2.511473670974873507 ) ) ;
#27408 = ADVANCED_FACE ( 'NONE', ( #9039 ), #48997, .T. ) ;
#27409 = APPLICATION_PROTOCOL_DEFINITION ( 'draft international standard', 'automotive_design', 1998, #58082 ) ;
#27410 = CARTESIAN_POINT ( 'NONE',  ( -3.350000000000029399, 12.50000000000000000, 6.495190528383297135 ) ) ;
#27411 = LINE ( 'NONE', #35966, #91994 ) ;
#27412 = CARTESIAN_POINT ( 'NONE',  ( 11.64999999999990621, 2.500000000000000000, -2.165063509461101710 ) ) ;
#27413 = DIRECTION ( 'NONE',  ( 0.000000000000000000, 0.000000000000000000, -1.000000000000000000 ) ) ;
#27414 = DIRECTION ( 'NONE',  ( 0.000000000000000000, 0.000000000000000000, 1.000000000000000000 ) ) ;
#27415 = EDGE_CURVE ( 'NONE', #3309, #35519, #100267, .T. ) ;
#27416 = EDGE_CURVE ( 'NONE', #104801, #33641, #47698, .T. ) ;
#27417 = CARTESIAN_POINT ( 'NONE',  ( 184.5000000000000000, 0.000000000000000000, 0.000000000000000000 ) ) ;
#27418 = EDGE_CURVE ( 'NONE', #16543, #80247, #91003, .T. ) ;
#27419 = EDGE_LOOP ( 'NONE', ( #52545, #104144 ) ) ;
#27420 = AXIS2_PLACEMENT_3D ( 'NONE', #56410, #115303, #6013 ) ;
#27422 = ORIENTED_EDGE ( 'NONE', *, *, #13004, .F. ) ;
#27421 = EDGE_CURVE ( 'NONE', #75945, #17249, #107727, .T. ) ;
#27423 = EDGE_CURVE ( 'NONE', #99834, #70878, #57564, .T. ) ;
#27424 = DIRECTION ( 'NONE',  ( 0.000000000000000000, 1.000000000000000000, 0.000000000000000000 ) ) ;
#27425 = ORIENTED_EDGE ( 'NONE', *, *, #42959, .F. ) ;
#27426 = ORIENTED_EDGE ( 'NONE', *, *, #37422, .T. ) ;
#27427 = CARTESIAN_POINT ( 'NONE',  ( 9.999999999999914735, 2.500000000000000000, 0.6928203230275494784 ) ) ;
#27428 = CARTESIAN_POINT ( 'NONE',  ( 8.749999999999923617, 12.50000000000000000, 1.472243186433545459 ) ) ;
#27429 = CARTESIAN_POINT ( 'NONE',  ( -6.900000000000019007, 2.500000000000000000, 0.2464101615137735679 ) ) ;
#27430 = ADVANCED_FACE ( 'NONE', ( #18214 ), #61779, .T. ) ;
#27431 = AXIS2_PLACEMENT_3D ( 'NONE', #48919, #38458, #88823 ) ;
#27432 = DIRECTION ( 'NONE',  ( -0.000000000000000000, -1.000000000000000000, -0.000000000000000000 ) ) ;
#27433 = CARTESIAN_POINT ( 'NONE',  ( 185.0833333333333144, -6.668395609140180369, 3.849999999999994760 ) ) ;
#27434 = DIRECTION ( 'NONE',  ( -4.274815082592931898E-19, -0.9999939076577903929, -0.003490651415223739937 ) ) ;
#27435 = CARTESIAN_POINT ( 'NONE',  ( 10.84999999999991260, 2.500000000000000000, -2.165063509461101710 ) ) ;
#27436 = EDGE_LOOP ( 'NONE', ( #36660, #54335 ) ) ;
#27437 = DIRECTION ( 'NONE',  ( -0.000000000000000000, 1.000000000000000000, -0.000000000000000000 ) ) ;
#27438 = VECTOR ( 'NONE', #92718, 1000.000000000000000 ) ;
#27439 = CARTESIAN_POINT ( 'NONE',  ( -14.54999999999998472, 2.500000000000000000, -2.265063509461099578 ) ) ;
#27440 = ORIENTED_EDGE ( 'NONE', *, *, #77326, .T. ) ;
#27441 = CONICAL_SURFACE ( 'NONE', #98538, 0.09999999999999982514, 0.003490658503988666988 ) ;
#27442 = AXIS2_PLACEMENT_3D ( 'NONE', #5046, #92814, #54790 ) ;
#27443 = ORIENTED_EDGE ( 'NONE', *, *, #104376, .F. ) ;
#27444 = VERTEX_POINT ( 'NONE', #60108 ) ;
#27445 = VERTEX_POINT ( 'NONE', #100016 ) ;
#27446 = CARTESIAN_POINT ( 'NONE',  ( -8.550000000000011369, 2.500000000000000000, -2.411473670974877859 ) ) ;
#27447 = PLANE ( 'NONE',  #47841 ) ;
#27448 = EDGE_LOOP ( 'NONE', ( #90648, #79390 ) ) ;
#27449 = FACE_OUTER_BOUND ( 'NONE', #14203, .T. ) ;
#27450 = DIRECTION ( 'NONE',  ( -0.000000000000000000, -1.000000000000000000, -0.000000000000000000 ) ) ;
#27451 = FACE_OUTER_BOUND ( 'NONE', #94560, .T. ) ;
#27452 = ORIENTED_EDGE ( 'NONE', *, *, #101717, .F. ) ;
#27453 = DIRECTION ( 'NONE',  ( 0.000000000000000000, 0.000000000000000000, 1.000000000000000000 ) ) ;
#27454 = CARTESIAN_POINT ( 'NONE',  ( 7.299999999999926104, 2.500000000000000000, 4.776537180435972196 ) ) ;
#27455 = ORIENTED_EDGE ( 'NONE', *, *, #125149, .T. ) ;
#27456 = EDGE_CURVE ( 'NONE', #44454, #6764, #118190, .T. ) ;
#27457 = VERTEX_POINT ( 'NONE', #98069 ) ;
#27458 = VERTEX_POINT ( 'NONE', #48333 ) ;
#27459 = AXIS2_PLACEMENT_3D ( 'NONE', #65263, #105199, #120190 ) ;
#27460 = DIRECTION ( 'NONE',  ( 0.000000000000000000, 0.000000000000000000, 1.000000000000000000 ) ) ;
#27461 = AXIS2_PLACEMENT_3D ( 'NONE', #115463, #46110, #125942 ) ;
#27462 = FACE_OUTER_BOUND ( 'NONE', #106268, .T. ) ;
#27463 = AXIS2_PLACEMENT_3D ( 'NONE', #76446, #125533, #14906 ) ;
#27464 = VECTOR ( 'NONE', #117535, 1000.000000000000000 ) ;
#27466 = ORIENTED_EDGE ( 'NONE', *, *, #16617, .T. ) ;
#27465 = CIRCLE ( 'NONE', #71304, 0.06509327318403745899 ) ;
#27467 = CARTESIAN_POINT ( 'NONE',  ( 1.849999999999950129, 2.500000000000000000, -6.941600689897078347 ) ) ;
#27468 = DIRECTION ( 'NONE',  ( 0.000000000000000000, 0.000000000000000000, 1.000000000000000000 ) ) ;
#27469 = ADVANCED_FACE ( 'NONE', ( #503 ), #19913, .T. ) ;
#27470 = CARTESIAN_POINT ( 'NONE',  ( -1.650000000000034328, 2.500000000000000000, -6.495190528383302464 ) ) ;
#27471 = CARTESIAN_POINT ( 'NONE',  ( 187.5000000000000000, 0.000000000000000000, 0.000000000000000000 ) ) ;
#27472 = EDGE_LOOP ( 'NONE', ( #9671, #79832 ) ) ;
#27473 = DIRECTION ( 'NONE',  ( 0.000000000000000000, 1.000000000000000000, 0.000000000000000000 ) ) ;
#27474 = EDGE_LOOP ( 'NONE', ( #73415, #69415, #94859, #107857 ) ) ;
#27475 = ORIENTED_EDGE ( 'NONE', *, *, #5844, .F. ) ;
#27476 = DIRECTION ( 'NONE',  ( 0.000000000000000000, 1.000000000000000000, 0.000000000000000000 ) ) ;
#27477 = ORIENTED_EDGE ( 'NONE', *, *, #24033, .F. ) ;
#27478 = DIRECTION ( 'NONE',  ( 0.000000000000000000, 0.000000000000000000, 1.000000000000000000 ) ) ;
#27479 = FACE_BOUND ( 'NONE', #63238, .T. ) ;
#27480 = CARTESIAN_POINT ( 'NONE',  ( 17.49862860983209956, 2.500000000000000000, 4.081131818001135336 ) ) ;
#27481 = FACE_OUTER_BOUND ( 'NONE', #121551, .T. ) ;
#27482 = FACE_OUTER_BOUND ( 'NONE', #7828, .T. ) ;
#27483 = ORIENTED_EDGE ( 'NONE', *, *, #53407, .T. ) ;
#27484 = DIRECTION ( 'NONE',  ( 0.000000000000000000, -0.9999939076577903929, 0.003490651415223739937 ) ) ;
#27485 = CARTESIAN_POINT ( 'NONE',  ( -6.900000000000019007, 2.500000000000000000, -4.776537180435978414 ) ) ;
#27486 = FACE_OUTER_BOUND ( 'NONE', #47532, .T. ) ;
#27487 = DIRECTION ( 'NONE',  ( -0.000000000000000000, 1.000000000000000000, -0.000000000000000000 ) ) ;
#27488 = ORIENTED_EDGE ( 'NONE', *, *, #118546, .T. ) ;
#27489 = CIRCLE ( 'NONE', #48443, 0.09999999999999999167 ) ;
#27490 = DIRECTION ( 'NONE',  ( 0.000000000000000000, 0.000000000000000000, -1.000000000000000000 ) ) ;
#27491 = CONICAL_SURFACE ( 'NONE', #65144, 0.1000000000000002554, 0.003490658503988666988 ) ;
#27492 = ADVANCED_FACE ( 'NONE', ( #101311 ), #92779, .T. ) ;
#27493 = DIRECTION ( 'NONE',  ( 0.000000000000000000, -0.000000000000000000, 1.000000000000000000 ) ) ;
#27494 = ORIENTED_EDGE ( 'NONE', *, *, #17297, .F. ) ;
#27495 = DIRECTION ( 'NONE',  ( -0.000000000000000000, -1.000000000000000000, -0.000000000000000000 ) ) ;
#27496 = LINE ( 'NONE', #67413, #86103 ) ;
#27497 = FACE_BOUND ( 'NONE', #124312, .T. ) ;
#27498 = AXIS2_PLACEMENT_3D ( 'NONE', #7840, #98155, #119099 ) ;
#27499 = ADVANCED_FACE ( 'NONE', ( #52845 ), #68013, .T. ) ;
#27500 = DIRECTION ( 'NONE',  ( -0.000000000000000000, -1.000000000000000000, -0.000000000000000000 ) ) ;
#27501 = AXIS2_PLACEMENT_3D ( 'NONE', #46432, #26165, #114524 ) ;
#27502 = ORIENTED_EDGE ( 'NONE', *, *, #19719, .F. ) ;
#27503 = FACE_OUTER_BOUND ( 'NONE', #35120, .T. ) ;
#27504 = EDGE_CURVE ( 'NONE', #72741, #19960, #11577, .T. ) ;
#27505 = ORIENTED_EDGE ( 'NONE', *, *, #107523, .F. ) ;
#27506 = EDGE_CURVE ( 'NONE', #63975, #95323, #52203, .T. ) ;
#27507 = EDGE_LOOP ( 'NONE', ( #126625, #120140 ) ) ;
#27508 = CARTESIAN_POINT ( 'NONE',  ( 18.29531403502779696, 0.5011766475904850804, -4.780851392375763176 ) ) ;
#27509 = ADVANCED_FACE ( 'NONE', ( #103238 ), #38803, .T. ) ;
#27510 = EDGE_CURVE ( 'NONE', #23306, #50259, #76339, .T. ) ;
#27511 = CARTESIAN_POINT ( 'NONE',  ( 186.0833333333333144, -6.668395609140180369, 3.849999999999994760 ) ) ;
#27512 = ADVANCED_FACE ( 'NONE', ( #1794 ), #23368, .T. ) ;
#27513 = EDGE_LOOP ( 'NONE', ( #351, #67100 ) ) ;
#27515 = DIRECTION ( 'NONE',  ( 0.000000000000000000, 0.000000000000000000, 1.000000000000000000 ) ) ;
#27514 = AXIS2_PLACEMENT_3D ( 'NONE', #67739, #88002, #97840 ) ;
#27516 = DIRECTION ( 'NONE',  ( -0.000000000000000000, -1.000000000000000000, -0.000000000000000000 ) ) ;
#27517 = AXIS2_PLACEMENT_3D ( 'NONE', #84013, #104932, #55218 ) ;
#27518 = VECTOR ( 'NONE', #69158, 1000.000000000000000 ) ;
#27519 = FACE_OUTER_BOUND ( 'NONE', #111862, .T. ) ;
#27520 = EDGE_CURVE ( 'NONE', #115678, #126433, #116038, .T. ) ;
#27521 = VECTOR ( 'NONE', #21233, 1000.000000000000000 ) ;
#27522 = EDGE_CURVE ( 'NONE', #114128, #102404, #84740, .T. ) ;
#27523 = ADVANCED_FACE ( 'NONE', ( #51569 ), #13626, .T. ) ;
#27524 = VERTEX_POINT ( 'NONE', #91475 ) ;
#27525 = DIRECTION ( 'NONE',  ( -0.000000000000000000, -1.000000000000000000, -0.000000000000000000 ) ) ;
#27526 = AXIS2_PLACEMENT_3D ( 'NONE', #107388, #79233, #9188 ) ;
#27527 = CIRCLE ( 'NONE', #123674, 0.1000000000000002554 ) ;
#27528 = CARTESIAN_POINT ( 'NONE',  ( 12.09999999999990195, 12.50000000000000000, -0.6928203230275541413 ) ) ;
#27529 = DIRECTION ( 'NONE',  ( 0.000000000000000000, 0.000000000000000000, -1.000000000000000000 ) ) ;
#27530 = DIRECTION ( 'NONE',  ( 0.000000000000000000, 1.000000000000000000, 0.000000000000000000 ) ) ;
#27531 = EDGE_LOOP ( 'NONE', ( #62266, #43177, #118415, #85294 ) ) ;
#27532 = DIRECTION ( 'NONE',  ( 0.000000000000000000, 0.000000000000000000, -1.000000000000000000 ) ) ;
#27533 = VERTEX_POINT ( 'NONE', #112418 ) ;
#27534 = DIRECTION ( 'NONE',  ( 0.000000000000000000, 0.000000000000000000, 1.000000000000000000 ) ) ;
#27535 = ORIENTED_EDGE ( 'NONE', *, *, #80141, .F. ) ;
#27536 = CARTESIAN_POINT ( 'NONE',  ( 8.099999999999921485, 2.500000000000000000, -0.3464101615137783474 ) ) ;
#27537 = DIRECTION ( 'NONE',  ( 0.000000000000000000, 0.000000000000000000, 1.000000000000000000 ) ) ;
#27538 = FACE_OUTER_BOUND ( 'NONE', #98138, .T. ) ;
#27539 = DIRECTION ( 'NONE',  ( -0.000000000000000000, 1.000000000000000000, -0.000000000000000000 ) ) ;
#27540 = ORIENTED_EDGE ( 'NONE', *, *, #9967, .F. ) ;
#27541 = DIRECTION ( 'NONE',  ( 0.000000000000000000, 0.000000000000000000, 1.000000000000000000 ) ) ;
#27542 = CARTESIAN_POINT ( 'NONE',  ( 5.849999999999933031, 2.500000000000000000, -1.472243186433550122 ) ) ;
#27543 = DIRECTION ( 'NONE',  ( -0.000000000000000000, 1.000000000000000000, -0.000000000000000000 ) ) ;
#27544 = CARTESIAN_POINT ( 'NONE',  ( -13.29999999999998828, 12.50000000000000000, 4.330127018922196314 ) ) ;
#27545 = LINE ( 'NONE', #46550, #32797 ) ;
#27546 = ORIENTED_EDGE ( 'NONE', *, *, #105170, .T. ) ;
#27547 = ORIENTED_EDGE ( 'NONE', *, *, #70008, .T. ) ;
#27548 = CARTESIAN_POINT ( 'NONE',  ( 2.049999999999950084, 2.500000000000000000, 2.065063509461097624 ) ) ;
#27549 = ORIENTED_EDGE ( 'NONE', *, *, #25569, .T. ) ;
#27550 = VECTOR ( 'NONE', #92218, 1000.000000000000000 ) ;
#27551 = CARTESIAN_POINT ( 'NONE',  ( 8.949999999999917577, 12.50000000000000000, -2.576566944158915184 ) ) ;
#27552 = AXIS2_PLACEMENT_3D ( 'NONE', #31188, #71093, #53393 ) ;
#27553 = AXIS2_PLACEMENT_3D ( 'NONE', #102312, #50613, #70914 ) ;
#27555 = VERTEX_POINT ( 'NONE', #121570 ) ;
#27554 = ORIENTED_EDGE ( 'NONE', *, *, #4010, .F. ) ;
#27556 = ORIENTED_EDGE ( 'NONE', *, *, #26531, .F. ) ;
#27557 = FACE_OUTER_BOUND ( 'NONE', #50721, .T. ) ;
#27558 = DIRECTION ( 'NONE',  ( 0.000000000000000000, 0.000000000000000000, -1.000000000000000000 ) ) ;
#27559 = AXIS2_PLACEMENT_3D ( 'NONE', #62124, #3205, #102042 ) ;
#27560 = CARTESIAN_POINT ( 'NONE',  ( 1.899999999999951283, 2.500000000000000000, -3.983716857408426293 ) ) ;
#27561 = AXIS2_PLACEMENT_3D ( 'NONE', #1011, #122088, #92618 ) ;
#27562 = CARTESIAN_POINT ( 'NONE',  ( 4.149999999999938183, 2.500000000000000000, 7.288010851410849256 ) ) ;
#27563 = CARTESIAN_POINT ( 'NONE',  ( 5.799999999999934985, 12.50000000000000000, -4.330127018922201643 ) ) ;
#27564 = AXIS2_PLACEMENT_3D ( 'NONE', #8865, #127379, #48826 ) ;
#27565 = DIRECTION ( 'NONE',  ( 0.000000000000000000, -0.9999939076577903929, 0.003490651415223739937 ) ) ;
#27566 = CARTESIAN_POINT ( 'NONE',  ( 9.399999999999918643, 2.500000000000000000, 0.2464101615137736789 ) ) ;
#27567 = CIRCLE ( 'NONE', #25511, 0.1000000000000002554 ) ;
#27568 = VERTEX_POINT ( 'NONE', #43057 ) ;
#27569 = EDGE_CURVE ( 'NONE', #69598, #3939, #40860, .T. ) ;
#27570 = DIRECTION ( 'NONE',  ( 0.000000000000000000, 0.000000000000000000, -1.000000000000000000 ) ) ;
#27571 = VERTEX_POINT ( 'NONE', #53499 ) ;
#27572 = ADVANCED_FACE ( 'NONE', ( #102577 ), #82958, .T. ) ;
#27573 = ORIENTED_EDGE ( 'NONE', *, *, #36673, .T. ) ;
#27574 = EDGE_LOOP ( 'NONE', ( #49679, #99683 ) ) ;
#27575 = ORIENTED_EDGE ( 'NONE', *, *, #6966, .F. ) ;
#27576 = EDGE_CURVE ( 'NONE', #86599, #110722, #33227, .T. ) ;
#27577 = CARTESIAN_POINT ( 'NONE',  ( 8.949999999999921130, 2.500000000000000000, 1.818653347947321475 ) ) ;
#27578 = EDGE_LOOP ( 'NONE', ( #96925, #37069, #119605, #49308 ) ) ;
#27579 = ORIENTED_EDGE ( 'NONE', *, *, #62145, .T. ) ;
#27580 = ADVANCED_FACE ( 'NONE', ( #110470 ), #69237, .T. ) ;
#27581 = CARTESIAN_POINT ( 'NONE',  ( 3.099999999999944134, 2.500000000000000000, 4.776537180435972196 ) ) ;
#27582 = DIRECTION ( 'NONE',  ( 0.000000000000000000, 0.000000000000000000, 1.000000000000000000 ) ) ;
#27583 = FACE_OUTER_BOUND ( 'NONE', #111169, .T. ) ;
#27584 = CARTESIAN_POINT ( 'NONE',  ( 3.099999999999943245, 12.50000000000000000, 3.983716857408420076 ) ) ;
#27585 = DIRECTION ( 'NONE',  ( 0.000000000000000000, -0.9999939076577903929, 0.003490651415223739937 ) ) ;
#27586 = EDGE_LOOP ( 'NONE', ( #97878, #43452 ) ) ;
#27587 = CARTESIAN_POINT ( 'NONE',  ( 6.849999999999930367, 2.500000000000000000, -6.841600689897078702 ) ) ;
#27588 = AXIS2_PLACEMENT_3D ( 'NONE', #82214, #24576, #112321 ) ;
#27589 = ORIENTED_EDGE ( 'NONE', *, *, #48211, .F. ) ;
#27590 = CARTESIAN_POINT ( 'NONE',  ( -14.34999999999998543, 2.500000000000000000, 1.718653347947325383 ) ) ;
#27591 = EDGE_LOOP ( 'NONE', ( #73719, #118625 ) ) ;
#27592 = CARTESIAN_POINT ( 'NONE',  ( -3.150000000000029665, 2.500000000000000000, 6.841600689897072485 ) ) ;
#27593 = ORIENTED_EDGE ( 'NONE', *, *, #34794, .F. ) ;
#27594 = EDGE_CURVE ( 'NONE', #3622, #5490, #75498, .T. ) ;
#27595 = ORIENTED_EDGE ( 'NONE', *, *, #101557, .T. ) ;
#27596 = AXIS2_PLACEMENT_3D ( 'NONE', #71782, #30583, #50852 ) ;
#27597 = FACE_OUTER_BOUND ( 'NONE', #117358, .T. ) ;
#27598 = DIRECTION ( 'NONE',  ( 0.000000000000000000, 0.000000000000000000, 1.000000000000000000 ) ) ;
#27599 = CIRCLE ( 'NONE', #98605, 7.700000000000000178 ) ;
#27600 = CARTESIAN_POINT ( 'NONE',  ( 8.949999999999917577, 2.500000000000000000, 6.048780366869520364 ) ) ;
#27601 = CIRCLE ( 'NONE', #75625, 0.09999999999999982514 ) ;
#27602 = CARTESIAN_POINT ( 'NONE',  ( -2.700000000000029932, 12.50000000000000000, -4.611443907251939756 ) ) ;
#27603 = FACE_OUTER_BOUND ( 'NONE', #125930, .T. ) ;
#27604 = ORIENTED_EDGE ( 'NONE', *, *, #80513, .T. ) ;
#27605 = LINE ( 'NONE', #8604, #10092 ) ;
#27606 = DIRECTION ( 'NONE',  ( 0.000000000000000000, 0.000000000000000000, 1.000000000000000000 ) ) ;
#27607 = DIRECTION ( 'NONE',  ( -0.000000000000000000, 1.000000000000000000, -0.000000000000000000 ) ) ;
#27608 = DIRECTION ( 'NONE',  ( -0.000000000000000000, 1.000000000000000000, -0.000000000000000000 ) ) ;
#27609 = FACE_OUTER_BOUND ( 'NONE', #20181, .T. ) ;
#27610 = ORIENTED_EDGE ( 'NONE', *, *, #91523, .F. ) ;
#27611 = EDGE_CURVE ( 'NONE', #36319, #78931, #104837, .T. ) ;
#27612 = AXIS2_PLACEMENT_3D ( 'NONE', #19808, #80007, #119939 ) ;
#27613 = CIRCLE ( 'NONE', #100771, 0.06509327318403743123 ) ;
#27614 = VECTOR ( 'NONE', #77950, 1000.000000000000000 ) ;
#27615 = ORIENTED_EDGE ( 'NONE', *, *, #127563, .F. ) ;
#27616 = DIRECTION ( 'NONE',  ( 0.000000000000000000, 0.000000000000000000, 1.000000000000000000 ) ) ;
#27617 = CIRCLE ( 'NONE', #17133, 0.09999999999999999167 ) ;
#27618 = EDGE_LOOP ( 'NONE', ( #33953, #103627 ) ) ;
#27619 = CARTESIAN_POINT ( 'NONE',  ( -5.850000000000018296, 12.50000000000000000, 5.867463478539781896 ) ) ;
#27620 = PLANE ( 'NONE',  #110787 ) ;
#27621 = CONICAL_SURFACE ( 'NONE', #40265, 0.1000000000000000472, 0.003490658503988666988 ) ;
#27622 = ORIENTED_EDGE ( 'NONE', *, *, #39223, .T. ) ;
#27623 = CARTESIAN_POINT ( 'NONE',  ( 185.8750000000000000, 8.891194145520236347, 5.444286225454521982E-16 ) ) ;
#27624 = CARTESIAN_POINT ( 'NONE',  ( 6.649999999999928413, 12.50000000000000000, 1.407149913249508000 ) ) ;
#27625 = ADVANCED_FACE ( 'NONE', ( #33844 ), #111085, .T. ) ;
#27626 = DIRECTION ( 'NONE',  ( 0.000000000000000000, 1.000000000000000000, 0.000000000000000000 ) ) ;
#27627 = LINE ( 'NONE', #68857, #62311 ) ;
#27628 = EDGE_LOOP ( 'NONE', ( #5244, #92038 ) ) ;
#27629 = CARTESIAN_POINT ( 'NONE',  ( -3.100000000000028511, 12.50000000000000000, -0.3464101615137782364 ) ) ;
#27630 = CARTESIAN_POINT ( 'NONE',  ( 6.649999999999931077, 2.500000000000000000, -6.595190528383302109 ) ) ;
#27631 = ORIENTED_EDGE ( 'NONE', *, *, #87397, .T. ) ;
#27632 = DIRECTION ( 'NONE',  ( -0.000000000000000000, -1.000000000000000000, -0.000000000000000000 ) ) ;
#27633 = DIRECTION ( 'NONE',  ( -1.000000000000000000, -0.000000000000000000, -0.000000000000000000 ) ) ;
#27634 = DIRECTION ( 'NONE',  ( -0.000000000000000000, -1.000000000000000000, -0.000000000000000000 ) ) ;
#27635 = ORIENTED_EDGE ( 'NONE', *, *, #13341, .T. ) ;
#27636 = DIRECTION ( 'NONE',  ( 0.000000000000000000, 0.000000000000000000, -1.000000000000000000 ) ) ;
#27637 = VECTOR ( 'NONE', #118159, 1000.000000000000000 ) ;
#27638 = AXIS2_PLACEMENT_3D ( 'NONE', #19095, #118611, #109440 ) ;
#27639 = AXIS2_PLACEMENT_3D ( 'NONE', #24232, #62868, #14389 ) ;
#27640 = ORIENTED_EDGE ( 'NONE', *, *, #110561, .T. ) ;
#27641 = FACE_OUTER_BOUND ( 'NONE', #14437, .T. ) ;
#27642 = DIRECTION ( 'NONE',  ( 0.000000000000000000, 1.000000000000000000, 0.000000000000000000 ) ) ;
#27643 = DIRECTION ( 'NONE',  ( 0.000000000000000000, 0.000000000000000000, 1.000000000000000000 ) ) ;
#27644 = VERTEX_POINT ( 'NONE', #85525 ) ;
#27646 = CARTESIAN_POINT ( 'NONE',  ( -3.550000000000028244, 2.500000000000000000, -1.718653347947326049 ) ) ;
#27645 = VECTOR ( 'NONE', #114114, 1000.000000000000000 ) ;
#27647 = CONICAL_SURFACE ( 'NONE', #88186, 0.09999999999999982514, 0.003490658503988666988 ) ;
#27649 = EDGE_CURVE ( 'NONE', #7845, #27568, #6515, .T. ) ;
#27648 = AXIS2_PLACEMENT_3D ( 'NONE', #20980, #60902, #12437 ) ;
#27650 = PLANE ( 'NONE',  #1510 ) ;
#27651 = CIRCLE ( 'NONE', #88290, 0.1000000000000000472 ) ;
#27652 = ORIENTED_EDGE ( 'NONE', *, *, #28334, .T. ) ;
#27653 = AXIS2_PLACEMENT_3D ( 'NONE', #50296, #79749, #9724 ) ;
#27654 = CARTESIAN_POINT ( 'NONE',  ( -6.650000000000015454, 2.500000000000000000, 7.088010851410848190 ) ) ;
#27655 = ORIENTED_EDGE ( 'NONE', *, *, #94549, .T. ) ;
#27656 = CIRCLE ( 'NONE', #23475, 0.06509327318403745899 ) ;
#27657 = DIRECTION ( 'NONE',  ( -0.000000000000000000, -1.000000000000000000, -0.000000000000000000 ) ) ;
#27658 = EDGE_CURVE ( 'NONE', #57054, #86890, #54135, .T. ) ;
#27659 = ORIENTED_EDGE ( 'NONE', *, *, #61396, .T. ) ;
#27660 = DIRECTION ( 'NONE',  ( 1.000000000000000000, 0.000000000000000000, 0.000000000000000000 ) ) ;
#27661 = DIRECTION ( 'NONE',  ( -0.000000000000000000, -1.000000000000000000, -0.000000000000000000 ) ) ;
#27662 = EDGE_CURVE ( 'NONE', #64421, #96425, #48415, .T. ) ;
#27663 = VERTEX_POINT ( 'NONE', #84223 ) ;
#27664 = ADVANCED_FACE ( 'NONE', ( #44307 ), #35158, .T. ) ;
#27665 = VERTEX_POINT ( 'NONE', #26608 ) ;
#27666 = EDGE_CURVE ( 'NONE', #108022, #24264, #50472, .T. ) ;
#27667 = ADVANCED_FACE ( 'NONE', ( #95352 ), #106453, .T. ) ;
#27668 = LINE ( 'NONE', #19128, #111540 ) ;
#27669 = CARTESIAN_POINT ( 'NONE',  ( -5.650000000000019895, 2.500000000000000000, 1.718653347947321386 ) ) ;
#27670 = ORIENTED_EDGE ( 'NONE', *, *, #501, .T. ) ;
#27671 = AXIS2_PLACEMENT_3D ( 'NONE', #8804, #88675, #7523 ) ;
#27672 = DIRECTION ( 'NONE',  ( 0.000000000000000000, 0.000000000000000000, -1.000000000000000000 ) ) ;
#27673 = CARTESIAN_POINT ( 'NONE',  ( -8.150000000000014566, 12.50000000000000000, -6.213873640053559022 ) ) ;
#27674 = ADVANCED_FACE ( 'NONE', ( #115616 ), #96422, .T. ) ;
#27675 = CARTESIAN_POINT ( 'NONE',  ( -4.150000000000025224, 2.500000000000000000, 5.802370205355744659 ) ) ;
#27676 = LINE ( 'NONE', #67605, #777 ) ;
#27677 = EDGE_CURVE ( 'NONE', #99122, #99741, #2331, .T. ) ;
#27678 = DIRECTION ( 'NONE',  ( 0.000000000000000000, -0.9999939076577903929, 0.003490651415223739937 ) ) ;
#27679 = DIRECTION ( 'NONE',  ( -0.000000000000000000, -1.000000000000000000, -0.000000000000000000 ) ) ;
#27680 = EDGE_CURVE ( 'NONE', #78540, #114240, #98569, .T. ) ;
#27681 = CIRCLE ( 'NONE', #82075, 0.06509327318403745899 ) ;
#27682 = EDGE_CURVE ( 'NONE', #96759, #62016, #113164, .T. ) ;
#27683 = CIRCLE ( 'NONE', #31913, 0.06509327318403745899 ) ;
#27684 = ADVANCED_FACE ( 'NONE', ( #56051 ), #121563, .T. ) ;
#27685 = ORIENTED_EDGE ( 'NONE', *, *, #14093, .T. ) ;
#27686 = VERTEX_POINT ( 'NONE', #6293 ) ;
#27687 = EDGE_LOOP ( 'NONE', ( #112663, #21964, #18805, #93427 ) ) ;
#27688 = ORIENTED_EDGE ( 'NONE', *, *, #92306, .F. ) ;
#27689 = DIRECTION ( 'NONE',  ( -0.000000000000000000, 1.000000000000000000, -0.000000000000000000 ) ) ;
#27690 = DIRECTION ( 'NONE',  ( -0.000000000000000000, 1.000000000000000000, -0.000000000000000000 ) ) ;
#27691 = CARTESIAN_POINT ( 'NONE',  ( -10.84999999999999964, 2.500000000000000000, 2.857883832488649301 ) ) ;
#27692 = VERTEX_POINT ( 'NONE', #14822 ) ;
#27693 = FACE_BOUND ( 'NONE', #24734, .T. ) ;
#27694 = EDGE_LOOP ( 'NONE', ( #24589, #36246 ) ) ;
#27696 = ADVANCED_FACE ( 'NONE', ( #103881 ), #4474, .T. ) ;
#27695 = AXIS2_PLACEMENT_3D ( 'NONE', #67752, #88685, #9481 ) ;
#27697 = CARTESIAN_POINT ( 'NONE',  ( -11.24999999999996270, 2.500000000000000000, 6.495190528383297135 ) ) ;
#27698 = FACE_OUTER_BOUND ( 'NONE', #68940, .T. ) ;
#27699 = AXIS2_PLACEMENT_3D ( 'NONE', #67013, #107605, #108874 ) ;
#27701 = DIRECTION ( 'NONE',  ( 0.000000000000000000, 0.000000000000000000, 1.000000000000000000 ) ) ;
#27700 = CIRCLE ( 'NONE', #92461, 0.1000000000000002554 ) ;
#27702 = CIRCLE ( 'NONE', #92463, 0.06509327318403745899 ) ;
#27703 = CARTESIAN_POINT ( 'NONE',  ( 0.7999999999999612976, 2.500000000000000000, 0.09999999999999989453 ) ) ;
#27704 = DIRECTION ( 'NONE',  ( 0.000000000000000000, -0.000000000000000000, 1.000000000000000000 ) ) ;
#27705 = DIRECTION ( 'NONE',  ( 0.000000000000000000, 0.000000000000000000, 1.000000000000000000 ) ) ;
#27706 = CARTESIAN_POINT ( 'NONE',  ( -1.250000000000001110, 12.50000000000000000, -2.165063509461101710 ) ) ;
#27707 = CARTESIAN_POINT ( 'NONE',  ( 0.4499999999999552136, 12.50000000000000000, 6.560283801567334372 ) ) ;
#27708 = LINE ( 'NONE', #127225, #108024 ) ;
#27709 = CONICAL_SURFACE ( 'NONE', #13122, 0.09999999999999982514, 0.003490658503988666988 ) ;
#27710 = CARTESIAN_POINT ( 'NONE',  ( -4.350000000000027178, 12.50000000000000000, -6.213873640053564351 ) ) ;
#27711 = CONICAL_SURFACE ( 'NONE', #15176, 0.1000000000000000472, 0.003490658503988666988 ) ;
#27712 = EDGE_LOOP ( 'NONE', ( #4695, #127793 ) ) ;
#27713 = ORIENTED_EDGE ( 'NONE', *, *, #127009, .T. ) ;
#27714 = EDGE_LOOP ( 'NONE', ( #90110, #101518 ) ) ;
#27716 = EDGE_LOOP ( 'NONE', ( #29334, #71069 ) ) ;
#27715 = CIRCLE ( 'NONE', #2564, 0.09999999999999982514 ) ;
#27717 = VECTOR ( 'NONE', #28245, 1000.000000000000000 ) ;
#27718 = AXIS2_PLACEMENT_3D ( 'NONE', #90999, #52359, #81184 ) ;
#27719 = FACE_OUTER_BOUND ( 'NONE', #13151, .T. ) ;
#27720 = DIRECTION ( 'NONE',  ( 0.000000000000000000, 0.000000000000000000, 1.000000000000000000 ) ) ;
#27722 = ORIENTED_EDGE ( 'NONE', *, *, #2526, .F. ) ;
#27721 = EDGE_LOOP ( 'NONE', ( #125055, #8708, #118166, #58505 ) ) ;
#27723 = EDGE_LOOP ( 'NONE', ( #9066, #22023, #50835, #42742 ) ) ;
#27724 = CIRCLE ( 'NONE', #92574, 0.06509327318403745899 ) ;
#27725 = CARTESIAN_POINT ( 'NONE',  ( 0.8499999999999553468, 2.500000000000000000, 2.165063509461097713 ) ) ;
#27726 = AXIS2_PLACEMENT_3D ( 'NONE', #88371, #128342, #38677 ) ;
#27727 = DIRECTION ( 'NONE',  ( 0.000000000000000000, 0.000000000000000000, 1.000000000000000000 ) ) ;
#27728 = CARTESIAN_POINT ( 'NONE',  ( -4.150000000000024336, 2.500000000000000000, 2.265063509461097357 ) ) ;
#27729 = DIRECTION ( 'NONE',  ( 0.000000000000000000, -0.000000000000000000, 1.000000000000000000 ) ) ;
#27730 = DIRECTION ( 'NONE',  ( 0.000000000000000000, 0.000000000000000000, -1.000000000000000000 ) ) ;
#27731 = ORIENTED_EDGE ( 'NONE', *, *, #117671, .F. ) ;
#27732 = PLANE ( 'NONE',  #53794 ) ;
#27733 = ORIENTED_EDGE ( 'NONE', *, *, #418, .T. ) ;
#27734 = ADVANCED_FACE ( 'NONE', ( #64593 ), #73451, .T. ) ;
#27735 = ORIENTED_EDGE ( 'NONE', *, *, #46467, .F. ) ;
#27736 = ORIENTED_EDGE ( 'NONE', *, *, #45844, .F. ) ;
#27737 = ADVANCED_FACE ( 'NONE', ( #94693 ), #46264, .T. ) ;
#27738 = DIRECTION ( 'NONE',  ( 0.000000000000000000, 0.000000000000000000, 1.000000000000000000 ) ) ;
#27739 = CIRCLE ( 'NONE', #117599, 0.1000000000000002554 ) ;
#27740 = ORIENTED_EDGE ( 'NONE', *, *, #33768, .T. ) ;
#27741 = ORIENTED_EDGE ( 'NONE', *, *, #89105, .F. ) ;
#27742 = CARTESIAN_POINT ( 'NONE',  ( 10.84999999999991260, 2.500000000000000000, -2.857883832488653741 ) ) ;
#27743 = EDGE_CURVE ( 'NONE', #50291, #40749, #94380, .T. ) ;
#27744 = DIRECTION ( 'NONE',  ( -0.000000000000000000, 1.000000000000000000, -0.000000000000000000 ) ) ;
#27745 = CARTESIAN_POINT ( 'NONE',  ( -10.45000000000000462, 2.500000000000000000, -2.165063509461097713 ) ) ;
#27747 = DIRECTION ( 'NONE',  ( 0.000000000000000000, 1.000000000000000000, 0.000000000000000000 ) ) ;
#27746 = AXIS2_PLACEMENT_3D ( 'NONE', #121376, #103024, #111563 ) ;
#27748 = CONICAL_SURFACE ( 'NONE', #77919, 0.09999999999999982514, 0.003490658503988666988 ) ;
#27749 = AXIS2_PLACEMENT_3D ( 'NONE', #92981, #113909, #44507 ) ;
#27750 = CARTESIAN_POINT ( 'NONE',  ( -0.6500000000000398792, 2.500000000000000000, -2.611473670974877592 ) ) ;
#27751 = EDGE_LOOP ( 'NONE', ( #75579, #102905, #94369, #56284 ) ) ;
#27752 = LINE ( 'NONE', #57881, #53271 ) ;
#27753 = AXIS2_PLACEMENT_3D ( 'NONE', #5853, #35343, #3933 ) ;
#27754 = VERTEX_POINT ( 'NONE', #38382 ) ;
#27755 = DIRECTION ( 'NONE',  ( 0.000000000000000000, 0.000000000000000000, 1.000000000000000000 ) ) ;
#27756 = CONICAL_SURFACE ( 'NONE', #100907, 0.1000000000000000472, 0.003490658503988666988 ) ;
#27757 = ORIENTED_EDGE ( 'NONE', *, *, #4358, .F. ) ;
#27758 = CARTESIAN_POINT ( 'NONE',  ( 109.6384078294126283, 7.300040591920232913, -4.735138557421405991 ) ) ;
#27759 = CARTESIAN_POINT ( 'NONE',  ( 3.099999999999943245, 12.50000000000000000, 3.983716857408420076 ) ) ;
#27760 = ORIENTED_EDGE ( 'NONE', *, *, #234, .T. ) ;
#27761 = AXIS2_PLACEMENT_3D ( 'NONE', #70999, #110901, #68404 ) ;
#27762 = DIRECTION ( 'NONE',  ( 0.000000000000000000, 1.000000000000000000, 0.000000000000000000 ) ) ;
#27763 = AXIS2_PLACEMENT_3D ( 'NONE', #97771, #8092, #48041 ) ;
#27764 = DIRECTION ( 'NONE',  ( -4.274815082592931898E-19, -0.9999939076577903929, -0.003490651415223739937 ) ) ;
#27765 = ORIENTED_EDGE ( 'NONE', *, *, #71786, .F. ) ;
#27766 = CONICAL_SURFACE ( 'NONE', #29837, 0.1000000000000002554, 0.003490658503988666988 ) ;
#27767 = DIRECTION ( 'NONE',  ( -0.000000000000000000, -1.000000000000000000, -0.000000000000000000 ) ) ;
#27768 = VERTEX_POINT ( 'NONE', #28548 ) ;
#27769 = ORIENTED_EDGE ( 'NONE', *, *, #21176, .F. ) ;
#27770 = FACE_OUTER_BOUND ( 'NONE', #95680, .T. ) ;
#27771 = DIRECTION ( 'NONE',  ( 0.000000000000000000, 0.000000000000000000, 1.000000000000000000 ) ) ;
#27772 = CARTESIAN_POINT ( 'NONE',  ( 185.8385416670080872, 6.551208109652274736, 3.782341765625001351 ) ) ;
#27773 = CARTESIAN_POINT ( 'NONE',  ( -6.650000000000014566, 12.50000000000000000, 2.230156782645134950 ) ) ;
#27774 = CIRCLE ( 'NONE', #123917, 0.06509327318403745899 ) ;
#27775 = EDGE_CURVE ( 'NONE', #19384, #33136, #280, .T. ) ;
#27776 = FACE_OUTER_BOUND ( 'NONE', #44642, .T. ) ;
#27777 = CARTESIAN_POINT ( 'NONE',  ( 184.0729166673494603, 4.445597072760049784, -7.700000000000123634 ) ) ;
#27778 = AXIS2_PLACEMENT_3D ( 'NONE', #70631, #41836, #82409 ) ;
#27779 = VERTEX_POINT ( 'NONE', #86812 ) ;
#27780 = AXIS2_PLACEMENT_3D ( 'NONE', #129302, #119437, #29786 ) ;
#27781 = DIRECTION ( 'NONE',  ( 0.000000000000000000, 0.000000000000000000, -1.000000000000000000 ) ) ;
#27782 = DIRECTION ( 'NONE',  ( -4.274815082592931898E-19, -0.9999939076577903929, -0.003490651415223739937 ) ) ;
#27783 = AXIS2_PLACEMENT_3D ( 'NONE', #15781, #114627, #24966 ) ;
#27784 = VERTEX_POINT ( 'NONE', #69100 ) ;
#27785 = EDGE_CURVE ( 'NONE', #16781, #110736, #37952, .T. ) ;
#27786 = FACE_OUTER_BOUND ( 'NONE', #114348, .T. ) ;
#27787 = DIRECTION ( 'NONE',  ( 0.000000000000000000, -0.9999939076577903929, 0.003490651415223739937 ) ) ;
#27788 = DIRECTION ( 'NONE',  ( 0.000000000000000000, 0.000000000000000000, 1.000000000000000000 ) ) ;
#27789 = ADVANCED_FACE ( 'NONE', ( #67814 ), #71383, .T. ) ;
#27790 = DIRECTION ( 'NONE',  ( 0.000000000000000000, 0.000000000000000000, 1.000000000000000000 ) ) ;
#27791 = AXIS2_PLACEMENT_3D ( 'NONE', #90606, #10736, #24938 ) ;
#27793 = VECTOR ( 'NONE', #80420, 1000.000000000000000 ) ;
#27792 = CARTESIAN_POINT ( 'NONE',  ( 3.349999999999944578, 2.500000000000000000, -1.472243186433550122 ) ) ;
#27794 = ORIENTED_EDGE ( 'NONE', *, *, #121081, .F. ) ;
#27795 = VECTOR ( 'NONE', #8541, 1000.000000000000000 ) ;
#27796 = VECTOR ( 'NONE', #116658, 1000.000000000000000 ) ;
#27797 = DIRECTION ( 'NONE',  ( 0.000000000000000000, 0.000000000000000000, 1.000000000000000000 ) ) ;
#27798 = CARTESIAN_POINT ( 'NONE',  ( -1.250000000000037970, 2.500000000000000000, 7.288010851410849256 ) ) ;
#27799 = EDGE_CURVE ( 'NONE', #59725, #122166, #10733, .T. ) ;
#27800 = CIRCLE ( 'NONE', #9019, 0.06509327318403745899 ) ;
#27801 = ORIENTED_EDGE ( 'NONE', *, *, #91850, .F. ) ;
#27803 = AXIS2_PLACEMENT_3D ( 'NONE', #18768, #47602, #96669 ) ;
#27802 = DIRECTION ( 'NONE',  ( 0.000000000000000000, 0.000000000000000000, 1.000000000000000000 ) ) ;
#27804 = VERTEX_POINT ( 'NONE', #56685 ) ;
#27805 = CIRCLE ( 'NONE', #65362, 0.09999999999999982514 ) ;
#27807 = EDGE_LOOP ( 'NONE', ( #13982, #108014, #16873, #95720 ) ) ;
#27806 = AXIS2_PLACEMENT_3D ( 'NONE', #24222, #34710, #64138 ) ;
#27808 = CONICAL_SURFACE ( 'NONE', #100977, 0.1000000000000002554, 0.003490658503988666988 ) ;
#27809 = LINE ( 'NONE', #48761, #21586 ) ;
#27811 = ORIENTED_EDGE ( 'NONE', *, *, #82925, .F. ) ;
#27810 = VECTOR ( 'NONE', #52809, 1000.000000000000000 ) ;
#27812 = DIRECTION ( 'NONE',  ( 0.000000000000000000, 1.000000000000000000, 0.000000000000000000 ) ) ;
#27813 = CARTESIAN_POINT ( 'NONE',  ( 5.799999999999931433, 2.500000000000000000, 4.330127018922196314 ) ) ;
#27814 = CARTESIAN_POINT ( 'NONE',  ( -7.900000000000011013, 2.500000000000000000, 3.537306695894645081 ) ) ;
#27815 = VERTEX_POINT ( 'NONE', #107747 ) ;
#27816 = CARTESIAN_POINT ( 'NONE',  ( -11.89999999999999503, 12.50000000000000000, 3.918623584224382839 ) ) ;
#27817 = VECTOR ( 'NONE', #7733, 1000.000000000000000 ) ;
#27819 = ORIENTED_EDGE ( 'NONE', *, *, #98033, .T. ) ;
#27818 = LINE ( 'NONE', #59243, #72444 ) ;
#27820 = DIRECTION ( 'NONE',  ( -4.274815082592931898E-19, -0.9999939076577903929, -0.003490651415223739937 ) ) ;
#27821 = DIRECTION ( 'NONE',  ( 0.000000000000000000, 1.000000000000000000, 0.000000000000000000 ) ) ;
#27822 = EDGE_LOOP ( 'NONE', ( #127485, #120002, #63055, #34759 ) ) ;
#27823 = EDGE_CURVE ( 'NONE', #66532, #54360, #109688, .T. ) ;
#27824 = ORIENTED_EDGE ( 'NONE', *, *, #56947, .T. ) ;
#27825 = VERTEX_POINT ( 'NONE', #9553 ) ;
#27826 = DIRECTION ( 'NONE',  ( 0.000000000000000000, 1.000000000000000000, 0.000000000000000000 ) ) ;
#27827 = FACE_OUTER_BOUND ( 'NONE', #120210, .T. ) ;
#27829 = DIRECTION ( 'NONE',  ( 0.000000000000000000, 0.000000000000000000, -1.000000000000000000 ) ) ;
#27828 = CONICAL_SURFACE ( 'NONE', #121823, 0.1000000000000002554, 0.003490658503988666988 ) ;
#27830 = CIRCLE ( 'NONE', #32065, 0.1000000000000002554 ) ;
#27831 = EDGE_CURVE ( 'NONE', #53467, #96425, #37723, .T. ) ;
#27832 = FACE_BOUND ( 'NONE', #76811, .T. ) ;
#27833 = VERTEX_POINT ( 'NONE', #57357 ) ;
#27834 = EDGE_CURVE ( 'NONE', #66455, #32421, #6936, .T. ) ;
#27835 = CARTESIAN_POINT ( 'NONE',  ( -5.200000000000025935, 2.500000000000000000, -4.083716857408426826 ) ) ;
#27836 = DIRECTION ( 'NONE',  ( 0.000000000000000000, 0.000000000000000000, 1.000000000000000000 ) ) ;
#27837 = ORIENTED_EDGE ( 'NONE', *, *, #110569, .T. ) ;
#27839 = CARTESIAN_POINT ( 'NONE',  ( -9.800000000000004263, 12.50000000000000000, 3.983716857408420076 ) ) ;
#27838 = VECTOR ( 'NONE', #23956, 1000.000000000000000 ) ;
#27840 = CIRCLE ( 'NONE', #59167, 0.09999999999999999167 ) ;
#27841 = CONICAL_SURFACE ( 'NONE', #86323, 0.1000000000000002554, 0.003490658503988666988 ) ;
#27842 = EDGE_CURVE ( 'NONE', #34384, #106414, #8678, .T. ) ;
#27844 = AXIS2_PLACEMENT_3D ( 'NONE', #94572, #95238, #96494 ) ;
#27843 = DIRECTION ( 'NONE',  ( -0.000000000000000000, -1.000000000000000000, -0.000000000000000000 ) ) ;
#27845 = ADVANCED_FACE ( 'NONE', ( #118210 ), #108942, .T. ) ;
#27846 = LINE ( 'NONE', #49446, #63296 ) ;
#27847 = EDGE_CURVE ( 'NONE', #107859, #128878, #125669, .T. ) ;
#27848 = PLANE ( 'NONE',  #101514 ) ;
#27849 = DIRECTION ( 'NONE',  ( 0.000000000000000000, 0.000000000000000000, -1.000000000000000000 ) ) ;
#27850 = VECTOR ( 'NONE', #29567, 1000.000000000000000 ) ;
#27851 = CONICAL_SURFACE ( 'NONE', #59174, 0.09999999999999999167, 0.003490658503988666988 ) ;
#27852 = VECTOR ( 'NONE', #12692, 1000.000000000000000 ) ;
#27853 = EDGE_CURVE ( 'NONE', #96425, #64421, #119410, .T. ) ;
#27854 = EDGE_LOOP ( 'NONE', ( #67558, #3818, #63685, #16098 ) ) ;
#27855 = VERTEX_POINT ( 'NONE', #58013 ) ;
#27856 = ORIENTED_EDGE ( 'NONE', *, *, #86034, .F. ) ;
#27857 = VERTEX_POINT ( 'NONE', #8885 ) ;
#27859 = EDGE_LOOP ( 'NONE', ( #59435, #3534, #18983, #101536 ) ) ;
#27858 = CONICAL_SURFACE ( 'NONE', #40397, 0.09999999999999999167, 0.003490658503988666988 ) ;
#27860 = LINE ( 'NONE', #18682, #119521 ) ;
#27861 = CIRCLE ( 'NONE', #9080, 0.1000000000000002554 ) ;
#27862 = LINE ( 'NONE', #67781, #2876 ) ;
#27863 = EDGE_LOOP ( 'NONE', ( #83414, #16814 ) ) ;
#27864 = ADVANCED_FACE ( 'NONE', ( #59317 ), #48841, .T. ) ;
#27865 = FACE_BOUND ( 'NONE', #124201, .T. ) ;
#27866 = ADVANCED_FACE ( 'NONE', ( #128712 ), #42262, .T. ) ;
#27867 = CIRCLE ( 'NONE', #61322, 1.000000000000000888 ) ;
#27868 = FACE_OUTER_BOUND ( 'NONE', #105802, .T. ) ;
#27869 = DIRECTION ( 'NONE',  ( 0.000000000000000000, 0.000000000000000000, 1.000000000000000000 ) ) ;
#27870 = DIRECTION ( 'NONE',  ( 0.000000000000000000, 1.000000000000000000, 0.000000000000000000 ) ) ;
#27871 = DIRECTION ( 'NONE',  ( -0.000000000000000000, -1.000000000000000000, -0.000000000000000000 ) ) ;
#27872 = FACE_OUTER_BOUND ( 'NONE', #16345, .T. ) ;
#27873 = EDGE_LOOP ( 'NONE', ( #45179, #80593, #42641, #90364 ) ) ;
#27874 = FACE_OUTER_BOUND ( 'NONE', #40802, .T. ) ;
#27875 = VECTOR ( 'NONE', #54530, 1000.000000000000000 ) ;
#27876 = ORIENTED_EDGE ( 'NONE', *, *, #92685, .F. ) ;
#27877 = VERTEX_POINT ( 'NONE', #48182 ) ;
#27878 = ORIENTED_EDGE ( 'NONE', *, *, #123662, .F. ) ;
#27879 = CARTESIAN_POINT ( 'NONE',  ( -3.150000000000029221, 2.500000000000000000, 2.511473670974873507 ) ) ;
#27880 = DIRECTION ( 'NONE',  ( 0.000000000000000000, 1.000000000000000000, 0.000000000000000000 ) ) ;
#27881 = CARTESIAN_POINT ( 'NONE',  ( 17.50000000000000355, -2.500000000000000000, -4.040567763475364060 ) ) ;
#27882 = ORIENTED_EDGE ( 'NONE', *, *, #15872, .F. ) ;
#27883 = CARTESIAN_POINT ( 'NONE',  ( 12.06068301339517390, 1.499999999999871436, -8.632777000277979340 ) ) ;
#27884 = AXIS2_PLACEMENT_3D ( 'NONE', #74222, #114776, #5460 ) ;
#27886 = DIRECTION ( 'NONE',  ( 0.000000000000000000, -0.000000000000000000, 1.000000000000000000 ) ) ;
#27885 = CIRCLE ( 'NONE', #44516, 0.09999999999999982514 ) ;
#27887 = PLANE ( 'NONE',  #89249 ) ;
#27888 = CARTESIAN_POINT ( 'NONE',  ( 11.24999999999990585, 12.50000000000000000, -5.867463478539787225 ) ) ;
#27889 = DIRECTION ( 'NONE',  ( -4.274815082592931898E-19, -0.9999939076577903929, -0.003490651415223739937 ) ) ;
#27890 = CARTESIAN_POINT ( 'NONE',  ( 9.599999999999914380, 12.50000000000000000, 5.022947341949748790 ) ) ;
#27891 = CARTESIAN_POINT ( 'NONE',  ( 2.699999999999947331, 2.500000000000000000, -4.776537180435978414 ) ) ;
#27892 = CONICAL_SURFACE ( 'NONE', #40439, 0.09999999999999982514, 0.003490658503988666988 ) ;
#27893 = ORIENTED_EDGE ( 'NONE', *, *, #80873, .T. ) ;
#27894 = DIRECTION ( 'NONE',  ( 0.000000000000000000, -0.000000000000000000, 1.000000000000000000 ) ) ;
#27895 = AXIS2_PLACEMENT_3D ( 'NONE', #65911, #46272, #76393 ) ;
#27896 = AXIS2_PLACEMENT_3D ( 'NONE', #120145, #10797, #11471 ) ;
#27897 = VERTEX_POINT ( 'NONE', #88074 ) ;
#27898 = CIRCLE ( 'NONE', #88522, 0.09999999999999982514 ) ;
#27899 = EDGE_CURVE ( 'NONE', #124875, #68434, #128032, .T. ) ;
#27900 = ORIENTED_EDGE ( 'NONE', *, *, #52508, .F. ) ;
#27901 = DIRECTION ( 'NONE',  ( 0.000000000000000000, 0.000000000000000000, 1.000000000000000000 ) ) ;
#27902 = EDGE_CURVE ( 'NONE', #30611, #107580, #111185, .T. ) ;
#27903 = CARTESIAN_POINT ( 'NONE',  ( 2.499999999999948930, 2.500000000000000000, -0.7928203230275542301 ) ) ;
#27904 = DIRECTION ( 'NONE',  ( 0.000000000000000000, 0.000000000000000000, 1.000000000000000000 ) ) ;
#27905 = AXIS2_PLACEMENT_3D ( 'NONE', #56992, #9197, #77934 ) ;
#27906 = ORIENTED_EDGE ( 'NONE', *, *, #126318, .F. ) ;
#27907 = VERTEX_POINT ( 'NONE', #12113 ) ;
#27908 = DIRECTION ( 'NONE',  ( 0.000000000000000000, 0.000000000000000000, 1.000000000000000000 ) ) ;
#27909 = CARTESIAN_POINT ( 'NONE',  ( 8.749999999999921840, 2.500000000000000000, 2.857883832488649301 ) ) ;
#27910 = AXIS2_PLACEMENT_3D ( 'NONE', #67028, #74942, #46123 ) ;
#27911 = AXIS2_PLACEMENT_3D ( 'NONE', #9558, #8251, #89403 ) ;
#27912 = DIRECTION ( 'NONE',  ( 0.000000000000000000, 0.000000000000000000, -1.000000000000000000 ) ) ;
#27913 = ORIENTED_EDGE ( 'NONE', *, *, #53160, .F. ) ;
#27914 = VERTEX_POINT ( 'NONE', #122724 ) ;
#27915 = CARTESIAN_POINT ( 'NONE',  ( -6.249999999999981348, 2.500000000000000000, 6.395190528383296602 ) ) ;
#27916 = AXIS2_PLACEMENT_3D ( 'NONE', #309, #8849, #19983 ) ;
#27917 = EDGE_LOOP ( 'NONE', ( #87129, #42352, #10195, #106893, #18727, #107926, #37885, #57074, #95702, #18397, #103397, #25314 ) ) ;
#27918 = CARTESIAN_POINT ( 'NONE',  ( 13.29999999999989946, 12.50000000000000000, -2.385244779468109755E-15 ) ) ;
#27919 = DIRECTION ( 'NONE',  ( 1.000000000000000000, 0.000000000000000000, 1.776356839400247112E-15 ) ) ;
#27920 = ORIENTED_EDGE ( 'NONE', *, *, #94666, .T. ) ;
#27921 = CARTESIAN_POINT ( 'NONE',  ( -5.800000000000018474, 2.500000000000000000, -0.1000000000000022815 ) ) ;
#27922 = FACE_OUTER_BOUND ( 'NONE', #31127, .T. ) ;
#27923 = DIRECTION ( 'NONE',  ( -0.000000000000000000, 1.000000000000000000, -0.000000000000000000 ) ) ;
#27924 = CARTESIAN_POINT ( 'NONE',  ( 0.1999999999999627909, 12.50000000000000000, 0.4115034346978132529 ) ) ;
#27925 = ORIENTED_EDGE ( 'NONE', *, *, #49430, .T. ) ;
#27926 = DIRECTION ( 'NONE',  ( 0.000000000000000000, 0.000000000000000000, 1.000000000000000000 ) ) ;
#27927 = ORIENTED_EDGE ( 'NONE', *, *, #118289, .T. ) ;
#27928 = ORIENTED_EDGE ( 'NONE', *, *, #43933, .F. ) ;
#27929 = CONICAL_SURFACE ( 'NONE', #103143, 0.1000000000000002554, 0.003490658503988666988 ) ;
#27930 = AXIS2_PLACEMENT_3D ( 'NONE', #124953, #35295, #73917 ) ;
#27931 = DIRECTION ( 'NONE',  ( -0.000000000000000000, -1.000000000000000000, -0.000000000000000000 ) ) ;
#27932 = DIRECTION ( 'NONE',  ( 0.000000000000000000, 1.000000000000000000, 0.000000000000000000 ) ) ;
#27933 = CARTESIAN_POINT ( 'NONE',  ( -8.950000000000009948, 2.500000000000000000, 2.511473670974873507 ) ) ;
#27934 = CARTESIAN_POINT ( 'NONE',  ( 9.399999999999918643, 2.500000000000000000, -0.3464101615137782364 ) ) ;
#27935 = CARTESIAN_POINT ( 'NONE',  ( -13.09999999999999254, 12.50000000000000000, 0.3464101615137777923 ) ) ;
#27936 = DIRECTION ( 'NONE',  ( 0.000000000000000000, 0.000000000000000000, -1.000000000000000000 ) ) ;
#27937 = EDGE_CURVE ( 'NONE', #127206, #115023, #48515, .T. ) ;
#27938 = VECTOR ( 'NONE', #124581, 1000.000000000000000 ) ;
#27939 = CIRCLE ( 'NONE', #17456, 0.06509327318403745899 ) ;
#27940 = DIRECTION ( 'NONE',  ( 0.000000000000000000, -0.000000000000000000, 1.000000000000000000 ) ) ;
#27941 = CARTESIAN_POINT ( 'NONE',  ( 14.34999999999989306, 2.500000000000000000, -1.818653347947326138 ) ) ;
#27943 = AXIS2_PLACEMENT_3D ( 'NONE', #74432, #44975, #44312 ) ;
#27942 = CARTESIAN_POINT ( 'NONE',  ( -9.400000000000007461, 2.500000000000000000, -0.4464101615137783252 ) ) ;
#27944 = VECTOR ( 'NONE', #31030, 1000.000000000000000 ) ;
#27945 = CARTESIAN_POINT ( 'NONE',  ( -7.950000000000016165, 2.500000000000000000, -6.395190528383296602 ) ) ;
#27946 = EDGE_CURVE ( 'NONE', #92039, #14604, #58984, .T. ) ;
#27947 = CONICAL_SURFACE ( 'NONE', #59271, 0.09999999999999982514, 0.003490658503988666988 ) ;
#27948 = AXIS2_PLACEMENT_3D ( 'NONE', #102287, #112107, #11958 ) ;
#27949 = AXIS2_PLACEMENT_3D ( 'NONE', #125249, #116705, #55226 ) ;
#27950 = EDGE_LOOP ( 'NONE', ( #114044, #15891, #108855, #83638 ) ) ;
#27951 = DIRECTION ( 'NONE',  ( 0.000000000000000000, 0.000000000000000000, 1.000000000000000000 ) ) ;
#27952 = CIRCLE ( 'NONE', #753, 0.06509327318403745899 ) ;
#27953 = ADVANCED_FACE ( 'NONE', ( #90018 ), #69328, .T. ) ;
#27954 = DIRECTION ( 'NONE',  ( 0.000000000000000000, 0.000000000000000000, 1.000000000000000000 ) ) ;
#27956 = EDGE_CURVE ( 'NONE', #100972, #91293, #91326, .T. ) ;
#27955 = DIRECTION ( 'NONE',  ( -4.274815082592931898E-19, -0.9999939076577903929, -0.003490651415223739937 ) ) ;
#27957 = CARTESIAN_POINT ( 'NONE',  ( -1.050000000000037348, 12.50000000000000000, -6.841600689897078702 ) ) ;
#27958 = DIRECTION ( 'NONE',  ( -4.274815082592931898E-19, -0.9999939076577903929, -0.003490651415223739937 ) ) ;
#27959 = ORIENTED_EDGE ( 'NONE', *, *, #116604, .T. ) ;
#27960 = DIRECTION ( 'NONE',  ( 0.000000000000000000, 0.000000000000000000, 1.000000000000000000 ) ) ;
#27961 = ADVANCED_FACE ( 'NONE', ( #71047 ), #92324, .T. ) ;
#27962 = DIRECTION ( 'NONE',  ( 0.000000000000000000, 0.000000000000000000, 1.000000000000000000 ) ) ;
#27964 = ORIENTED_EDGE ( 'NONE', *, *, #76774, .F. ) ;
#27963 = CARTESIAN_POINT ( 'NONE',  ( -4.350000000000027178, 2.500000000000000000, -6.741600689897077281 ) ) ;
#27965 = ADVANCED_FACE ( 'NONE', ( #59968 ), #35898, .T. ) ;
#27966 = AXIS2_PLACEMENT_3D ( 'NONE', #75316, #55036, #17002 ) ;
#27967 = ORIENTED_EDGE ( 'NONE', *, *, #129400, .F. ) ;
#27968 = VERTEX_POINT ( 'NONE', #72351 ) ;
#27969 = ORIENTED_EDGE ( 'NONE', *, *, #90793, .T. ) ;
#27970 = EDGE_LOOP ( 'NONE', ( #46516, #117415 ) ) ;
#27971 = DIRECTION ( 'NONE',  ( 0.000000000000000000, 1.000000000000000000, 0.000000000000000000 ) ) ;
#27973 = DIRECTION ( 'NONE',  ( -0.000000000000000000, -1.000000000000000000, -0.000000000000000000 ) ) ;
#27972 = VECTOR ( 'NONE', #61953, 1000.000000000000000 ) ;
#27974 = CARTESIAN_POINT ( 'NONE',  ( 0.8499999999999557909, 2.500000000000000000, -7.188010851410854052 ) ) ;
#27975 = AXIS2_PLACEMENT_3D ( 'NONE', #4644, #54413, #74706 ) ;
#27976 = CARTESIAN_POINT ( 'NONE',  ( -7.950000000000012612, 12.50000000000000000, 2.099970236277060032 ) ) ;
#27977 = CONICAL_SURFACE ( 'NONE', #115701, 0.1000000000000002554, 0.003490658503988666988 ) ;
#27978 = ORIENTED_EDGE ( 'NONE', *, *, #41327, .T. ) ;
#27979 = DIRECTION ( 'NONE',  ( 0.000000000000000000, 0.000000000000000000, 1.000000000000000000 ) ) ;
#27980 = ORIENTED_EDGE ( 'NONE', *, *, #122057, .F. ) ;
#27981 = CARTESIAN_POINT ( 'NONE',  ( 87.50000000000001421, -3.974992050023849810, -6.359987280038161828 ) ) ;
#27982 = CARTESIAN_POINT ( 'NONE',  ( 1.849999999999949685, 2.500000000000000000, -2.611473670974877592 ) ) ;
#27983 = CARTESIAN_POINT ( 'NONE',  ( 20.64614705759265689, 2.669560853936145950, 2.247897417617497062 ) ) ;
#27984 = DIRECTION ( 'NONE',  ( -0.000000000000000000, -1.000000000000000000, -0.000000000000000000 ) ) ;
#27985 = DIRECTION ( 'NONE',  ( -0.000000000000000000, 1.000000000000000000, -0.000000000000000000 ) ) ;
#27986 = AXIS2_PLACEMENT_3D ( 'NONE', #32475, #65102, #35669 ) ;
#27987 = VECTOR ( 'NONE', #100493, 1000.000000000000000 ) ;
#27988 = VERTEX_POINT ( 'NONE', #61886 ) ;
#27989 = EDGE_CURVE ( 'NONE', #14553, #120064, #10831, .T. ) ;
#27990 = ORIENTED_EDGE ( 'NONE', *, *, #53282, .T. ) ;
#27991 = ORIENTED_EDGE ( 'NONE', *, *, #21194, .F. ) ;
#27992 = EDGE_LOOP ( 'NONE', ( #104586, #83795, #77190, #39847 ) ) ;
#27993 = FACE_OUTER_BOUND ( 'NONE', #61070, .T. ) ;
#27994 = CARTESIAN_POINT ( 'NONE',  ( -0.8500000000000395017, 2.500000000000000000, 2.265063509461097357 ) ) ;
#27995 = CARTESIAN_POINT ( 'NONE',  ( 7.949999999999922018, 12.50000000000000000, -2.099970236277064473 ) ) ;
#27996 = ADVANCED_FACE ( 'NONE', ( #350 ), #71482, .T. ) ;
#27997 = FACE_BOUND ( 'NONE', #116922, .T. ) ;
#27998 = AXIS2_PLACEMENT_3D ( 'NONE', #108371, #18698, #98532 ) ;
#27999 = LINE ( 'NONE', #99324, #47328 ) ;
#28000 = DIRECTION ( 'NONE',  ( 0.000000000000000000, 0.000000000000000000, -1.000000000000000000 ) ) ;
#28001 = ADVANCED_FACE ( 'NONE', ( #110323 ), #56797, .T. ) ;
#28002 = DIRECTION ( 'NONE',  ( 0.000000000000000000, 1.000000000000000000, 0.000000000000000000 ) ) ;
#28003 = CARTESIAN_POINT ( 'NONE',  ( -3.350000000000028955, 2.500000000000000000, 2.265063509461097357 ) ) ;
#28004 = AXIS2_PLACEMENT_3D ( 'NONE', #7, #39951, #97565 ) ;
#28005 = EDGE_CURVE ( 'NONE', #110872, #117851, #109036, .T. ) ;
#28006 = CARTESIAN_POINT ( 'NONE',  ( 184.7135416670080588, 4.367472073101518859, -7.564683531249999149 ) ) ;
#28007 = EDGE_CURVE ( 'NONE', #34238, #49883, #54754, .T. ) ;
#28008 = DIRECTION ( 'NONE',  ( 0.000000000000000000, 0.000000000000000000, 1.000000000000000000 ) ) ;
#28009 = CONICAL_SURFACE ( 'NONE', #30084, 0.09999999999999982514, 0.003490658503988666988 ) ;
#28010 = ADVANCED_FACE ( 'NONE', ( #60601 ), #110946, .T. ) ;
#28011 = CARTESIAN_POINT ( 'NONE',  ( 10.64999999999991331, 2.500000000000000000, 6.841600689897072485 ) ) ;
#28012 = EDGE_CURVE ( 'NONE', #16978, #109486, #23358, .T. ) ;
#28013 = AXIS2_PLACEMENT_3D ( 'NONE', #16555, #66945, #118636 ) ;
#28014 = CARTESIAN_POINT ( 'NONE',  ( 1.849999999999951017, 12.50000000000000000, -6.148780366869526226 ) ) ;
#28015 = ADVANCED_FACE ( 'NONE', ( #90680 ), #17079, .T. ) ;
#28016 = ORIENTED_EDGE ( 'NONE', *, *, #80704, .F. ) ;
#28017 = ORIENTED_EDGE ( 'NONE', *, *, #64941, .T. ) ;
#28018 = EDGE_LOOP ( 'NONE', ( #126773, #106678, #55837, #23995 ) ) ;
#28019 = EDGE_LOOP ( 'NONE', ( #37687, #68687, #106413, #62644 ) ) ;
#28020 = PLANE ( 'NONE',  #61184 ) ;
#28021 = FACE_BOUND ( 'NONE', #107538, .T. ) ;
#28022 = EDGE_CURVE ( 'NONE', #12583, #38386, #80875, .T. ) ;
#28023 = DIRECTION ( 'NONE',  ( 0.000000000000000000, 0.000000000000000000, 1.000000000000000000 ) ) ;
#28024 = EDGE_CURVE ( 'NONE', #40294, #108133, #82158, .T. ) ;
#28025 = CONICAL_SURFACE ( 'NONE', #95215, 0.1000000000000000472, 0.003490658503988666988 ) ;
#28026 = ORIENTED_EDGE ( 'NONE', *, *, #110170, .F. ) ;
#28028 = AXIS2_PLACEMENT_3D ( 'NONE', #13692, #5162, #64733 ) ;
#28027 = LINE ( 'NONE', #17542, #128304 ) ;
#28029 = CARTESIAN_POINT ( 'NONE',  ( -7.100000000000017408, 2.500000000000000000, 0.6928203230275494784 ) ) ;
#28030 = FACE_OUTER_BOUND ( 'NONE', #103751, .T. ) ;
#28031 = EDGE_LOOP ( 'NONE', ( #72835, #59200 ) ) ;
#28032 = CARTESIAN_POINT ( 'NONE',  ( -4.800000000000028244, 12.50000000000000000, -3.918623584224389056 ) ) ;
#28033 = CARTESIAN_POINT ( 'NONE',  ( 5.649999999999934630, 2.500000000000000000, -1.918653347947325782 ) ) ;
#28034 = VECTOR ( 'NONE', #23807, 1000.000000000000000 ) ;
#28035 = CIRCLE ( 'NONE', #82433, 0.1000000000000002554 ) ;
#28036 = AXIS2_PLACEMENT_3D ( 'NONE', #99127, #89296, #129255 ) ;
#28038 = ORIENTED_EDGE ( 'NONE', *, *, #60524, .F. ) ;
#28037 = AXIS2_PLACEMENT_3D ( 'NONE', #118213, #99229, #59975 ) ;
#28039 = ORIENTED_EDGE ( 'NONE', *, *, #72789, .F. ) ;
#28040 = FACE_OUTER_BOUND ( 'NONE', #56397, .T. ) ;
#28041 = DIRECTION ( 'NONE',  ( 0.000000000000000000, 1.000000000000000000, 0.000000000000000000 ) ) ;
#28042 = AXIS2_PLACEMENT_3D ( 'NONE', #77859, #106679, #128281 ) ;
#28043 = AXIS2_PLACEMENT_3D ( 'NONE', #77916, #127666, #49134 ) ;
#28044 = CARTESIAN_POINT ( 'NONE',  ( -12.89999999999999325, 12.50000000000000000, 0.7579135962115910452 ) ) ;
#28045 = DIRECTION ( 'NONE',  ( 0.000000000000000000, 0.000000000000000000, 1.000000000000000000 ) ) ;
#28046 = VERTEX_POINT ( 'NONE', #101154 ) ;
#28047 = CARTESIAN_POINT ( 'NONE',  ( 9.999999999999912959, 12.50000000000000000, 3.637306695894644726 ) ) ;
#28049 = EDGE_LOOP ( 'NONE', ( #74921, #99021, #73423, #31811 ) ) ;
#28048 = VECTOR ( 'NONE', #113097, 1000.000000000000000 ) ;
#28050 = ORIENTED_EDGE ( 'NONE', *, *, #113067, .T. ) ;
#28051 = DIRECTION ( 'NONE',  ( 0.000000000000000000, 0.000000000000000000, 1.000000000000000000 ) ) ;
#28052 = ORIENTED_EDGE ( 'NONE', *, *, #90273, .T. ) ;
#28053 = DIRECTION ( 'NONE',  ( 0.000000000000000000, 1.000000000000000000, 0.000000000000000000 ) ) ;
#28054 = FACE_BOUND ( 'NONE', #87674, .T. ) ;
#28055 = ORIENTED_EDGE ( 'NONE', *, *, #116787, .T. ) ;
#28056 = EDGE_CURVE ( 'NONE', #68041, #121003, #11474, .T. ) ;
#28057 = DIRECTION ( 'NONE',  ( 0.000000000000000000, 0.000000000000000000, 1.000000000000000000 ) ) ;
#28058 = EDGE_LOOP ( 'NONE', ( #124245, #129578, #58225, #39817 ) ) ;
#28059 = CARTESIAN_POINT ( 'NONE',  ( -7.500000000000001776, 1.500000000000000000, 1.734723475976807094E-15 ) ) ;
#28060 = CARTESIAN_POINT ( 'NONE',  ( 5.599999999999931255, 2.500000000000000000, 4.776537180435972196 ) ) ;
#28061 = CARTESIAN_POINT ( 'NONE',  ( -11.25000000000000000, 12.50000000000000000, -7.122917578226813262 ) ) ;
#28062 = CARTESIAN_POINT ( 'NONE',  ( 9.999999999999911182, 2.500000000000000000, 5.122947341949749323 ) ) ;
#28063 = CARTESIAN_POINT ( 'NONE',  ( -5.650000000000019895, 2.500000000000000000, 1.918653347947321564 ) ) ;
#28064 = VECTOR ( 'NONE', #66778, 1000.000000000000000 ) ;
#28065 = ORIENTED_EDGE ( 'NONE', *, *, #41935, .F. ) ;
#28066 = ORIENTED_EDGE ( 'NONE', *, *, #106160, .F. ) ;
#28067 = ADVANCED_FACE ( 'NONE', ( #116595 ), #57025, .T. ) ;
#28068 = VERTEX_POINT ( 'NONE', #34360 ) ;
#28069 = DIRECTION ( 'NONE',  ( 0.000000000000000000, 0.000000000000000000, 1.000000000000000000 ) ) ;
#28070 = DIRECTION ( 'NONE',  ( -4.274815082592931898E-19, -0.9999939076577903929, -0.003490651415223739937 ) ) ;
#28071 = PLANE ( 'NONE',  #4112 ) ;
#28073 = ORIENTED_EDGE ( 'NONE', *, *, #74952, .F. ) ;
#28072 = ORIENTED_EDGE ( 'NONE', *, *, #19260, .T. ) ;
#28074 = ORIENTED_EDGE ( 'NONE', *, *, #37097, .T. ) ;
#28075 = FACE_OUTER_BOUND ( 'NONE', #92954, .T. ) ;
#28076 = AXIS2_PLACEMENT_3D ( 'NONE', #109811, #106731, #59446 ) ;
#28077 = LINE ( 'NONE', #7776, #92512 ) ;
#28078 =( NAMED_UNIT ( * ) SI_UNIT ( $, .STERADIAN. ) SOLID_ANGLE_UNIT ( ) );
#28079 = DIRECTION ( 'NONE',  ( -0.000000000000000000, -1.000000000000000000, -0.000000000000000000 ) ) ;
#28080 = DIRECTION ( 'NONE',  ( 0.000000000000000000, 1.000000000000000000, 0.000000000000000000 ) ) ;
#28081 = CARTESIAN_POINT ( 'NONE',  ( 6.899999999999926636, 2.500000000000000000, -0.2464101615137782308 ) ) ;
#28082 = CARTESIAN_POINT ( 'NONE',  ( -6.900000000000015454, 2.500000000000000000, 3.983716857408420076 ) ) ;
#28083 = CARTESIAN_POINT ( 'NONE',  ( 0.6499999999999561684, 2.500000000000000000, 2.511473670974873507 ) ) ;
#28084 = DIRECTION ( 'NONE',  ( 0.000000000000000000, -0.000000000000000000, 1.000000000000000000 ) ) ;
#28085 = ORIENTED_EDGE ( 'NONE', *, *, #75489, .T. ) ;
#28086 = ORIENTED_EDGE ( 'NONE', *, *, #39967, .F. ) ;
#28087 = AXIS2_PLACEMENT_3D ( 'NONE', #68375, #78215, #18630 ) ;
#28088 = DIRECTION ( 'NONE',  ( -4.274815082592931898E-19, -0.9999939076577903929, -0.003490651415223739937 ) ) ;
#28089 = DIRECTION ( 'NONE',  ( 0.000000000000000000, 0.000000000000000000, -1.000000000000000000 ) ) ;
#28090 = ORIENTED_EDGE ( 'NONE', *, *, #103481, .T. ) ;
#28091 = ORIENTED_EDGE ( 'NONE', *, *, #2756, .F. ) ;
#28092 = CARTESIAN_POINT ( 'NONE',  ( 187.2760416670080588, 6.551208109652274736, 3.782341765625001351 ) ) ;
#28093 = DIRECTION ( 'NONE',  ( 0.000000000000000000, 0.000000000000000000, -1.000000000000000000 ) ) ;
#28094 = DIRECTION ( 'NONE',  ( 0.000000000000000000, -0.9999939076577903929, 0.003490651415223739937 ) ) ;
#28095 = CARTESIAN_POINT ( 'NONE',  ( 11.24999999999994493, 2.500000000000000000, -2.165063509461101710 ) ) ;
#28096 = CARTESIAN_POINT ( 'NONE',  ( 185.1250000000000000, -8.891194145520236347, -1.633285867636356299E-15 ) ) ;
#28097 = VECTOR ( 'NONE', #91103, 1000.000000000000000 ) ;
#28098 = FACE_OUTER_BOUND ( 'NONE', #113668, .T. ) ;
#28099 = CIRCLE ( 'NONE', #49048, 0.06509327318403745899 ) ;
#28100 = DIRECTION ( 'NONE',  ( 0.000000000000000000, 1.000000000000000000, 0.000000000000000000 ) ) ;
#28101 = ORIENTED_EDGE ( 'NONE', *, *, #26705, .T. ) ;
#28102 = DIRECTION ( 'NONE',  ( 0.000000000000000000, 0.000000000000000000, -1.000000000000000000 ) ) ;
#28103 = AXIS2_PLACEMENT_3D ( 'NONE', #128353, #8530, #48480 ) ;
#28104 = CIRCLE ( 'NONE', #90791, 0.1000000000000000056 ) ;
#28105 = CARTESIAN_POINT ( 'NONE',  ( 12.49999999999990230, 2.500000000000000000, -0.6928203230275541413 ) ) ;
#28106 = EDGE_CURVE ( 'NONE', #117378, #111575, #125759, .T. ) ;
#28107 = ORIENTED_EDGE ( 'NONE', *, *, #120172, .T. ) ;
#28108 = EDGE_LOOP ( 'NONE', ( #96840, #35753, #80213, #108616 ) ) ;
#28109 = EDGE_CURVE ( 'NONE', #62965, #63975, #31796, .T. ) ;
#28110 = ORIENTED_EDGE ( 'NONE', *, *, #31836, .T. ) ;
#28111 = ORIENTED_EDGE ( 'NONE', *, *, #83838, .T. ) ;
#28112 = EDGE_CURVE ( 'NONE', #11241, #52697, #106980, .T. ) ;
#28113 = CARTESIAN_POINT ( 'NONE',  ( -10.60000000000000142, 2.500000000000000000, 0.2464101615137736789 ) ) ;
#28114 = CARTESIAN_POINT ( 'NONE',  ( 2.949999999999945111, 12.50000000000000000, 2.099970236277060032 ) ) ;
#28115 = ORIENTED_EDGE ( 'NONE', *, *, #66266, .F. ) ;
#28116 = DIRECTION ( 'NONE',  ( 0.000000000000000000, -0.000000000000000000, 1.000000000000000000 ) ) ;
#28117 = CARTESIAN_POINT ( 'NONE',  ( 17.50000000000000000, 2.750000000000000000, -3.999999999999998224 ) ) ;
#28118 = CIRCLE ( 'NONE', #46903, 0.1000000000000002554 ) ;
#28119 = EDGE_CURVE ( 'NONE', #3070, #121018, #90253, .T. ) ;
#28120 = CONICAL_SURFACE ( 'NONE', #78210, 0.1000000000000002554, 0.003490658503988666988 ) ;
#28121 = FACE_OUTER_BOUND ( 'NONE', #22848, .T. ) ;
#28124 = ORIENTED_EDGE ( 'NONE', *, *, #33883, .T. ) ;
#28123 = ADVANCED_FACE ( 'NONE', ( #87136 ), #102779, .T. ) ;
#28122 = CARTESIAN_POINT ( 'NONE',  ( -10.65000000000000391, 12.50000000000000000, -2.576566944158911188 ) ) ;
#28125 = VECTOR ( 'NONE', #73634, 1000.000000000000000 ) ;
#28126 = VECTOR ( 'NONE', #92773, 1000.000000000000000 ) ;
#28127 = EDGE_CURVE ( 'NONE', #4240, #39644, #40106, .T. ) ;
#28128 = CARTESIAN_POINT ( 'NONE',  ( -4.400000000000025224, 12.50000000000000000, 4.611443907251934426 ) ) ;
#28129 = DIRECTION ( 'NONE',  ( 0.000000000000000000, 1.000000000000000000, 0.000000000000000000 ) ) ;
#28130 = VERTEX_POINT ( 'NONE', #96959 ) ;
#28131 = AXIS2_PLACEMENT_3D ( 'NONE', #89572, #69938, #109865 ) ;
#28132 = AXIS2_PLACEMENT_3D ( 'NONE', #17051, #54432, #44625 ) ;
#28133 = VECTOR ( 'NONE', #84635, 1000.000000000000000 ) ;
#28134 = ORIENTED_EDGE ( 'NONE', *, *, #126215, .F. ) ;
#28135 = ORIENTED_EDGE ( 'NONE', *, *, #67657, .T. ) ;
#28136 = CARTESIAN_POINT ( 'NONE',  ( 9.599999999999914380, 12.50000000000000000, 4.330127018922196314 ) ) ;
#28137 = DIRECTION ( 'NONE',  ( 0.000000000000000000, 0.000000000000000000, -1.000000000000000000 ) ) ;
#28138 = CONICAL_SURFACE ( 'NONE', #101299, 0.1000000000000002554, 0.003490658503988666988 ) ;
#28139 = AXIS2_PLACEMENT_3D ( 'NONE', #85005, #85655, #45103 ) ;
#28140 = AXIS2_PLACEMENT_3D ( 'NONE', #96661, #120199, #39730 ) ;
#28141 = EDGE_LOOP ( 'NONE', ( #98036, #88352, #41696, #37971 ) ) ;
#28142 = CARTESIAN_POINT ( 'NONE',  ( -4.600000000000024514, 12.50000000000000000, 5.022947341949748790 ) ) ;
#28143 = CARTESIAN_POINT ( 'NONE',  ( -1.250000000000037970, 2.500000000000000000, 7.188010851410848723 ) ) ;
#28144 = DIRECTION ( 'NONE',  ( 0.000000000000000000, 0.000000000000000000, -1.000000000000000000 ) ) ;
#28145 = DIRECTION ( 'NONE',  ( 0.000000000000000000, 1.000000000000000000, 0.000000000000000000 ) ) ;
#28146 = EDGE_LOOP ( 'NONE', ( #4665, #26954 ) ) ;
#28147 = PLANE ( 'NONE',  #43672 ) ;
#28148 = ORIENTED_EDGE ( 'NONE', *, *, #50888, .F. ) ;
#28149 = ORIENTED_EDGE ( 'NONE', *, *, #87530, .F. ) ;
#28150 = DIRECTION ( 'NONE',  ( 0.000000000000000000, -0.000000000000000000, 1.000000000000000000 ) ) ;
#28151 = CARTESIAN_POINT ( 'NONE',  ( 11.04999999999990656, 12.50000000000000000, 2.511473670974873507 ) ) ;
#28152 = FACE_BOUND ( 'NONE', #91597, .T. ) ;
#28153 = DIRECTION ( 'NONE',  ( 0.000000000000000000, 0.000000000000000000, 1.000000000000000000 ) ) ;
#28154 = AXIS2_PLACEMENT_3D ( 'NONE', #6030, #5395, #4100 ) ;
#28155 = CARTESIAN_POINT ( 'NONE',  ( -2.700000000000029932, 2.500000000000000000, -4.576537180435977348 ) ) ;
#28156 = DIRECTION ( 'NONE',  ( 0.000000000000000000, 0.000000000000000000, 1.000000000000000000 ) ) ;
#28157 = EDGE_CURVE ( 'NONE', #86941, #69063, #61021, .T. ) ;
#28158 = ORIENTED_EDGE ( 'NONE', *, *, #104223, .T. ) ;
#28159 = ADVANCED_FACE ( 'NONE', ( #43537 ), #26304, .T. ) ;
#28160 = DIRECTION ( 'NONE',  ( 0.000000000000000000, 1.000000000000000000, 0.000000000000000000 ) ) ;
#28161 = DIRECTION ( 'NONE',  ( 0.000000000000000000, 1.000000000000000000, 0.000000000000000000 ) ) ;
#28162 = CARTESIAN_POINT ( 'NONE',  ( -14.54999999999998472, 12.50000000000000000, 2.165063509461101265 ) ) ;
#28163 = ADVANCED_FACE ( 'NONE', ( #113543 ), #7929, .T. ) ;
#28164 = DIRECTION ( 'NONE',  ( -0.000000000000000000, -1.000000000000000000, -0.000000000000000000 ) ) ;
#28165 = ORIENTED_EDGE ( 'NONE', *, *, #126756, .T. ) ;
#28166 = AXIS2_PLACEMENT_3D ( 'NONE', #126208, #56163, #97385 ) ;
#28167 = FACE_OUTER_BOUND ( 'NONE', #29931, .T. ) ;
#28168 = DIRECTION ( 'NONE',  ( -0.000000000000000000, -1.000000000000000000, -0.000000000000000000 ) ) ;
#28169 = EDGE_CURVE ( 'NONE', #60091, #121535, #65217, .T. ) ;
#28170 = EDGE_LOOP ( 'NONE', ( #103371, #34330, #27230, #76634 ) ) ;
#28171 = EDGE_LOOP ( 'NONE', ( #56334, #114784, #29958, #74155 ) ) ;
#28172 = DIRECTION ( 'NONE',  ( 0.000000000000000000, -0.000000000000000000, 1.000000000000000000 ) ) ;
#28173 = DIRECTION ( 'NONE',  ( -0.000000000000000000, -1.000000000000000000, -0.000000000000000000 ) ) ;
#28174 = FACE_BOUND ( 'NONE', #22265, .T. ) ;
#28175 = DIRECTION ( 'NONE',  ( 0.000000000000000000, 0.000000000000000000, -1.000000000000000000 ) ) ;
#28176 = EDGE_CURVE ( 'NONE', #14119, #64139, #4560, .T. ) ;
#28177 = CONICAL_SURFACE ( 'NONE', #19869, 0.1000000000000002554, 0.003490658503988666988 ) ;
#28178 = EDGE_CURVE ( 'NONE', #120246, #98907, #123364, .T. ) ;
#28179 = VERTEX_POINT ( 'NONE', #77323 ) ;
#28180 = LINE ( 'NONE', #68088, #69573 ) ;
#28181 = AXIS2_PLACEMENT_3D ( 'NONE', #118486, #28840, #89041 ) ;
#28182 = ORIENTED_EDGE ( 'NONE', *, *, #109428, .T. ) ;
#28183 = ORIENTED_EDGE ( 'NONE', *, *, #16280, .F. ) ;
#28184 = DIRECTION ( 'NONE',  ( 0.000000000000000000, 0.000000000000000000, -1.000000000000000000 ) ) ;
#28185 = CARTESIAN_POINT ( 'NONE',  ( 186.5833333333333144, -6.668395609140180369, 3.849999999999994760 ) ) ;
#28186 = EDGE_CURVE ( 'NONE', #14788, #11702, #17172, .T. ) ;
#28187 = ORIENTED_EDGE ( 'NONE', *, *, #81972, .T. ) ;
#28188 = LINE ( 'NONE', #100155, #21802 ) ;
#28189 = DIRECTION ( 'NONE',  ( 0.000000000000000000, -0.9999939076577903929, 0.003490651415223739937 ) ) ;
#28190 = AXIS2_PLACEMENT_3D ( 'NONE', #111211, #121049, #111886 ) ;
#28191 = AXIS2_PLACEMENT_3D ( 'NONE', #50406, #83593, #72484 ) ;
#28192 = CARTESIAN_POINT ( 'NONE',  ( 3.949999999999941558, 12.50000000000000000, -1.818653347947326138 ) ) ;
#28193 = DIRECTION ( 'NONE',  ( 0.000000000000000000, -0.000000000000000000, 1.000000000000000000 ) ) ;
#28194 = AXIS2_PLACEMENT_3D ( 'NONE', #123454, #125402, #84174 ) ;
#28195 = EDGE_LOOP ( 'NONE', ( #38481, #77465 ) ) ;
#28196 = CARTESIAN_POINT ( 'NONE',  ( -1.250000000000037970, 2.500000000000000000, 7.188010851410848723 ) ) ;
#28197 = DIRECTION ( 'NONE',  ( -0.000000000000000000, 1.000000000000000000, -0.000000000000000000 ) ) ;
#28198 = CARTESIAN_POINT ( 'NONE',  ( -10.45000000000000462, 2.500000000000000000, -6.395190528383298378 ) ) ;
#28199 = DIRECTION ( 'NONE',  ( 0.000000000000000000, 0.000000000000000000, 1.000000000000000000 ) ) ;
#28200 = VERTEX_POINT ( 'NONE', #63808 ) ;
#28201 = CARTESIAN_POINT ( 'NONE',  ( 14.14999999999989200, 12.50000000000000000, -2.165063509461101710 ) ) ;
#28202 = ORIENTED_EDGE ( 'NONE', *, *, #125313, .F. ) ;
#28203 = CARTESIAN_POINT ( 'NONE',  ( 17.46754094667558377, 1.506946019333248898, 5.249106724335526941 ) ) ;
#28204 = EDGE_LOOP ( 'NONE', ( #18163, #19868 ) ) ;
#28205 = PLANE ( 'NONE',  #107825 ) ;
#28206 = LINE ( 'NONE', #119159, #51545 ) ;
#28207 = DIRECTION ( 'NONE',  ( -0.000000000000000000, 1.000000000000000000, -0.000000000000000000 ) ) ;
#28209 = DIRECTION ( 'NONE',  ( -0.000000000000000000, -1.000000000000000000, -0.000000000000000000 ) ) ;
#28208 = CIRCLE ( 'NONE', #122310, 0.06509327318403745899 ) ;
#28210 = EDGE_LOOP ( 'NONE', ( #77891, #123182, #92206, #99342 ) ) ;
#28211 = AXIS2_PLACEMENT_3D ( 'NONE', #27935, #58056, #30542 ) ;
#28212 = DIRECTION ( 'NONE',  ( 0.000000000000000000, 1.000000000000000000, 0.000000000000000000 ) ) ;
#28213 = DIRECTION ( 'NONE',  ( -4.274815082592931898E-19, -0.9999939076577903929, -0.003490651415223739937 ) ) ;
#28214 = DIRECTION ( 'NONE',  ( -4.274815082592931898E-19, -0.9999939076577903929, -0.003490651415223739937 ) ) ;
#28215 = AXIS2_PLACEMENT_3D ( 'NONE', #113370, #103570, #72179 ) ;
#28216 = DIRECTION ( 'NONE',  ( -0.000000000000000000, -1.000000000000000000, -0.000000000000000000 ) ) ;
#28217 = CARTESIAN_POINT ( 'NONE',  ( -2.950000000000030376, 2.500000000000000000, 6.395190528383296602 ) ) ;
#28218 = CARTESIAN_POINT ( 'NONE',  ( -4.350000000000023626, 2.500000000000000000, 2.411473670974873862 ) ) ;
#28219 = VECTOR ( 'NONE', #31635, 1000.000000000000000 ) ;
#28220 = ORIENTED_EDGE ( 'NONE', *, *, #70111, .T. ) ;
#28221 = EDGE_CURVE ( 'NONE', #82798, #62529, #44157, .T. ) ;
#28223 = VERTEX_POINT ( 'NONE', #106143 ) ;
#28222 = CIRCLE ( 'NONE', #5217, 0.06509327318403745899 ) ;
#28225 = CARTESIAN_POINT ( 'NONE',  ( 8.749999999999921840, 2.500000000000000000, 2.857883832488649301 ) ) ;
#28224 = CONICAL_SURFACE ( 'NONE', #101385, 0.1000000000000002554, 0.003490658503988666988 ) ;
#28226 = VERTEX_POINT ( 'NONE', #103736 ) ;
#28227 = DIRECTION ( 'NONE',  ( 0.000000000000000000, 1.000000000000000000, 0.000000000000000000 ) ) ;
#28230 = ORIENTED_EDGE ( 'NONE', *, *, #38468, .F. ) ;
#28229 = VERTEX_POINT ( 'NONE', #67475 ) ;
#28228 = AXIS2_PLACEMENT_3D ( 'NONE', #23446, #63380, #115685 ) ;
#28231 = ORIENTED_EDGE ( 'NONE', *, *, #90789, .F. ) ;
#28232 = DIRECTION ( 'NONE',  ( 0.000000000000000000, -0.000000000000000000, 1.000000000000000000 ) ) ;
#28234 = CONICAL_SURFACE ( 'NONE', #26176, 0.1000000000000002554, 0.003490658503988666988 ) ;
#28233 = LINE ( 'NONE', #30177, #52713 ) ;
#28235 = CARTESIAN_POINT ( 'NONE',  ( -2.500000000000032419, 2.500000000000000000, 0.6928203230275494784 ) ) ;
#28236 = DIRECTION ( 'NONE',  ( -0.000000000000000000, 1.000000000000000000, -0.000000000000000000 ) ) ;
#28237 = DIRECTION ( 'NONE',  ( 0.000000000000000000, 0.000000000000000000, -1.000000000000000000 ) ) ;
#28238 = VECTOR ( 'NONE', #55797, 1000.000000000000000 ) ;
#28239 = CARTESIAN_POINT ( 'NONE',  ( -3.100000000000028955, 12.50000000000000000, 4.611443907251934426 ) ) ;
#28240 = FACE_OUTER_BOUND ( 'NONE', #121858, .T. ) ;
#28241 = DIRECTION ( 'NONE',  ( -0.000000000000000000, -1.000000000000000000, -0.000000000000000000 ) ) ;
#28242 = ORIENTED_EDGE ( 'NONE', *, *, #71396, .T. ) ;
#28243 = ORIENTED_EDGE ( 'NONE', *, *, #39421, .T. ) ;
#28244 = VERTEX_POINT ( 'NONE', #17747 ) ;
#28245 = DIRECTION ( 'NONE',  ( 0.000000000000000000, -0.9999939076577903929, 0.003490651415223739937 ) ) ;
#28246 = ORIENTED_EDGE ( 'NONE', *, *, #86622, .F. ) ;
#28247 = ORIENTED_EDGE ( 'NONE', *, *, #2173, .F. ) ;
#28248 = AXIS2_PLACEMENT_3D ( 'NONE', #98363, #8683, #48637 ) ;
#28249 = DIRECTION ( 'NONE',  ( 0.000000000000000000, 0.000000000000000000, -1.000000000000000000 ) ) ;
#28250 = CARTESIAN_POINT ( 'NONE',  ( 8.749999999999920064, 2.500000000000000000, -2.857883832488653741 ) ) ;
#28251 = DIRECTION ( 'NONE',  ( -0.000000000000000000, -1.000000000000000000, -0.000000000000000000 ) ) ;
#28252 = DIRECTION ( 'NONE',  ( 0.000000000000000000, 1.000000000000000000, 0.000000000000000000 ) ) ;
#28253 = DIRECTION ( 'NONE',  ( 0.000000000000000000, 0.000000000000000000, -1.000000000000000000 ) ) ;
#28254 = ORIENTED_EDGE ( 'NONE', *, *, #63067, .F. ) ;
#28255 = EDGE_CURVE ( 'NONE', #45160, #98077, #93913, .T. ) ;
#28256 = DIRECTION ( 'NONE',  ( 0.000000000000000000, 1.000000000000000000, 0.000000000000000000 ) ) ;
#28257 = AXIS2_PLACEMENT_3D ( 'NONE', #101128, #71663, #71028 ) ;
#28258 = AXIS2_PLACEMENT_3D ( 'NONE', #48294, #100599, #88184 ) ;
#28259 = VERTEX_POINT ( 'NONE', #53983 ) ;
#28260 = DIRECTION ( 'NONE',  ( -0.000000000000000000, 1.000000000000000000, -0.000000000000000000 ) ) ;
#28261 = ADVANCED_FACE ( 'NONE', ( #39364 ), #9877, .T. ) ;
#28262 = EDGE_LOOP ( 'NONE', ( #21531, #60440 ) ) ;
#28263 = CARTESIAN_POINT ( 'NONE',  ( -4.150000000000025224, 12.50000000000000000, -1.407149913249512663 ) ) ;
#28264 = EDGE_LOOP ( 'NONE', ( #94205, #47057, #37085, #46226 ) ) ;
#28265 = EDGE_CURVE ( 'NONE', #121714, #36406, #28233, .T. ) ;
#28266 = ORIENTED_EDGE ( 'NONE', *, *, #125776, .F. ) ;
#28267 = EDGE_CURVE ( 'NONE', #19758, #57799, #19246, .T. ) ;
#28268 = DIRECTION ( 'NONE',  ( 0.000000000000000000, 1.000000000000000000, 0.000000000000000000 ) ) ;
#28269 = CARTESIAN_POINT ( 'NONE',  ( 10.39999999999991154, 2.500000000000000000, 4.922947341949748257 ) ) ;
#28270 = AXIS2_PLACEMENT_3D ( 'NONE', #112024, #24931, #121829 ) ;
#28271 = DIRECTION ( 'NONE',  ( 0.000000000000000000, 1.000000000000000000, 0.000000000000000000 ) ) ;
#28272 = CARTESIAN_POINT ( 'NONE',  ( 3.949999999999940670, 2.500000000000000000, 1.818653347947321475 ) ) ;
#28273 = ADVANCED_FACE ( 'NONE', ( #28884 ), #2616, .T. ) ;
#28274 = LINE ( 'NONE', #18448, #114093 ) ;
#28276 = ORIENTED_EDGE ( 'NONE', *, *, #11623, .T. ) ;
#28275 = EDGE_CURVE ( 'NONE', #26422, #57522, #75779, .T. ) ;
#28277 = CARTESIAN_POINT ( 'NONE',  ( 3.949999999999938005, 2.500000000000000000, 6.941600689897073018 ) ) ;
#28278 = DIRECTION ( 'NONE',  ( 0.000000000000000000, 0.000000000000000000, -1.000000000000000000 ) ) ;
#28279 = EDGE_CURVE ( 'NONE', #51573, #12542, #73631, .T. ) ;
#28280 = DIRECTION ( 'NONE',  ( -0.000000000000000000, 1.000000000000000000, -0.000000000000000000 ) ) ;
#28281 = EDGE_CURVE ( 'NONE', #121393, #36999, #18405, .T. ) ;
#28282 = ADVANCED_FACE ( 'NONE', ( #98245 ), #79905, .T. ) ;
#28283 = CARTESIAN_POINT ( 'NONE',  ( -4.800000000000024691, 2.500000000000000000, 0.4464101615137735513 ) ) ;
#28284 = CARTESIAN_POINT ( 'NONE',  ( 4.549999999999939426, 12.50000000000000000, -6.560283801567339701 ) ) ;
#28285 = ORIENTED_EDGE ( 'NONE', *, *, #118703, .T. ) ;
#28286 = CIRCLE ( 'NONE', #82677, 0.06509327318403745899 ) ;
#28287 = CONICAL_SURFACE ( 'NONE', #30451, 0.09999999999999982514, 0.003490658503988666988 ) ;
#28288 = VERTEX_POINT ( 'NONE', #99558 ) ;
#28289 = DIRECTION ( 'NONE',  ( 0.000000000000000000, 0.000000000000000000, 1.000000000000000000 ) ) ;
#28290 = EDGE_CURVE ( 'NONE', #113580, #99802, #88420, .T. ) ;
#28291 = ORIENTED_EDGE ( 'NONE', *, *, #77132, .F. ) ;
#28292 = DIRECTION ( 'NONE',  ( 0.000000000000000000, 0.000000000000000000, 1.000000000000000000 ) ) ;
#28293 = CARTESIAN_POINT ( 'NONE',  ( 184.5000000000000000, 0.000000000000000000, 0.000000000000000000 ) ) ;
#28294 = VERTEX_POINT ( 'NONE', #119185 ) ;
#28295 = CARTESIAN_POINT ( 'NONE',  ( 185.0833333333333144, -6.668395609140180369, 3.849999999999994760 ) ) ;
#28296 = DIRECTION ( 'NONE',  ( -0.000000000000000000, -1.000000000000000000, -0.000000000000000000 ) ) ;
#28297 = DIRECTION ( 'NONE',  ( -4.274815082592931898E-19, -0.9999939076577903929, -0.003490651415223739937 ) ) ;
#28298 = AXIS2_PLACEMENT_3D ( 'NONE', #113888, #5839, #75884 ) ;
#28299 = DIRECTION ( 'NONE',  ( 0.000000000000000000, 0.000000000000000000, 1.000000000000000000 ) ) ;
#28300 = ORIENTED_EDGE ( 'NONE', *, *, #112280, .T. ) ;
#28301 = CIRCLE ( 'NONE', #107718, 0.09999999999999999167 ) ;
#28302 = CARTESIAN_POINT ( 'NONE',  ( 10.84999999999990905, 12.50000000000000000, 2.792790559304612064 ) ) ;
#28303 = CONICAL_SURFACE ( 'NONE', #74279, 0.1000000000000002554, 0.003490658503988666988 ) ;
#28304 = EDGE_LOOP ( 'NONE', ( #67637, #6082 ) ) ;
#28305 = AXIS2_PLACEMENT_3D ( 'NONE', #86484, #127076, #104199 ) ;
#28306 = DIRECTION ( 'NONE',  ( 0.000000000000000000, 0.000000000000000000, 1.000000000000000000 ) ) ;
#28307 = CARTESIAN_POINT ( 'NONE',  ( -10.00000000000000355, 2.500000000000000000, 3.737306695894644371 ) ) ;
#28308 = CARTESIAN_POINT ( 'NONE',  ( 8.549999999999922551, 12.50000000000000000, 2.511473670974873507 ) ) ;
#28309 = AXIS2_PLACEMENT_3D ( 'NONE', #42769, #53216, #113407 ) ;
#28310 = AXIS2_PLACEMENT_3D ( 'NONE', #39185, #107247, #58172 ) ;
#28311 = ORIENTED_EDGE ( 'NONE', *, *, #3650, .T. ) ;
#28312 = AXIS2_PLACEMENT_3D ( 'NONE', #5385, #95714, #103605 ) ;
#28313 = CARTESIAN_POINT ( 'NONE',  ( -0.8500000000000382805, 2.500000000000000000, -2.957883832488653830 ) ) ;
#28314 = CONICAL_SURFACE ( 'NONE', #24112, 0.1000000000000002554, 0.003490658503988666988 ) ;
#28315 = ORIENTED_EDGE ( 'NONE', *, *, #69473, .F. ) ;
#28316 = EDGE_CURVE ( 'NONE', #84188, #102542, #458, .T. ) ;
#28317 = DIRECTION ( 'NONE',  ( -0.000000000000000000, -1.000000000000000000, -0.000000000000000000 ) ) ;
#28318 = DIRECTION ( 'NONE',  ( -0.000000000000000000, 1.000000000000000000, -0.000000000000000000 ) ) ;
#28319 = CARTESIAN_POINT ( 'NONE',  ( 12.69999999999990337, 2.500000000000000000, -4.676537180435978769 ) ) ;
#28320 = ADVANCED_FACE ( 'NONE', ( #110019 ), #88288, .T. ) ;
#28321 = ORIENTED_EDGE ( 'NONE', *, *, #8365, .F. ) ;
#28322 = AXIS2_PLACEMENT_3D ( 'NONE', #103120, #123396, #4902 ) ;
#28323 = DIRECTION ( 'NONE',  ( 0.000000000000000000, -0.9999939076577903929, 0.003490651415223739937 ) ) ;
#28324 = EDGE_CURVE ( 'NONE', #70717, #53411, #11150, .T. ) ;
#28325 = CIRCLE ( 'NONE', #17846, 0.06509327318403745899 ) ;
#28326 = CARTESIAN_POINT ( 'NONE',  ( -4.150000000000025224, 2.500000000000000000, 6.495190528383297135 ) ) ;
#28327 = CIRCLE ( 'NONE', #45063, 0.06509327318403745899 ) ;
#28328 = ORIENTED_EDGE ( 'NONE', *, *, #18913, .F. ) ;
#28329 = DIRECTION ( 'NONE',  ( 0.000000000000000000, 0.000000000000000000, 1.000000000000000000 ) ) ;
#28330 = EDGE_CURVE ( 'NONE', #58403, #37993, #68793, .T. ) ;
#28331 = EDGE_LOOP ( 'NONE', ( #27422, #96551, #90662, #28496 ) ) ;
#28332 = DIRECTION ( 'NONE',  ( 0.000000000000000000, 0.000000000000000000, 1.000000000000000000 ) ) ;
#28333 = ADVANCED_FACE ( 'NONE', ( #58980 ), #94562, .T. ) ;
#28334 = EDGE_CURVE ( 'NONE', #92046, #126222, #86137, .T. ) ;
#28335 = ADVANCED_FACE ( 'NONE', ( #89720 ), #90349, .T. ) ;
#28336 = ORIENTED_EDGE ( 'NONE', *, *, #64731, .F. ) ;
#28337 = FACE_OUTER_BOUND ( 'NONE', #3699, .T. ) ;
#28338 = CARTESIAN_POINT ( 'NONE',  ( -2.900000000000029221, 12.50000000000000000, -0.6928203230275541413 ) ) ;
#28339 = VERTEX_POINT ( 'NONE', #46 ) ;
#28340 = ORIENTED_EDGE ( 'NONE', *, *, #24868, .T. ) ;
#28341 = CARTESIAN_POINT ( 'NONE',  ( -5.450000000000023270, 2.500000000000000000, -2.265063509461101798 ) ) ;
#28342 = DIRECTION ( 'NONE',  ( 0.000000000000000000, 0.000000000000000000, -1.000000000000000000 ) ) ;
#28343 = CIRCLE ( 'NONE', #114024, 0.06509327318403745899 ) ;
#28344 = VERTEX_POINT ( 'NONE', #40654 ) ;
#28345 = ADVANCED_FACE ( 'NONE', ( #80559 ), #110648, .T. ) ;
#28346 = CARTESIAN_POINT ( 'NONE',  ( 185.7500000000000000, 9.429780353434619030E-16, -7.700000000000000178 ) ) ;
#28347 = CARTESIAN_POINT ( 'NONE',  ( 186.9010416670080588, -4.367472073101520635, 7.564683531249999149 ) ) ;
#28348 = DIRECTION ( 'NONE',  ( 0.000000000000000000, 0.000000000000000000, -1.000000000000000000 ) ) ;
#28349 = DIRECTION ( 'NONE',  ( 0.000000000000000000, 1.000000000000000000, 0.000000000000000000 ) ) ;
#28350 = DIRECTION ( 'NONE',  ( 0.000000000000000000, 0.000000000000000000, -1.000000000000000000 ) ) ;
#28351 = CIRCLE ( 'NONE', #95251, 0.06509327318403745899 ) ;
#28352 = DIRECTION ( 'NONE',  ( -0.000000000000000000, 1.000000000000000000, -0.000000000000000000 ) ) ;
#28353 = AXIS2_PLACEMENT_3D ( 'NONE', #102398, #52636, #92570 ) ;
#28354 = CIRCLE ( 'NONE', #11616, 0.1000000000000002554 ) ;
#28355 = VERTEX_POINT ( 'NONE', #111267 ) ;
#28356 = EDGE_LOOP ( 'NONE', ( #35725, #111168, #91710, #86549 ) ) ;
#28357 = ORIENTED_EDGE ( 'NONE', *, *, #94927, .F. ) ;
#28358 = ORIENTED_EDGE ( 'NONE', *, *, #66384, .F. ) ;
#28359 = DIRECTION ( 'NONE',  ( 0.000000000000000000, 0.000000000000000000, 1.000000000000000000 ) ) ;
#28360 = DIRECTION ( 'NONE',  ( 0.000000000000000000, 1.000000000000000000, 0.000000000000000000 ) ) ;
#28361 = FACE_OUTER_BOUND ( 'NONE', #48251, .T. ) ;
#28362 = ORIENTED_EDGE ( 'NONE', *, *, #79261, .T. ) ;
#28363 = FACE_BOUND ( 'NONE', #95157, .T. ) ;
#28364 = ORIENTED_EDGE ( 'NONE', *, *, #28852, .T. ) ;
#28365 = EDGE_CURVE ( 'NONE', #72890, #53599, #19341, .T. ) ;
#28366 = DIRECTION ( 'NONE',  ( 0.000000000000000000, 0.000000000000000000, -1.000000000000000000 ) ) ;
#28367 = LINE ( 'NONE', #116724, #110735 ) ;
#28368 = AXIS2_PLACEMENT_3D ( 'NONE', #48433, #110577, #69350 ) ;
#28369 = DIRECTION ( 'NONE',  ( 0.000000000000000000, 1.000000000000000000, 0.000000000000000000 ) ) ;
#28370 = DIRECTION ( 'NONE',  ( 0.000000000000000000, 0.000000000000000000, -1.000000000000000000 ) ) ;
#28371 = CIRCLE ( 'NONE', #107778, 0.09999999999999999167 ) ;
#28372 = CARTESIAN_POINT ( 'NONE',  ( 10.64999999999991331, 2.500000000000000000, -2.511473670974877948 ) ) ;
#28373 = FACE_OUTER_BOUND ( 'NONE', #16661, .T. ) ;
#28374 = DIRECTION ( 'NONE',  ( 0.000000000000000000, 1.000000000000000000, 0.000000000000000000 ) ) ;
#28375 = DIRECTION ( 'NONE',  ( -0.000000000000000000, 1.000000000000000000, -0.000000000000000000 ) ) ;
#28376 = DIRECTION ( 'NONE',  ( 0.000000000000000000, 0.000000000000000000, 1.000000000000000000 ) ) ;
#28377 = DIRECTION ( 'NONE',  ( 0.000000000000000000, 1.000000000000000000, 0.000000000000000000 ) ) ;
#28378 = AXIS2_PLACEMENT_3D ( 'NONE', #68898, #10601, #128495 ) ;
#28379 = EDGE_LOOP ( 'NONE', ( #76009, #105372, #64495, #86529 ) ) ;
#28380 = ORIENTED_EDGE ( 'NONE', *, *, #118599, .T. ) ;
#28381 = CIRCLE ( 'NONE', #53515, 0.1000000000000002554 ) ;
#28382 = ADVANCED_FACE ( 'NONE', ( #2612 ), #72670, .T. ) ;
#28383 = ORIENTED_EDGE ( 'NONE', *, *, #29904, .T. ) ;
#28384 = ORIENTED_EDGE ( 'NONE', *, *, #27785, .T. ) ;
#28385 = CARTESIAN_POINT ( 'NONE',  ( 17.50000000000010303, -2.262036863574762080, -3.993716676846037039 ) ) ;
#28386 = FACE_OUTER_BOUND ( 'NONE', #31820, .T. ) ;
#28388 = EDGE_LOOP ( 'NONE', ( #8754, #14308, #75389, #77275 ) ) ;
#28387 = ORIENTED_EDGE ( 'NONE', *, *, #122864, .T. ) ;
#28389 = ORIENTED_EDGE ( 'NONE', *, *, #13815, .F. ) ;
#28390 = DIRECTION ( 'NONE',  ( 0.000000000000000000, 1.000000000000000000, 0.000000000000000000 ) ) ;
#28391 = LINE ( 'NONE', #68295, #69714 ) ;
#28392 = CARTESIAN_POINT ( 'NONE',  ( 185.8333333333333144, 6.668395609140177704, -3.849999999999998312 ) ) ;
#28393 = CARTESIAN_POINT ( 'NONE',  ( 5.399999999999932854, 12.50000000000000000, 5.022947341949748790 ) ) ;
#28394 = CARTESIAN_POINT ( 'NONE',  ( -13.54999999999999005, 2.500000000000000000, 2.411473670974877415 ) ) ;
#28395 = PLANE ( 'NONE',  #37216 ) ;
#28396 = PLANE ( 'NONE',  #44493 ) ;
#28397 = EDGE_CURVE ( 'NONE', #2959, #41590, #100815, .T. ) ;
#28398 = ORIENTED_EDGE ( 'NONE', *, *, #61896, .F. ) ;
#28399 = LINE ( 'NONE', #9402, #39252 ) ;
#28400 = VERTEX_POINT ( 'NONE', #73295 ) ;
#28402 = VERTEX_POINT ( 'NONE', #64125 ) ;
#28401 = AXIS2_PLACEMENT_3D ( 'NONE', #80046, #20491, #70232 ) ;
#28403 = VERTEX_POINT ( 'NONE', #14365 ) ;
#28404 = AXIS2_PLACEMENT_3D ( 'NONE', #36176, #13934, #65616 ) ;
#28405 = CARTESIAN_POINT ( 'NONE',  ( -10.00000000000000533, 12.50000000000000000, 0.7579135962115869374 ) ) ;
#28406 =( BOUNDED_SURFACE ( )  B_SPLINE_SURFACE ( 3, 2, ( 
 ( #51022, #1894, #77089 ),
 ( #116354, #56144, #84325 ),
 ( #94146, #37177, #126185 ),
 ( #16838, #24127, #5743 ),
 ( #36537, #45705, #105904 ),
 ( #16207, #75158, #96078 ),
 ( #44405, #6375, #46330 ),
 ( #86242, #125534, #65317 ),
 ( #76447, #115055, #26058 ),
 ( #45068, #105254, #5111 ),
 ( #64046, #24773, #85612 ),
 ( #94794, #115709, #64683 ),
 ( #4444, #35877, #15573 ),
 ( #26698, #25389, #55521 ) ),
 .UNSPECIFIED., .F., .F., .F. ) 
 B_SPLINE_SURFACE_WITH_KNOTS ( ( 4, 2, 2, 2, 2, 2, 4 ),
 ( 3, 3 ),
 ( 0.000000000000000000, 0.001744612550434199941, 0.002616918825651300129, 0.003489225100868399883, 0.005233837651302600258, 0.006106143926519700012, 0.006978450201736799766 ),
 ( 0.000000000000000000, 1.000000000000000000 ),
 .UNSPECIFIED. ) 
 GEOMETRIC_REPRESENTATION_ITEM ( )  RATIONAL_B_SPLINE_SURFACE ( (
 ( 1.000000000000000000, 0.7318752858502181047, 1.000000000000000000),
 ( 1.000000000000000000, 0.7270130115578827823, 1.000000000000000000),
 ( 1.000000000000000000, 0.7223762446139352367, 1.000000000000000000),
 ( 1.000000000000000000, 0.7156127915551185881, 1.000000000000000000),
 ( 1.000000000000000000, 0.7133893117692130525, 1.000000000000000000),
 ( 1.000000000000000000, 0.7090389252573708889, 1.000000000000000000),
 ( 1.000000000000000000, 0.7069297463491673872, 1.000000000000000000),
 ( 1.000000000000000000, 0.7010696893200437652, 1.000000000000000000),
 ( 1.000000000000000000, 0.6977361265600255935, 1.000000000000000000),
 ( 1.000000000000000000, 0.6948030504687735531, 1.000000000000000000),
 ( 1.000000000000000000, 0.6942033558614377764, 1.000000000000000000),
 ( 1.000000000000000000, 0.6937817651809667918, 1.000000000000000000),
 ( 1.000000000000000000, 0.6939284133496244067, 1.000000000000000000),
 ( 1.000000000000000000, 0.6944177883068211043, 1.000000000000000000) ) ) 
 REPRESENTATION_ITEM ( '' )  SURFACE ( )  );
#28407 = ORIENTED_EDGE ( 'NONE', *, *, #87397, .F. ) ;
#28408 = EDGE_LOOP ( 'NONE', ( #50937, #3857, #22322, #39492 ) ) ;
#28409 = DIRECTION ( 'NONE',  ( 0.000000000000000000, 0.000000000000000000, 1.000000000000000000 ) ) ;
#28410 = CARTESIAN_POINT ( 'NONE',  ( -14.54999999999998472, 2.500000000000000000, 2.165063509461101265 ) ) ;
#28411 = FACE_OUTER_BOUND ( 'NONE', #128065, .T. ) ;
#28412 = LINE ( 'NONE', #79450, #117325 ) ;
#28413 = AXIS2_PLACEMENT_3D ( 'NONE', #76268, #106365, #27797 ) ;
#28414 = DIRECTION ( 'NONE',  ( 0.000000000000000000, 0.000000000000000000, 1.000000000000000000 ) ) ;
#28415 = ORIENTED_EDGE ( 'NONE', *, *, #111934, .T. ) ;
#28416 = CARTESIAN_POINT ( 'NONE',  ( -8.150000000000012790, 2.500000000000000000, -2.511473670974877948 ) ) ;
#28417 = CIRCLE ( 'NONE', #68101, 0.1000000000000002554 ) ;
#28418 = VECTOR ( 'NONE', #12416, 1000.000000000000000 ) ;
#28419 = VERTEX_POINT ( 'NONE', #73951 ) ;
#28420 = CARTESIAN_POINT ( 'NONE',  ( -3.100000000000028955, 12.50000000000000000, 3.983716857408420964 ) ) ;
#28422 = EDGE_CURVE ( 'NONE', #82111, #56575, #83767, .T. ) ;
#28421 = CIRCLE ( 'NONE', #86988, 0.06509327318403745899 ) ;
#28423 = VERTEX_POINT ( 'NONE', #71354 ) ;
#28424 = CARTESIAN_POINT ( 'NONE',  ( 111.9633609056390071, 8.147017582221319998, -3.065257838783662425 ) ) ;
#28425 = DIRECTION ( 'NONE',  ( 0.000000000000000000, -0.000000000000000000, 1.000000000000000000 ) ) ;
#28426 = AXIS2_PLACEMENT_3D ( 'NONE', #62104, #575, #42466 ) ;
#28427 = ORIENTED_EDGE ( 'NONE', *, *, #29444, .F. ) ;
#28428 = CARTESIAN_POINT ( 'NONE',  ( -10.20000000000000284, 2.500000000000000000, 3.983716857408420964 ) ) ;
#28429 = DIRECTION ( 'NONE',  ( -0.000000000000000000, 1.000000000000000000, -0.000000000000000000 ) ) ;
#28430 = EDGE_LOOP ( 'NONE', ( #17466, #63927, #121957, #113228 ) ) ;
#28431 = CARTESIAN_POINT ( 'NONE',  ( 1.649999999999951505, 12.50000000000000000, -1.472243186433550122 ) ) ;
#28432 = ORIENTED_EDGE ( 'NONE', *, *, #41924, .T. ) ;
#28433 = EDGE_CURVE ( 'NONE', #104247, #113011, #63181, .T. ) ;
#28435 = ORIENTED_EDGE ( 'NONE', *, *, #62279, .T. ) ;
#28434 = EDGE_CURVE ( 'NONE', #45891, #41822, #128023, .T. ) ;
#28436 = CARTESIAN_POINT ( 'NONE',  ( -6.850000000000017408, 12.50000000000000000, -1.883746621131363375 ) ) ;
#28437 = DIRECTION ( 'NONE',  ( 0.000000000000000000, 1.000000000000000000, 0.000000000000000000 ) ) ;
#28438 = EDGE_CURVE ( 'NONE', #117751, #50154, #46444, .T. ) ;
#28439 = CARTESIAN_POINT ( 'NONE',  ( 186.7968750003414300, 8.734944146203032389, 5.348610694689227483E-16 ) ) ;
#28440 = EDGE_CURVE ( 'NONE', #122530, #23542, #96605, .T. ) ;
#28441 = CIRCLE ( 'NONE', #128806, 0.06509327318403745899 ) ;
#28442 = CARTESIAN_POINT ( 'NONE',  ( 2.699999999999946443, 12.50000000000000000, -3.983716857408426293 ) ) ;
#28443 = DIRECTION ( 'NONE',  ( 0.000000000000000000, -0.000000000000000000, 1.000000000000000000 ) ) ;
#28444 = EDGE_CURVE ( 'NONE', #110699, #55428, #103416, .T. ) ;
#28445 = FACE_OUTER_BOUND ( 'NONE', #61866, .T. ) ;
#28446 = TOROIDAL_SURFACE ( 'NONE', #101599, 3.500000000000000000, 0.5000000000000000000 ) ;
#28447 = ADVANCED_FACE ( 'NONE', ( #92959 ), #81202, .T. ) ;
#28448 = ORIENTED_EDGE ( 'NONE', *, *, #30231, .T. ) ;
#28449 = CIRCLE ( 'NONE', #84869, 0.06509327318403745899 ) ;
#28450 = ADVANCED_FACE ( 'NONE', ( #61572 ), #3278, .T. ) ;
#28451 = CARTESIAN_POINT ( 'NONE',  ( 9.799999999999913669, 12.50000000000000000, -3.983716857408426293 ) ) ;
#28452 = CARTESIAN_POINT ( 'NONE',  ( -11.64999999999999680, 12.50000000000000000, 2.792790559304612064 ) ) ;
#28453 = ADVANCED_FACE ( 'NONE', ( #53664 ), #31881, .T. ) ;
#28454 = AXIS2_PLACEMENT_3D ( 'NONE', #105450, #75328, #115897 ) ;
#28455 = ORIENTED_EDGE ( 'NONE', *, *, #4711, .T. ) ;
#28456 = PRODUCT_DEFINITION ( 'UNKNOWN', '', #14983, #28761 ) ;
#28457 = FACE_OUTER_BOUND ( 'NONE', #112395, .T. ) ;
#28458 = CARTESIAN_POINT ( 'NONE',  ( 13.14999999999990088, 2.500000000000000000, 1.818653347947321475 ) ) ;
#28459 = DIRECTION ( 'NONE',  ( -4.274815082592931898E-19, -0.9999939076577903929, -0.003490651415223739937 ) ) ;
#28460 = FACE_BOUND ( 'NONE', #63190, .T. ) ;
#28461 = EDGE_CURVE ( 'NONE', #116195, #111299, #75682, .T. ) ;
#28462 = DIRECTION ( 'NONE',  ( 0.000000000000000000, 1.000000000000000000, 0.000000000000000000 ) ) ;
#28463 = ORIENTED_EDGE ( 'NONE', *, *, #22204, .F. ) ;
#28465 = CIRCLE ( 'NONE', #66009, 0.06509327318403741736 ) ;
#28464 = CIRCLE ( 'NONE', #101625, 0.09999999999999982514 ) ;
#28466 = DIRECTION ( 'NONE',  ( 0.000000000000000000, 0.000000000000000000, 1.000000000000000000 ) ) ;
#28467 = DIRECTION ( 'NONE',  ( 0.000000000000000000, 1.000000000000000000, 0.000000000000000000 ) ) ;
#28468 = ORIENTED_EDGE ( 'NONE', *, *, #101012, .T. ) ;
#28469 = CARTESIAN_POINT ( 'NONE',  ( -1.450000000000035039, 2.500000000000000000, -2.411473670974877859 ) ) ;
#28470 = VERTEX_POINT ( 'NONE', #24209 ) ;
#28471 = VERTEX_POINT ( 'NONE', #104055 ) ;
#28472 = DIRECTION ( 'NONE',  ( 1.000000000000000000, -0.000000000000000000, -7.228014483236698281E-17 ) ) ;
#28473 = ORIENTED_EDGE ( 'NONE', *, *, #95656, .F. ) ;
#28474 = PLANE ( 'NONE',  #579 ) ;
#28475 = DIRECTION ( 'NONE',  ( 0.000000000000000000, 0.000000000000000000, 1.000000000000000000 ) ) ;
#28476 = DIRECTION ( 'NONE',  ( -0.000000000000000000, -1.000000000000000000, -0.000000000000000000 ) ) ;
#28477 = EDGE_LOOP ( 'NONE', ( #51552, #74574, #53341, #52571 ) ) ;
#28478 = DIRECTION ( 'NONE',  ( 0.000000000000000000, -0.000000000000000000, 1.000000000000000000 ) ) ;
#28480 = ORIENTED_EDGE ( 'NONE', *, *, #110617, .T. ) ;
#28479 = LINE ( 'NONE', #40228, #22286 ) ;
#28481 = CARTESIAN_POINT ( 'NONE',  ( 12.89999999999990266, 2.500000000000000000, -3.637306695894650055 ) ) ;
#28482 = DIRECTION ( 'NONE',  ( 0.000000000000000000, 0.000000000000000000, -1.000000000000000000 ) ) ;
#28483 = EDGE_LOOP ( 'NONE', ( #113187, #52915 ) ) ;
#28484 = ADVANCED_FACE ( 'NONE', ( #11801 ), #51741, .T. ) ;
#28485 = ORIENTED_EDGE ( 'NONE', *, *, #639, .F. ) ;
#28486 = AXIS2_PLACEMENT_3D ( 'NONE', #72082, #120527, #70775 ) ;
#28487 = EDGE_CURVE ( 'NONE', #19960, #106590, #121750, .T. ) ;
#28488 = ORIENTED_EDGE ( 'NONE', *, *, #25963, .T. ) ;
#28489 = PLANE ( 'NONE',  #58846 ) ;
#28490 = CARTESIAN_POINT ( 'NONE',  ( 11.24999999999990941, 12.50000000000000000, -1.407149913249512663 ) ) ;
#28491 = FACE_OUTER_BOUND ( 'NONE', #5178, .T. ) ;
#28492 = FACE_BOUND ( 'NONE', #28895, .T. ) ;
#28493 = ORIENTED_EDGE ( 'NONE', *, *, #110889, .F. ) ;
#28494 = CARTESIAN_POINT ( 'NONE',  ( 187.5000000000000000, 0.000000000000000000, 0.000000000000000000 ) ) ;
#28495 = CARTESIAN_POINT ( 'NONE',  ( 2.099999999999949463, 12.50000000000000000, -3.637306695894650055 ) ) ;
#28496 = ORIENTED_EDGE ( 'NONE', *, *, #67725, .T. ) ;
#28497 = EDGE_CURVE ( 'NONE', #71388, #35640, #8873, .T. ) ;
#28499 = AXIS2_PLACEMENT_3D ( 'NONE', #11587, #51528, #101907 ) ;
#28498 = AXIS2_PLACEMENT_3D ( 'NONE', #44879, #75593, #53402 ) ;
#28500 = DIRECTION ( 'NONE',  ( 0.000000000000000000, 0.000000000000000000, -1.000000000000000000 ) ) ;
#28501 = CARTESIAN_POINT ( 'NONE',  ( -9.400000000000009237, 12.50000000000000000, -4.676537180435974328 ) ) ;
#28502 = DIRECTION ( 'NONE',  ( 0.000000000000000000, -0.9999939076577903929, 0.003490651415223739937 ) ) ;
#28503 = CARTESIAN_POINT ( 'NONE',  ( -10.00000000000000711, 2.500000000000000000, -3.637306695894645614 ) ) ;
#28504 = CARTESIAN_POINT ( 'NONE',  ( 17.50000000000000000, 2.500000000000000000, -2.922290670089280340 ) ) ;
#28505 = DIRECTION ( 'NONE',  ( 0.000000000000000000, 0.000000000000000000, 1.000000000000000000 ) ) ;
#28506 = DIRECTION ( 'NONE',  ( 0.000000000000000000, 0.000000000000000000, 1.000000000000000000 ) ) ;
#28508 = VECTOR ( 'NONE', #74044, 1000.000000000000000 ) ;
#28507 = AXIS2_PLACEMENT_3D ( 'NONE', #72867, #121969, #112796 ) ;
#28509 = CIRCLE ( 'NONE', #87071, 0.06509327318403745899 ) ;
#28510 = ORIENTED_EDGE ( 'NONE', *, *, #91218, .F. ) ;
#28511 = ORIENTED_EDGE ( 'NONE', *, *, #29904, .F. ) ;
#28512 = ORIENTED_EDGE ( 'NONE', *, *, #32433, .F. ) ;
#28513 = VERTEX_POINT ( 'NONE', #25477 ) ;
#28514 = ORIENTED_EDGE ( 'NONE', *, *, #36333, .T. ) ;
#28515 = DIRECTION ( 'NONE',  ( -0.000000000000000000, 1.000000000000000000, -0.000000000000000000 ) ) ;
#28516 = CARTESIAN_POINT ( 'NONE',  ( 11.24999999999994493, 2.500000000000000000, -2.165063509461101710 ) ) ;
#28517 = EDGE_LOOP ( 'NONE', ( #106353, #107598, #43677, #31607 ) ) ;
#28518 = FACE_BOUND ( 'NONE', #33640, .T. ) ;
#28519 = DIRECTION ( 'NONE',  ( -0.000000000000000000, 1.000000000000000000, -0.000000000000000000 ) ) ;
#28520 = DIRECTION ( 'NONE',  ( 0.000000000000000000, 0.000000000000000000, 1.000000000000000000 ) ) ;
#28521 = CARTESIAN_POINT ( 'NONE',  ( 2.299999999999949640, 12.50000000000000000, -4.676537180435977881 ) ) ;
#28522 = CARTESIAN_POINT ( 'NONE',  ( -6.850000000000017408, 2.500000000000000000, -1.818653347947325916 ) ) ;
#28523 = DIRECTION ( 'NONE',  ( 0.000000000000000000, 0.000000000000000000, 1.000000000000000000 ) ) ;
#28525 = VERTEX_POINT ( 'NONE', #46410 ) ;
#28524 = CIRCLE ( 'NONE', #43293, 0.1000000000000002554 ) ;
#28526 = CARTESIAN_POINT ( 'NONE',  ( 12.69999999999989804, 12.50000000000000000, 0.3464101615137735735 ) ) ;
#28527 = ORIENTED_EDGE ( 'NONE', *, *, #80300, .T. ) ;
#28528 = CONICAL_SURFACE ( 'NONE', #95425, 0.09999999999999982514, 0.003490658503988666988 ) ;
#28529 = EDGE_LOOP ( 'NONE', ( #34449, #66550 ) ) ;
#28530 = ORIENTED_EDGE ( 'NONE', *, *, #3846, .F. ) ;
#28531 = DIRECTION ( 'NONE',  ( 0.000000000000000000, 1.000000000000000000, 0.000000000000000000 ) ) ;
#28532 = CARTESIAN_POINT ( 'NONE',  ( 3.549999999999944755, 12.50000000000000000, -2.446380397790840266 ) ) ;
#28533 = CARTESIAN_POINT ( 'NONE',  ( -5.200000000000020606, 12.50000000000000000, -0.3464101615137782364 ) ) ;
#28534 = ORIENTED_EDGE ( 'NONE', *, *, #16883, .F. ) ;
#28535 = DIRECTION ( 'NONE',  ( 0.000000000000000000, 1.000000000000000000, 0.000000000000000000 ) ) ;
#28536 = AXIS2_PLACEMENT_3D ( 'NONE', #108511, #64238, #78439 ) ;
#28537 = AXIS2_PLACEMENT_3D ( 'NONE', #62952, #120588, #72781 ) ;
#28538 = DIRECTION ( 'NONE',  ( 0.000000000000000000, 0.000000000000000000, 1.000000000000000000 ) ) ;
#28539 = VECTOR ( 'NONE', #32710, 1000.000000000000000 ) ;
#28540 = DIRECTION ( 'NONE',  ( 0.000000000000000000, -0.000000000000000000, 1.000000000000000000 ) ) ;
#28541 = CARTESIAN_POINT ( 'NONE',  ( 185.5260416670080588, -6.551208109652273848, -3.782341765625003571 ) ) ;
#28542 = DIRECTION ( 'NONE',  ( 0.000000000000000000, -0.000000000000000000, 1.000000000000000000 ) ) ;
#28543 = CARTESIAN_POINT ( 'NONE',  ( 6.649999999999928413, 12.50000000000000000, 2.857883832488649301 ) ) ;
#28544 = ADVANCED_FACE ( 'NONE', ( #17591 ), #126926, .T. ) ;
#28545 = DIRECTION ( 'NONE',  ( 0.000000000000000000, 1.000000000000000000, 0.000000000000000000 ) ) ;
#28546 = ADVANCED_FACE ( 'NONE', ( #67315 ), #115477, .T. ) ;
#28547 = ORIENTED_EDGE ( 'NONE', *, *, #17766, .T. ) ;
#28548 = CARTESIAN_POINT ( 'NONE',  ( -5.450000000000023270, 2.500000000000000000, -2.065063509461102065 ) ) ;
#28549 = AXIS2_PLACEMENT_3D ( 'NONE', #35576, #74206, #44751 ) ;
#28550 = ORIENTED_EDGE ( 'NONE', *, *, #114001, .F. ) ;
#28552 = AXIS2_PLACEMENT_3D ( 'NONE', #123197, #33530, #93727 ) ;
#28551 = AXIS2_PLACEMENT_3D ( 'NONE', #111787, #122898, #43710 ) ;
#28553 = ORIENTED_EDGE ( 'NONE', *, *, #79641, .T. ) ;
#28554 = DIRECTION ( 'NONE',  ( 0.000000000000000000, 1.000000000000000000, 0.000000000000000000 ) ) ;
#28555 = DIRECTION ( 'NONE',  ( 0.000000000000000000, 0.000000000000000000, 1.000000000000000000 ) ) ;
#28557 = EDGE_CURVE ( 'NONE', #10201, #114690, #77841, .T. ) ;
#28556 = CARTESIAN_POINT ( 'NONE',  ( 8.749999999999923617, 12.50000000000000000, -7.253104124594891289 ) ) ;
#28558 = ORIENTED_EDGE ( 'NONE', *, *, #6333, .T. ) ;
#28559 = ORIENTED_EDGE ( 'NONE', *, *, #10121, .T. ) ;
#28560 = DIRECTION ( 'NONE',  ( -0.000000000000000000, 1.000000000000000000, -0.000000000000000000 ) ) ;
#28561 = DIRECTION ( 'NONE',  ( 0.000000000000000000, 1.000000000000000000, 0.000000000000000000 ) ) ;
#28562 = DIRECTION ( 'NONE',  ( -0.000000000000000000, 1.000000000000000000, -0.000000000000000000 ) ) ;
#28563 = ORIENTED_EDGE ( 'NONE', *, *, #110020, .T. ) ;
#28564 = ORIENTED_EDGE ( 'NONE', *, *, #58484, .T. ) ;
#28565 = CARTESIAN_POINT ( 'NONE',  ( 8.349999999999923261, 12.50000000000000000, 2.165063509461097713 ) ) ;
#28566 = VERTEX_POINT ( 'NONE', #15652 ) ;
#28567 = DIRECTION ( 'NONE',  ( 0.000000000000000000, 0.000000000000000000, -1.000000000000000000 ) ) ;
#28568 = FACE_OUTER_BOUND ( 'NONE', #106617, .T. ) ;
#28569 = ORIENTED_EDGE ( 'NONE', *, *, #15008, .F. ) ;
#28570 = CARTESIAN_POINT ( 'NONE',  ( -7.700000000000016165, 2.500000000000000000, -3.983716857408426293 ) ) ;
#28571 = ADVANCED_FACE ( 'NONE', ( #74594 ), #12986, .T. ) ;
#28572 = CARTESIAN_POINT ( 'NONE',  ( 8.149999999999923972, 12.50000000000000000, -6.841600689897077814 ) ) ;
#28573 = FACE_BOUND ( 'NONE', #61024, .T. ) ;
#28574 = CARTESIAN_POINT ( 'NONE',  ( 6.899999999999928413, 12.50000000000000000, -3.983716857408426293 ) ) ;
#28575 = ORIENTED_EDGE ( 'NONE', *, *, #68195, .F. ) ;
#28576 = EDGE_CURVE ( 'NONE', #115529, #68346, #82045, .T. ) ;
#28577 = DIRECTION ( 'NONE',  ( 0.000000000000000000, 0.000000000000000000, -1.000000000000000000 ) ) ;
#28578 = AXIS2_PLACEMENT_3D ( 'NONE', #91000, #121736, #69413 ) ;
#28579 = VECTOR ( 'NONE', #15702, 1000.000000000000000 ) ;
#28580 = ORIENTED_EDGE ( 'NONE', *, *, #46969, .F. ) ;
#28581 = ORIENTED_EDGE ( 'NONE', *, *, #108528, .T. ) ;
#28582 = EDGE_CURVE ( 'NONE', #109502, #96511, #107082, .T. ) ;
#28583 = EDGE_CURVE ( 'NONE', #21308, #92121, #76534, .T. ) ;
#28584 = DIRECTION ( 'NONE',  ( 0.000000000000000000, 0.000000000000000000, 1.000000000000000000 ) ) ;
#28585 = CARTESIAN_POINT ( 'NONE',  ( 149.5981739382431783, 2.500000000000000000, -1.703575533167231537 ) ) ;
#28586 = DIRECTION ( 'NONE',  ( 0.000000000000000000, 0.000000000000000000, 1.000000000000000000 ) ) ;
#28587 = EDGE_CURVE ( 'NONE', #13480, #115977, #8880, .T. ) ;
#28588 = LINE ( 'NONE', #86851, #114852 ) ;
#28589 = EDGE_CURVE ( 'NONE', #16932, #21274, #25601, .T. ) ;
#28590 = DIRECTION ( 'NONE',  ( 0.000000000000000000, 0.000000000000000000, 1.000000000000000000 ) ) ;
#28593 = CONICAL_SURFACE ( 'NONE', #70347, 0.09999999999999982514, 0.003490658503988666988 ) ;
#28592 = FACE_OUTER_BOUND ( 'NONE', #111102, .T. ) ;
#28591 = AXIS2_PLACEMENT_3D ( 'NONE', #93019, #54368, #23622 ) ;
#28594 = DIRECTION ( 'NONE',  ( 0.000000000000000000, -0.000000000000000000, -1.000000000000000000 ) ) ;
#28595 = DIRECTION ( 'NONE',  ( 0.000000000000000000, 0.000000000000000000, -1.000000000000000000 ) ) ;
#28596 = LINE ( 'NONE', #48228, #127923 ) ;
#28597 = EDGE_CURVE ( 'NONE', #79180, #103166, #113348, .T. ) ;
#28598 = EDGE_CURVE ( 'NONE', #19791, #76524, #14997, .T. ) ;
#28599 = CARTESIAN_POINT ( 'NONE',  ( -15.59999999999998010, 2.500000000000000000, 0.3464101615137759604 ) ) ;
#28601 = AXIS2_PLACEMENT_3D ( 'NONE', #18336, #109297, #19642 ) ;
#28600 = VECTOR ( 'NONE', #733, 1000.000000000000000 ) ;
#28602 = EDGE_CURVE ( 'NONE', #17818, #100677, #33944, .T. ) ;
#28603 = VECTOR ( 'NONE', #43496, 1000.000000000000000 ) ;
#28604 = ADVANCED_FACE ( 'NONE', ( #116438 ), #50661, .T. ) ;
#28605 = VERTEX_POINT ( 'NONE', #37261 ) ;
#28606 = FACE_OUTER_BOUND ( 'NONE', #100642, .T. ) ;
#28607 = EDGE_CURVE ( 'NONE', #59496, #65382, #98770, .T. ) ;
#28608 = CARTESIAN_POINT ( 'NONE',  ( -12.09999999999999609, 12.50000000000000000, 1.734723475976807094E-15 ) ) ;
#28609 = DIRECTION ( 'NONE',  ( -0.000000000000000000, 1.000000000000000000, -0.000000000000000000 ) ) ;
#28610 = DIRECTION ( 'NONE',  ( 0.000000000000000000, 1.000000000000000000, 0.000000000000000000 ) ) ;
#28611 = DIRECTION ( 'NONE',  ( -0.000000000000000000, 1.000000000000000000, -0.000000000000000000 ) ) ;
#28612 = EDGE_CURVE ( 'NONE', #67778, #28988, #10921, .T. ) ;
#28613 = EDGE_LOOP ( 'NONE', ( #103172, #86716 ) ) ;
#28614 = CARTESIAN_POINT ( 'NONE',  ( -9.800000000000004263, 2.500000000000000000, 4.083716857408420609 ) ) ;
#28615 = DIRECTION ( 'NONE',  ( -0.000000000000000000, 1.000000000000000000, -0.000000000000000000 ) ) ;
#28617 = ORIENTED_EDGE ( 'NONE', *, *, #78517, .F. ) ;
#28616 = DIRECTION ( 'NONE',  ( 0.000000000000000000, -0.9999939076577903929, 0.003490651415223739937 ) ) ;
#28618 = AXIS2_PLACEMENT_3D ( 'NONE', #99863, #38374, #118203 ) ;
#28619 = AXIS2_PLACEMENT_3D ( 'NONE', #17725, #34834, #24986 ) ;
#28620 = EDGE_LOOP ( 'NONE', ( #5390, #93627 ) ) ;
#28621 = AXIS2_PLACEMENT_3D ( 'NONE', #66347, #95817, #45439 ) ;
#28622 = CARTESIAN_POINT ( 'NONE',  ( 0.4499999999999573785, 12.50000000000000000, -6.560283801567339701 ) ) ;
#28623 = CIRCLE ( 'NONE', #68320, 0.06509327318403745899 ) ;
#28624 = ORIENTED_EDGE ( 'NONE', *, *, #103970, .F. ) ;
#28625 = ORIENTED_EDGE ( 'NONE', *, *, #122340, .F. ) ;
#28626 = EDGE_LOOP ( 'NONE', ( #17498, #63702, #87939, #75727 ) ) ;
#28627 = CARTESIAN_POINT ( 'NONE',  ( 8.349999999999923261, 2.500000000000000000, 2.065063509461097624 ) ) ;
#28628 = AXIS2_PLACEMENT_3D ( 'NONE', #129479, #30623, #20144 ) ;
#28629 = CARTESIAN_POINT ( 'NONE',  ( 3.099999999999944134, 12.50000000000000000, 4.741630453620009789 ) ) ;
#28630 = CARTESIAN_POINT ( 'NONE',  ( -8.749999999999975131, 12.50000000000000000, -2.230156782645139391 ) ) ;
#28631 = AXIS2_PLACEMENT_3D ( 'NONE', #79700, #41096, #110446 ) ;
#28632 = DIRECTION ( 'NONE',  ( 0.000000000000000000, 0.000000000000000000, -1.000000000000000000 ) ) ;
#28633 = ORIENTED_EDGE ( 'NONE', *, *, #7323, .F. ) ;
#28634 = CONICAL_SURFACE ( 'NONE', #124768, 0.09999999999999982514, 0.003490658503988666988 ) ;
#28635 = DIRECTION ( 'NONE',  ( 0.000000000000000000, -0.000000000000000000, 1.000000000000000000 ) ) ;
#28636 = ORIENTED_EDGE ( 'NONE', *, *, #65318, .F. ) ;
#28637 = FACE_OUTER_BOUND ( 'NONE', #107858, .T. ) ;
#28638 = CARTESIAN_POINT ( 'NONE',  ( 16.68526679983500571, -0.4774970013481819042, -5.954360761643378019 ) ) ;
#28639 = CARTESIAN_POINT ( 'NONE',  ( 20.69433222467986511, 2.585316282074592298, 4.139109617386874440 ) ) ;
#28640 = CARTESIAN_POINT ( 'NONE',  ( -2.500000000000031086, 12.50000000000000000, 3.702399969078682407 ) ) ;
#28641 = AXIS2_PLACEMENT_3D ( 'NONE', #122409, #71346, #30818 ) ;
#28642 = DIRECTION ( 'NONE',  ( 0.000000000000000000, 0.000000000000000000, -1.000000000000000000 ) ) ;
#28643 = AXIS2_PLACEMENT_3D ( 'NONE', #55056, #84514, #34788 ) ;
#28644 = VERTEX_POINT ( 'NONE', #117074 ) ;
#28645 = EDGE_CURVE ( 'NONE', #76002, #18774, #42356, .T. ) ;
#28647 = AXIS2_PLACEMENT_3D ( 'NONE', #64103, #124318, #86307 ) ;
#28646 = AXIS2_PLACEMENT_3D ( 'NONE', #128045, #18079, #18731 ) ;
#28648 = ORIENTED_EDGE ( 'NONE', *, *, #128049, .T. ) ;
#28649 = ORIENTED_EDGE ( 'NONE', *, *, #59533, .T. ) ;
#28651 = ADVANCED_FACE ( 'NONE', ( #35326 ), #69523, .T. ) ;
#28650 = VERTEX_POINT ( 'NONE', #124984 ) ;
#28652 = ORIENTED_EDGE ( 'NONE', *, *, #119586, .T. ) ;
#28653 = DIRECTION ( 'NONE',  ( -0.000000000000000000, 1.000000000000000000, -0.000000000000000000 ) ) ;
#28654 = CARTESIAN_POINT ( 'NONE',  ( -8.950000000000006395, 2.500000000000000000, 6.941600689897073018 ) ) ;
#28655 = CARTESIAN_POINT ( 'NONE',  ( -7.900000000000014566, 2.500000000000000000, -0.6928203230275541413 ) ) ;
#28656 = FACE_BOUND ( 'NONE', #31140, .T. ) ;
#28657 = CARTESIAN_POINT ( 'NONE',  ( -12.49999999999999289, 12.50000000000000000, -5.022947341949751454 ) ) ;
#28658 = DIRECTION ( 'NONE',  ( 0.000000000000000000, 0.000000000000000000, 1.000000000000000000 ) ) ;
#28659 = CARTESIAN_POINT ( 'NONE',  ( 10.64999999999990976, 2.500000000000000000, 2.511473670974873507 ) ) ;
#28660 = FACE_OUTER_BOUND ( 'NONE', #92443, .T. ) ;
#28661 = CARTESIAN_POINT ( 'NONE',  ( 184.9635416670080588, -4.367472073101520635, 7.564683531249999149 ) ) ;
#28662 = FACE_OUTER_BOUND ( 'NONE', #117299, .T. ) ;
#28663 = AXIS2_PLACEMENT_3D ( 'NONE', #66516, #106451, #9551 ) ;
#28664 = CARTESIAN_POINT ( 'NONE',  ( -5.850000000000021849, 2.500000000000000000, -5.902370205355750521 ) ) ;
#28665 = FACE_OUTER_BOUND ( 'NONE', #66934, .T. ) ;
#28666 = ORIENTED_EDGE ( 'NONE', *, *, #97314, .F. ) ;
#28667 = ORIENTED_EDGE ( 'NONE', *, *, #53376, .T. ) ;
#28668 = ORIENTED_EDGE ( 'NONE', *, *, #79452, .F. ) ;
#28669 = EDGE_LOOP ( 'NONE', ( #33444, #33858, #76679, #120271 ) ) ;
#28670 = DIRECTION ( 'NONE',  ( 0.000000000000000000, 0.000000000000000000, -1.000000000000000000 ) ) ;
#28671 = CARTESIAN_POINT ( 'NONE',  ( -8.550000000000013145, 2.500000000000000000, 2.511473670974873507 ) ) ;
#28672 = FACE_BOUND ( 'NONE', #6641, .T. ) ;
#28673 = CARTESIAN_POINT ( 'NONE',  ( 12.49999999999993960, 2.500000000000000000, 4.230127018922196669 ) ) ;
#28674 = CONICAL_SURFACE ( 'NONE', #97620, 0.1000000000000002554, 0.003490658503988666988 ) ;
#28675 = AXIS2_PLACEMENT_3D ( 'NONE', #83038, #94126, #122951 ) ;
#28676 = VERTEX_POINT ( 'NONE', #109195 ) ;
#28677 = DIRECTION ( 'NONE',  ( 0.000000000000000000, -0.000000000000000000, 1.000000000000000000 ) ) ;
#28678 = CARTESIAN_POINT ( 'NONE',  ( 9.399999999999915090, 2.500000000000000000, 4.776537180435972196 ) ) ;
#28679 = DIRECTION ( 'NONE',  ( 0.000000000000000000, 0.000000000000000000, 1.000000000000000000 ) ) ;
#28680 = LINE ( 'NONE', #70523, #43221 ) ;
#28681 = ORIENTED_EDGE ( 'NONE', *, *, #62605, .F. ) ;
#28682 = DIRECTION ( 'NONE',  ( 0.000000000000000000, 0.000000000000000000, -1.000000000000000000 ) ) ;
#28684 = VECTOR ( 'NONE', #1870, 1000.000000000000000 ) ;
#28683 = VECTOR ( 'NONE', #71274, 1000.000000000000000 ) ;
#28685 = ADVANCED_FACE ( 'NONE', ( #109864 ), #79912, .T. ) ;
#28686 = ORIENTED_EDGE ( 'NONE', *, *, #26729, .T. ) ;
#28687 = ORIENTED_EDGE ( 'NONE', *, *, #29076, .T. ) ;
#28688 = DIRECTION ( 'NONE',  ( -0.000000000000000000, 1.000000000000000000, -0.000000000000000000 ) ) ;
#28689 = DIRECTION ( 'NONE',  ( 0.000000000000000000, 1.000000000000000000, 0.000000000000000000 ) ) ;
#28690 = VERTEX_POINT ( 'NONE', #77802 ) ;
#28692 = CONICAL_SURFACE ( 'NONE', #83077, 0.1000000000000002554, 0.003490658503988666988 ) ;
#28691 = CIRCLE ( 'NONE', #126887, 0.1000000000000002554 ) ;
#28693 = VECTOR ( 'NONE', #65534, 1000.000000000000000 ) ;
#28694 = DIRECTION ( 'NONE',  ( 0.000000000000000000, 0.000000000000000000, -1.000000000000000000 ) ) ;
#28695 = DIRECTION ( 'NONE',  ( -0.000000000000000000, 1.000000000000000000, -0.000000000000000000 ) ) ;
#28696 = EDGE_LOOP ( 'NONE', ( #127600, #36920 ) ) ;
#28697 = CARTESIAN_POINT ( 'NONE',  ( 9.349999999999916156, 12.50000000000000000, 6.841600689897072485 ) ) ;
#28698 = ORIENTED_EDGE ( 'NONE', *, *, #77817, .F. ) ;
#28699 = EDGE_CURVE ( 'NONE', #29893, #81561, #86240, .T. ) ;
#28700 = ADVANCED_FACE ( 'NONE', ( #110495 ), #86143, .T. ) ;
#28701 = DIRECTION ( 'NONE',  ( -0.000000000000000000, -1.000000000000000000, -0.000000000000000000 ) ) ;
#28702 = ORIENTED_EDGE ( 'NONE', *, *, #124157, .F. ) ;
#28703 = CARTESIAN_POINT ( 'NONE',  ( 186.6145833340161175, 6.668395609140177704, -3.849999999999998312 ) ) ;
#28704 = FACE_BOUND ( 'NONE', #95949, .T. ) ;
#28705 = ORIENTED_EDGE ( 'NONE', *, *, #29806, .F. ) ;
#28706 = CARTESIAN_POINT ( 'NONE',  ( 112.4709740538754943, 7.366778627195011531, -2.262163914407335330 ) ) ;
#28707 = VERTEX_POINT ( 'NONE', #117714 ) ;
#28708 = DIRECTION ( 'NONE',  ( 0.000000000000000000, 0.000000000000000000, -1.000000000000000000 ) ) ;
#28709 = DIRECTION ( 'NONE',  ( 0.000000000000000000, 0.000000000000000000, 1.000000000000000000 ) ) ;
#28710 = DIRECTION ( 'NONE',  ( 0.000000000000000000, 0.000000000000000000, 1.000000000000000000 ) ) ;
#28712 = ADVANCED_FACE ( 'NONE', ( #69934 ), #31889, .T. ) ;
#28711 = CARTESIAN_POINT ( 'NONE',  ( 6.449999999999930012, 2.500000000000000000, -1.818653347947326138 ) ) ;
#28714 = CIRCLE ( 'NONE', #16064, 0.1000000000000000472 ) ;
#28713 = FACE_OUTER_BOUND ( 'NONE', #21622, .T. ) ;
#28715 = ORIENTED_EDGE ( 'NONE', *, *, #120658, .T. ) ;
#28716 = AXIS2_PLACEMENT_3D ( 'NONE', #51883, #32259, #12577 ) ;
#28717 = ORIENTED_EDGE ( 'NONE', *, *, #96807, .T. ) ;
#28718 = ORIENTED_EDGE ( 'NONE', *, *, #64341, .F. ) ;
#28719 = DIRECTION ( 'NONE',  ( 0.000000000000000000, 0.000000000000000000, -1.000000000000000000 ) ) ;
#28720 = AXIS2_PLACEMENT_3D ( 'NONE', #42817, #61140, #2199 ) ;
#28721 = DIRECTION ( 'NONE',  ( -0.000000000000000000, 1.000000000000000000, -0.000000000000000000 ) ) ;
#28722 = DIRECTION ( 'NONE',  ( 0.000000000000000000, 0.000000000000000000, 1.000000000000000000 ) ) ;
#28724 = EDGE_LOOP ( 'NONE', ( #58205, #61746 ) ) ;
#28723 = VERTEX_POINT ( 'NONE', #10363 ) ;
#28725 = ORIENTED_EDGE ( 'NONE', *, *, #112419, .T. ) ;
#28726 = DIRECTION ( 'NONE',  ( -0.000000000000000000, 1.000000000000000000, -0.000000000000000000 ) ) ;
#28727 = VECTOR ( 'NONE', #63128, 1000.000000000000000 ) ;
#28728 = CONICAL_SURFACE ( 'NONE', #93472, 0.1000000000000002554, 0.003490658503988666988 ) ;
#28729 = DIRECTION ( 'NONE',  ( 0.000000000000000000, -0.000000000000000000, 1.000000000000000000 ) ) ;
#28730 = DIRECTION ( 'NONE',  ( 1.000000000000000000, 0.000000000000000000, 0.000000000000000000 ) ) ;
#28731 = PLANE ( 'NONE',  #90816 ) ;
#28732 = DIRECTION ( 'NONE',  ( 0.000000000000000000, 1.000000000000000000, 0.000000000000000000 ) ) ;
#28733 = DIRECTION ( 'NONE',  ( -4.274815082592931898E-19, -0.9999939076577903929, -0.003490651415223739937 ) ) ;
#28734 = CARTESIAN_POINT ( 'NONE',  ( 6.899999999999928413, 2.500000000000000000, 4.083716857408421497 ) ) ;
#28735 = DIRECTION ( 'NONE',  ( -0.000000000000000000, -1.000000000000000000, -0.000000000000000000 ) ) ;
#28736 = CARTESIAN_POINT ( 'NONE',  ( 3.349999999999941913, 2.500000000000000000, 6.495190528383297135 ) ) ;
#28737 = ORIENTED_EDGE ( 'NONE', *, *, #50474, .F. ) ;
#28738 = VERTEX_POINT ( 'NONE', #90192 ) ;
#28739 = EDGE_CURVE ( 'NONE', #13047, #49424, #28077, .T. ) ;
#28740 = CARTESIAN_POINT ( 'NONE',  ( 1.849999999999951017, 12.50000000000000000, -6.148780366869526226 ) ) ;
#28742 = CONICAL_SURFACE ( 'NONE', #106090, 0.09999999999999982514, 0.003490658503988666988 ) ;
#28741 = CIRCLE ( 'NONE', #39228, 0.06509327318403745899 ) ;
#28743 = CARTESIAN_POINT ( 'NONE',  ( -0.6500000000000394351, 2.500000000000000000, 6.741600689897071952 ) ) ;
#28744 = EDGE_LOOP ( 'NONE', ( #70108, #126424, #52314, #28511 ) ) ;
#28745 = EDGE_LOOP ( 'NONE', ( #106457, #77903, #11849, #108449 ) ) ;
#28746 = ADVANCED_FACE ( 'NONE', ( #49022 ), #20189, .T. ) ;
#28747 = CARTESIAN_POINT ( 'NONE',  ( 186.4010416670080588, -4.367472073101519747, 7.564683531249999149 ) ) ;
#28748 = DIRECTION ( 'NONE',  ( 0.000000000000000000, 1.000000000000000000, 0.000000000000000000 ) ) ;
#28749 = DIRECTION ( 'NONE',  ( 0.000000000000000000, 1.000000000000000000, 0.000000000000000000 ) ) ;
#28750 = ADVANCED_FACE ( 'NONE', ( #88256 ), #54851, .T. ) ;
#28751 = DIRECTION ( 'NONE',  ( 0.000000000000000000, 0.000000000000000000, -1.000000000000000000 ) ) ;
#28752 = CARTESIAN_POINT ( 'NONE',  ( -12.89999999999999147, 2.500000000000000000, -4.330127018922198978 ) ) ;
#28753 = LINE ( 'NONE', #37913, #19744 ) ;
#28754 = CARTESIAN_POINT ( 'NONE',  ( -9.400000000000007461, 2.500000000000000000, 4.676537180435972552 ) ) ;
#28755 = EDGE_CURVE ( 'NONE', #13760, #88783, #44403, .T. ) ;
#28756 = EDGE_CURVE ( 'NONE', #34917, #16266, #29731, .T. ) ;
#28757 = EDGE_CURVE ( 'NONE', #16470, #23090, #40205, .T. ) ;
#28758 = CIRCLE ( 'NONE', #118620, 0.09999999999999982514 ) ;
#28759 = EDGE_CURVE ( 'NONE', #127685, #71566, #37889, .T. ) ;
#28760 = DIRECTION ( 'NONE',  ( 0.000000000000000000, 0.000000000000000000, 1.000000000000000000 ) ) ;
#28761 = PRODUCT_DEFINITION_CONTEXT ( 'detailed design', #60581, 'design' ) ;
#28762 = ORIENTED_EDGE ( 'NONE', *, *, #119498, .F. ) ;
#28763 = ADVANCED_FACE ( 'NONE', ( #129527 ), #36087, .T. ) ;
#28764 = EDGE_LOOP ( 'NONE', ( #39334, #103957 ) ) ;
#28765 = ORIENTED_EDGE ( 'NONE', *, *, #35514, .F. ) ;
#28766 = EDGE_LOOP ( 'NONE', ( #65585, #114699 ) ) ;
#28767 = CARTESIAN_POINT ( 'NONE',  ( 3.099999999999945466, 12.50000000000000000, -4.048810130592463530 ) ) ;
#28768 = CARTESIAN_POINT ( 'NONE',  ( 8.349999999999923261, 12.50000000000000000, 1.407149913249508000 ) ) ;
#28769 = ADVANCED_FACE ( 'NONE', ( #128219 ), #38564, .T. ) ;
#28770 = ORIENTED_EDGE ( 'NONE', *, *, #125485, .T. ) ;
#28771 = CIRCLE ( 'NONE', #116572, 0.06509327318403745899 ) ;
#28772 = CARTESIAN_POINT ( 'NONE',  ( 184.5000000000000000, 0.000000000000000000, 0.000000000000000000 ) ) ;
#28774 = DIRECTION ( 'NONE',  ( -0.000000000000000000, -1.000000000000000000, -0.000000000000000000 ) ) ;
#28773 = VECTOR ( 'NONE', #94443, 1000.000000000000000 ) ;
#28775 = DIRECTION ( 'NONE',  ( 0.000000000000000000, 1.000000000000000000, 0.000000000000000000 ) ) ;
#28777 = VERTEX_POINT ( 'NONE', #108566 ) ;
#28776 = DIRECTION ( 'NONE',  ( 0.000000000000000000, 0.000000000000000000, 1.000000000000000000 ) ) ;
#28778 = DIRECTION ( 'NONE',  ( 0.000000000000000000, 1.000000000000000000, 0.000000000000000000 ) ) ;
#28779 = AXIS2_PLACEMENT_3D ( 'NONE', #80317, #433, #8331 ) ;
#28780 = LINE ( 'NONE', #30729, #58279 ) ;
#28781 = ORIENTED_EDGE ( 'NONE', *, *, #52122, .F. ) ;
#28782 = AXIS2_PLACEMENT_3D ( 'NONE', #15159, #66212, #106148 ) ;
#28783 = ORIENTED_EDGE ( 'NONE', *, *, #96532, .F. ) ;
#28784 = ORIENTED_EDGE ( 'NONE', *, *, #10418, .T. ) ;
#28785 = FACE_OUTER_BOUND ( 'NONE', #64148, .T. ) ;
#28786 = CIRCLE ( 'NONE', #80737, 0.06509327318403745899 ) ;
#28787 = DIRECTION ( 'NONE',  ( 0.000000000000000000, 0.000000000000000000, -1.000000000000000000 ) ) ;
#28788 = CIRCLE ( 'NONE', #116503, 0.1000000000000002554 ) ;
#28789 = ORIENTED_EDGE ( 'NONE', *, *, #10381, .T. ) ;
#28790 = AXIS2_PLACEMENT_3D ( 'NONE', #61924, #102476, #71729 ) ;
#28791 = CARTESIAN_POINT ( 'NONE',  ( 9.149999999999916866, 2.500000000000000000, -1.572243186433550211 ) ) ;
#28792 = CARTESIAN_POINT ( 'NONE',  ( -7.950000000000009059, 12.50000000000000000, 6.495190528383297135 ) ) ;
#28793 = DIRECTION ( 'NONE',  ( 0.000000000000000000, 1.000000000000000000, 0.000000000000000000 ) ) ;
#28794 = CARTESIAN_POINT ( 'NONE',  ( 13.14999999999989733, 2.500000000000000000, -1.718653347947325827 ) ) ;
#28795 = EDGE_LOOP ( 'NONE', ( #91325, #61306 ) ) ;
#28796 = CIRCLE ( 'NONE', #14101, 0.06509327318403745899 ) ;
#28797 = DIRECTION ( 'NONE',  ( 0.000000000000000000, 1.000000000000000000, 0.000000000000000000 ) ) ;
#28798 = ADVANCED_FACE ( 'NONE', ( #98730 ), #128029, .T. ) ;
#28799 = AXIS2_PLACEMENT_3D ( 'NONE', #58959, #82313, #112412 ) ;
#28800 = ORIENTED_EDGE ( 'NONE', *, *, #128811, .T. ) ;
#28801 = EDGE_LOOP ( 'NONE', ( #121129, #30949, #56469, #29171 ) ) ;
#28802 = CARTESIAN_POINT ( 'NONE',  ( 7.949999999999922018, 2.500000000000000000, 6.495190528383297135 ) ) ;
#28803 = DIRECTION ( 'NONE',  ( 0.000000000000000000, 1.000000000000000000, 0.000000000000000000 ) ) ;
#28804 = FACE_BOUND ( 'NONE', #91141, .T. ) ;
#28805 = CIRCLE ( 'NONE', #20394, 0.1000000000000002554 ) ;
#28806 = DIRECTION ( 'NONE',  ( 0.000000000000000000, 0.000000000000000000, -1.000000000000000000 ) ) ;
#28807 = CARTESIAN_POINT ( 'NONE',  ( -2.900000000000029221, 12.50000000000000000, -4.330127018922201643 ) ) ;
#28808 = CIRCLE ( 'NONE', #68501, 0.09999999999999999167 ) ;
#28809 = CARTESIAN_POINT ( 'NONE',  ( 2.049999999999950084, 12.50000000000000000, -6.560283801567339701 ) ) ;
#28810 = EDGE_CURVE ( 'NONE', #16266, #34917, #90360, .T. ) ;
#28811 = AXIS2_PLACEMENT_3D ( 'NONE', #112822, #51341, #924 ) ;
#28812 = ORIENTED_EDGE ( 'NONE', *, *, #78583, .T. ) ;
#28813 = DIRECTION ( 'NONE',  ( 0.000000000000000000, 1.000000000000000000, 0.000000000000000000 ) ) ;
#28814 = CARTESIAN_POINT ( 'NONE',  ( -4.076600168545496672E-14, 12.50000000000000000, -5.022947341949754119 ) ) ;
#28816 = CARTESIAN_POINT ( 'NONE',  ( 5.849999999999935696, 2.500000000000000000, -6.495190528383302464 ) ) ;
#28815 = CIRCLE ( 'NONE', #101971, 0.06509327318403745899 ) ;
#28818 = DIRECTION ( 'NONE',  ( 0.000000000000000000, 0.000000000000000000, 1.000000000000000000 ) ) ;
#28817 = CIRCLE ( 'NONE', #101972, 0.06509327318403745899 ) ;
#28819 = ORIENTED_EDGE ( 'NONE', *, *, #114950, .T. ) ;
#28820 = CARTESIAN_POINT ( 'NONE',  ( -2.700000000000030820, 12.50000000000000000, -3.983716857408426293 ) ) ;
#28821 = AXIS2_PLACEMENT_3D ( 'NONE', #69333, #70005, #41844 ) ;
#28822 = DIRECTION ( 'NONE',  ( 0.000000000000000000, 0.000000000000000000, 1.000000000000000000 ) ) ;
#28823 = EDGE_LOOP ( 'NONE', ( #66001, #21890 ) ) ;
#28824 = ORIENTED_EDGE ( 'NONE', *, *, #799, .F. ) ;
#28825 = CARTESIAN_POINT ( 'NONE',  ( 9.149999999999915090, 2.500000000000000000, -2.265063509461101798 ) ) ;
#28826 = AXIS2_PLACEMENT_3D ( 'NONE', #15494, #115628, #103896 ) ;
#28827 = DIRECTION ( 'NONE',  ( -4.274815082592931898E-19, -0.9999939076577903929, -0.003490651415223739937 ) ) ;
#28828 = FACE_BOUND ( 'NONE', #85215, .T. ) ;
#28829 = CARTESIAN_POINT ( 'NONE',  ( 8.349999999999923261, 12.50000000000000000, 1.472243186433545459 ) ) ;
#28831 = CIRCLE ( 'NONE', #101989, 0.06509327318403745899 ) ;
#28830 = CIRCLE ( 'NONE', #39318, 0.1000000000000002554 ) ;
#28832 = ORIENTED_EDGE ( 'NONE', *, *, #55932, .T. ) ;
#28833 = DIRECTION ( 'NONE',  ( 0.000000000000000000, 1.000000000000000000, 0.000000000000000000 ) ) ;
#28834 = ORIENTED_EDGE ( 'NONE', *, *, #21191, .F. ) ;
#28835 = ORIENTED_EDGE ( 'NONE', *, *, #126582, .F. ) ;
#28836 = DIRECTION ( 'NONE',  ( -0.000000000000000000, -1.000000000000000000, -0.000000000000000000 ) ) ;
#28837 = CARTESIAN_POINT ( 'NONE',  ( 185.5833333333333144, -6.668395609140180369, 3.849999999999994760 ) ) ;
#28838 = ORIENTED_EDGE ( 'NONE', *, *, #57612, .T. ) ;
#28839 = DIRECTION ( 'NONE',  ( 0.000000000000000000, 0.000000000000000000, -1.000000000000000000 ) ) ;
#28840 = DIRECTION ( 'NONE',  ( -0.000000000000000000, -1.000000000000000000, -0.000000000000000000 ) ) ;
#28841 = EDGE_CURVE ( 'NONE', #36170, #100170, #565, .T. ) ;
#28842 = FACE_OUTER_BOUND ( 'NONE', #44177, .T. ) ;
#28843 = CARTESIAN_POINT ( 'NONE',  ( 194.5000000000000000, 0.000000000000000000, 0.000000000000000000 ) ) ;
#28844 = ADVANCED_FACE ( 'NONE', ( #1187 ), #100911, .T. ) ;
#28845 = ORIENTED_EDGE ( 'NONE', *, *, #111728, .F. ) ;
#28846 = SURFACE_SIDE_STYLE ('',( #17709 ) ) ;
#28847 = CARTESIAN_POINT ( 'NONE',  ( 6.449999999999930012, 2.500000000000000000, 1.918653347947321564 ) ) ;
#28848 = CARTESIAN_POINT ( 'NONE',  ( 184.5729166673494888, 4.445597072760062218, -7.700000000000102318 ) ) ;
#28849 = CARTESIAN_POINT ( 'NONE',  ( 2.299999999999948752, 2.500000000000000000, -4.083716857408426826 ) ) ;
#28850 = ORIENTED_EDGE ( 'NONE', *, *, #44877, .T. ) ;
#28852 = EDGE_CURVE ( 'NONE', #92706, #64742, #98861, .T. ) ;
#28851 = AXIS2_PLACEMENT_3D ( 'NONE', #35147, #44955, #56039 ) ;
#28853 = ORIENTED_EDGE ( 'NONE', *, *, #125628, .F. ) ;
#28854 = EDGE_CURVE ( 'NONE', #84759, #93988, #8973, .T. ) ;
#28855 = CARTESIAN_POINT ( 'NONE',  ( -8.750000000000005329, 2.500000000000000000, 5.802370205355744659 ) ) ;
#28856 = EDGE_LOOP ( 'NONE', ( #98669, #71943 ) ) ;
#28857 = DIRECTION ( 'NONE',  ( 0.000000000000000000, 0.000000000000000000, 1.000000000000000000 ) ) ;
#28858 = CARTESIAN_POINT ( 'NONE',  ( 5.849999999999935696, 2.500000000000000000, -6.495190528383302464 ) ) ;
#28859 = AXIS2_PLACEMENT_3D ( 'NONE', #114672, #96315, #86500 ) ;
#28860 = DIRECTION ( 'NONE',  ( 0.000000000000000000, 0.000000000000000000, -1.000000000000000000 ) ) ;
#28861 = AXIS2_PLACEMENT_3D ( 'NONE', #119247, #38788, #19770 ) ;
#28862 = DIRECTION ( 'NONE',  ( 0.000000000000000000, 1.000000000000000000, 0.000000000000000000 ) ) ;
#28863 = ORIENTED_EDGE ( 'NONE', *, *, #105256, .T. ) ;
#28864 = ADVANCED_FACE ( 'NONE', ( #113065 ), #122905, .T. ) ;
#28865 = DIRECTION ( 'NONE',  ( 0.000000000000000000, -0.9999939076577903929, 0.003490651415223739937 ) ) ;
#28866 = DIRECTION ( 'NONE',  ( -0.000000000000000000, -1.000000000000000000, -0.000000000000000000 ) ) ;
#28867 = CARTESIAN_POINT ( 'NONE',  ( 81.97672699151137010, 3.779183617727026601, -6.223416210580854369 ) ) ;
#28868 = CARTESIAN_POINT ( 'NONE',  ( 185.5260416670080588, -6.551208109652273848, -3.782341765625003571 ) ) ;
#28869 = DIRECTION ( 'NONE',  ( 0.000000000000000000, -0.9999939076577903929, 0.003490651415223739937 ) ) ;
#28870 = EDGE_CURVE ( 'NONE', #60531, #59400, #52232, .T. ) ;
#28871 = LINE ( 'NONE', #7267, #122655 ) ;
#28872 = VECTOR ( 'NONE', #48055, 1000.000000000000000 ) ;
#28873 = VERTEX_POINT ( 'NONE', #52872 ) ;
#28875 = ORIENTED_EDGE ( 'NONE', *, *, #50072, .F. ) ;
#28874 = CIRCLE ( 'NONE', #47744, 0.09999999999999999167 ) ;
#28876 = PLANE ( 'NONE',  #108039 ) ;
#28877 = VERTEX_POINT ( 'NONE', #1822 ) ;
#28878 = CARTESIAN_POINT ( 'NONE',  ( 187.5000000000000000, 9.429780353434619030E-16, -7.700000000000000178 ) ) ;
#28880 = ORIENTED_EDGE ( 'NONE', *, *, #97849, .T. ) ;
#28879 = ORIENTED_EDGE ( 'NONE', *, *, #115159, .T. ) ;
#28881 = EDGE_LOOP ( 'NONE', ( #119986, #129128, #126555, #119816 ) ) ;
#28882 = DIRECTION ( 'NONE',  ( -0.000000000000000000, -1.000000000000000000, -0.000000000000000000 ) ) ;
#28884 = FACE_OUTER_BOUND ( 'NONE', #18578, .T. ) ;
#28883 = VECTOR ( 'NONE', #56353, 1000.000000000000000 ) ;
#28885 = CARTESIAN_POINT ( 'NONE',  ( -3.550000000000030909, 12.50000000000000000, -6.906693963081115939 ) ) ;
#28886 = DIRECTION ( 'NONE',  ( 0.000000000000000000, 1.000000000000000000, 0.000000000000000000 ) ) ;
#28887 = DIRECTION ( 'NONE',  ( 0.000000000000000000, 0.000000000000000000, 1.000000000000000000 ) ) ;
#28888 = CARTESIAN_POINT ( 'NONE',  ( -7.700000000000010836, 12.50000000000000000, 3.918623584224383727 ) ) ;
#28889 = CIRCLE ( 'NONE', #10000, 2.000000000000000000 ) ;
#28890 = CARTESIAN_POINT ( 'NONE',  ( 2.299999999999946976, 2.500000000000000000, 4.576537180435972019 ) ) ;
#28891 = CARTESIAN_POINT ( 'NONE',  ( -6.050000000000022027, 12.50000000000000000, -1.818653347947326138 ) ) ;
#28892 = ORIENTED_EDGE ( 'NONE', *, *, #71468, .F. ) ;
#28893 = VECTOR ( 'NONE', #100902, 1000.000000000000000 ) ;
#28894 = ORIENTED_EDGE ( 'NONE', *, *, #89940, .F. ) ;
#28895 = EDGE_LOOP ( 'NONE', ( #56588, #61210 ) ) ;
#28896 = AXIS2_PLACEMENT_3D ( 'NONE', #80064, #118044, #9395 ) ;
#28897 = DIRECTION ( 'NONE',  ( 1.000000000000000000, -0.000000000000000000, -0.000000000000000000 ) ) ;
#28898 = VERTEX_POINT ( 'NONE', #112445 ) ;
#28899 = ORIENTED_EDGE ( 'NONE', *, *, #23201, .T. ) ;
#28900 = CARTESIAN_POINT ( 'NONE',  ( -13.74999999999998757, 2.500000000000000000, -2.757883832488651876 ) ) ;
#28901 = CIRCLE ( 'NONE', #106165, 0.06509327318403745899 ) ;
#28902 = AXIS2_PLACEMENT_3D ( 'NONE', #43865, #53030, #102126 ) ;
#28903 = EDGE_CURVE ( 'NONE', #62546, #115890, #119699, .T. ) ;
#28905 = CONICAL_SURFACE ( 'NONE', #18513, 0.1000000000000002554, 0.003490658503988666988 ) ;
#28904 = DIRECTION ( 'NONE',  ( 0.000000000000000000, 0.000000000000000000, -1.000000000000000000 ) ) ;
#28906 = DIRECTION ( 'NONE',  ( 0.000000000000000000, 1.000000000000000000, 0.000000000000000000 ) ) ;
#28907 = CARTESIAN_POINT ( 'NONE',  ( -11.64999999999999858, 2.500000000000000000, -5.802370205355746435 ) ) ;
#28908 = EDGE_CURVE ( 'NONE', #125626, #117945, #40305, .T. ) ;
#28909 = CARTESIAN_POINT ( 'NONE',  ( -1.650000000000034772, 12.50000000000000000, 2.165063509461097713 ) ) ;
#28910 = VERTEX_POINT ( 'NONE', #100661 ) ;
#28911 = ADVANCED_FACE ( 'NONE', ( #31951 ), #63272, .T. ) ;
#28912 = AXIS2_PLACEMENT_3D ( 'NONE', #13867, #32255, #53798 ) ;
#28913 = ADVANCED_FACE ( 'NONE', ( #41137 ), #92616, .T. ) ;
#28914 = EDGE_CURVE ( 'NONE', #109859, #94650, #121849, .T. ) ;
#28915 = ORIENTED_EDGE ( 'NONE', *, *, #21180, .T. ) ;
#28916 = LINE ( 'NONE', #27590, #30010 ) ;
#28917 = EDGE_LOOP ( 'NONE', ( #25837, #124605 ) ) ;
#28918 = CARTESIAN_POINT ( 'NONE',  ( 6.049999999999934097, 2.500000000000000000, -2.511473670974877948 ) ) ;
#28919 = ADVANCED_FACE ( 'NONE', ( #2456 ), #54956, .T. ) ;
#28920 = ORIENTED_EDGE ( 'NONE', *, *, #94496, .F. ) ;
#28921 = CONICAL_SURFACE ( 'NONE', #104123, 0.1000000000000002554, 0.003490658503988666988 ) ;
#28922 = ORIENTED_EDGE ( 'NONE', *, *, #91843, .F. ) ;
#28923 = DIRECTION ( 'NONE',  ( -0.000000000000000000, -1.000000000000000000, -0.000000000000000000 ) ) ;
#28924 = DIRECTION ( 'NONE',  ( 0.000000000000000000, 0.000000000000000000, 1.000000000000000000 ) ) ;
#28925 = EDGE_CURVE ( 'NONE', #112846, #32323, #4758, .T. ) ;
#28927 = ADVANCED_FACE ( 'NONE', ( #42417 ), #51595, .T. ) ;
#28926 = AXIS2_PLACEMENT_3D ( 'NONE', #81065, #87794, #31327 ) ;
#28928 = LINE ( 'NONE', #68832, #59187 ) ;
#28929 = DIRECTION ( 'NONE',  ( 0.000000000000000000, 0.000000000000000000, 1.000000000000000000 ) ) ;
#28930 = CARTESIAN_POINT ( 'NONE',  ( -5.400000000000023448, 2.500000000000000000, -5.022947341949754119 ) ) ;
#28931 = VERTEX_POINT ( 'NONE', #61418 ) ;
#28932 = DIRECTION ( 'NONE',  ( 0.000000000000000000, -0.9999939076577903929, 0.003490651415223739937 ) ) ;
#28933 = CARTESIAN_POINT ( 'NONE',  ( -10.65000000000000213, 12.50000000000000000, 2.446380397790835826 ) ) ;
#28934 = PLANE ( 'NONE',  #83381 ) ;
#28935 = DIRECTION ( 'NONE',  ( -0.000000000000000000, 1.000000000000000000, -0.000000000000000000 ) ) ;
#28936 = CARTESIAN_POINT ( 'NONE',  ( -1.650000000000034328, 12.50000000000000000, -6.495190528383302464 ) ) ;
#28937 = ORIENTED_EDGE ( 'NONE', *, *, #31268, .F. ) ;
#28938 = ORIENTED_EDGE ( 'NONE', *, *, #52507, .T. ) ;
#28939 = CONICAL_SURFACE ( 'NONE', #127233, 0.09999999999999999167, 0.003490658503988666988 ) ;
#28940 = CARTESIAN_POINT ( 'NONE',  ( -2.900000000000029221, 2.500000000000000000, -0.1000000000000022815 ) ) ;
#28941 = EDGE_CURVE ( 'NONE', #58229, #126385, #72522, .T. ) ;
#28942 = VERTEX_POINT ( 'NONE', #129298 ) ;
#28943 = FACE_OUTER_BOUND ( 'NONE', #32176, .T. ) ;
#28944 = CARTESIAN_POINT ( 'NONE',  ( 6.899999999999928413, 2.500000000000000000, -4.676537180435977881 ) ) ;
#28945 = AXIS2_PLACEMENT_3D ( 'NONE', #110067, #79331, #38772 ) ;
#28946 = AXIS2_PLACEMENT_3D ( 'NONE', #54639, #84764, #124692 ) ;
#28947 = AXIS2_PLACEMENT_3D ( 'NONE', #65388, #75217, #85028 ) ;
#28948 = AXIS2_PLACEMENT_3D ( 'NONE', #72029, #121111, #72669 ) ;
#28949 = ORIENTED_EDGE ( 'NONE', *, *, #117304, .F. ) ;
#28950 = CARTESIAN_POINT ( 'NONE',  ( 186.6666666666666856, -6.668395609140176816, -3.850000000000003642 ) ) ;
#28951 = LINE ( 'NONE', #86559, #11803 ) ;
#28952 = CARTESIAN_POINT ( 'NONE',  ( 187.4218750003414016, 0.000000000000000000, 7.564683531250000925 ) ) ;
#28953 = CARTESIAN_POINT ( 'NONE',  ( -9.350000000000006750, 2.500000000000000000, 2.511473670974873507 ) ) ;
#28954 = ORIENTED_EDGE ( 'NONE', *, *, #93326, .F. ) ;
#28955 = AXIS2_PLACEMENT_3D ( 'NONE', #7274, #107423, #38039 ) ;
#28956 = AXIS2_PLACEMENT_3D ( 'NONE', #113226, #85062, #92967 ) ;
#28957 = CIRCLE ( 'NONE', #35222, 0.06509327318403745899 ) ;
#28958 = CARTESIAN_POINT ( 'NONE',  ( 0.8499999999999553468, 2.500000000000000000, -2.065063509461102065 ) ) ;
#28959 = ORIENTED_EDGE ( 'NONE', *, *, #83125, .T. ) ;
#28960 = FACE_OUTER_BOUND ( 'NONE', #5665, .T. ) ;
#28961 = CARTESIAN_POINT ( 'NONE',  ( -0.4000000000000392131, 12.50000000000000000, -5.022947341949754119 ) ) ;
#28962 = CONICAL_SURFACE ( 'NONE', #102113, 0.1000000000000002554, 0.003490658503988666988 ) ;
#28963 = CARTESIAN_POINT ( 'NONE',  ( -8.100000000000013856, 2.500000000000000000, -4.676537180435977881 ) ) ;
#28964 = EDGE_CURVE ( 'NONE', #117945, #125626, #84192, .T. ) ;
#28965 = AXIS2_PLACEMENT_3D ( 'NONE', #106663, #6496, #55638 ) ;
#28966 = ORIENTED_EDGE ( 'NONE', *, *, #103566, .F. ) ;
#28967 = CARTESIAN_POINT ( 'NONE',  ( 0.8499999999999553468, 2.500000000000000000, 2.165063509461097713 ) ) ;
#28968 = ORIENTED_EDGE ( 'NONE', *, *, #62044, .T. ) ;
#28969 = DIRECTION ( 'NONE',  ( 0.000000000000000000, -0.000000000000000000, 1.000000000000000000 ) ) ;
#28970 = DIRECTION ( 'NONE',  ( 1.000000000000000000, -0.000000000000000000, -0.000000000000000000 ) ) ;
#28971 = DIRECTION ( 'NONE',  ( 0.000000000000000000, -0.9999939076577903929, 0.003490651415223739937 ) ) ;
#28972 = ORIENTED_EDGE ( 'NONE', *, *, #96587, .T. ) ;
#28973 = AXIS2_PLACEMENT_3D ( 'NONE', #58162, #47690, #28045 ) ;
#28974 = DIRECTION ( 'NONE',  ( 0.000000000000000000, 0.000000000000000000, -1.000000000000000000 ) ) ;
#28975 = CARTESIAN_POINT ( 'NONE',  ( 3.749999999999940492, 12.50000000000000000, 5.867463478539781896 ) ) ;
#28976 = AXIS2_PLACEMENT_3D ( 'NONE', #47364, #108204, #117348 ) ;
#28977 = AXIS2_PLACEMENT_3D ( 'NONE', #36171, #85259, #4105 ) ;
#28978 = ORIENTED_EDGE ( 'NONE', *, *, #35816, .F. ) ;
#28979 = DIRECTION ( 'NONE',  ( 0.000000000000000000, 0.000000000000000000, -1.000000000000000000 ) ) ;
#28980 = EDGE_LOOP ( 'NONE', ( #110484, #126893, #94062, #62642 ) ) ;
#28981 = DIRECTION ( 'NONE',  ( 0.000000000000000000, 1.000000000000000000, 0.000000000000000000 ) ) ;
#28982 = AXIS2_PLACEMENT_3D ( 'NONE', #18907, #26813, #58850 ) ;
#28983 = VERTEX_POINT ( 'NONE', #108959 ) ;
#28984 = STYLED_ITEM ( 'NONE', ( #57028 ), #78940 ) ;
#28985 = DIRECTION ( 'NONE',  ( 0.000000000000000000, 0.000000000000000000, 1.000000000000000000 ) ) ;
#28986 = LINE ( 'NONE', #96405, #14539 ) ;
#28987 = ORIENTED_EDGE ( 'NONE', *, *, #75621, .F. ) ;
#28988 = VERTEX_POINT ( 'NONE', #120102 ) ;
#28989 = DIRECTION ( 'NONE',  ( 0.000000000000000000, 1.000000000000000000, 0.000000000000000000 ) ) ;
#28990 = CARTESIAN_POINT ( 'NONE',  ( -5.600000000000020073, 12.50000000000000000, -0.4115034346978156399 ) ) ;
#28991 = CIRCLE ( 'NONE', #41527, 0.06509327318403745899 ) ;
#28992 = ORIENTED_EDGE ( 'NONE', *, *, #100030, .F. ) ;
#28993 = DIRECTION ( 'NONE',  ( 0.000000000000000000, 0.000000000000000000, 1.000000000000000000 ) ) ;
#28994 = CARTESIAN_POINT ( 'NONE',  ( 186.9427083336747160, -6.551208109652278289, 3.782341765624995134 ) ) ;
#28995 = CARTESIAN_POINT ( 'NONE',  ( -9.999999999999969802, 12.50000000000000000, 4.265033745738159077 ) ) ;
#28996 = CARTESIAN_POINT ( 'NONE',  ( 104.2436697997757165, 8.047302484776873044, -3.315374049100932474 ) ) ;
#28997 = FACE_OUTER_BOUND ( 'NONE', #62493, .T. ) ;
#28998 = CARTESIAN_POINT ( 'NONE',  ( -14.39999999999998614, 12.50000000000000000, 0.4115034346978132529 ) ) ;
#28999 = CARTESIAN_POINT ( 'NONE',  ( -11.44999999999999751, 12.50000000000000000, 1.753560074763284016 ) ) ;
#29000 = AXIS2_PLACEMENT_3D ( 'NONE', #111408, #125734, #45920 ) ;
#29001 = EDGE_CURVE ( 'NONE', #22580, #13178, #48716, .T. ) ;
#29002 = ORIENTED_EDGE ( 'NONE', *, *, #117787, .T. ) ;
#29003 = ORIENTED_EDGE ( 'NONE', *, *, #53114, .F. ) ;
#29005 = EDGE_LOOP ( 'NONE', ( #123437, #74310 ) ) ;
#29004 = CIRCLE ( 'NONE', #125423, 0.1000000000000002554 ) ;
#29006 = EDGE_LOOP ( 'NONE', ( #8341, #12888, #31210, #78148 ) ) ;
#29007 = DIRECTION ( 'NONE',  ( -0.000000000000000000, -1.000000000000000000, -0.000000000000000000 ) ) ;
#29008 = DIRECTION ( 'NONE',  ( 0.000000000000000000, 0.000000000000000000, -1.000000000000000000 ) ) ;
#29009 = DIRECTION ( 'NONE',  ( 0.000000000000000000, 1.000000000000000000, 0.000000000000000000 ) ) ;
#29010 = CIRCLE ( 'NONE', #12257, 0.06509327318403745899 ) ;
#29011 = VERTEX_POINT ( 'NONE', #38993 ) ;
#29012 = EDGE_CURVE ( 'NONE', #72399, #3753, #111369, .T. ) ;
#29013 = FACE_BOUND ( 'NONE', #13453, .T. ) ;
#29014 = VERTEX_POINT ( 'NONE', #69051 ) ;
#29015 = ADVANCED_FACE ( 'NONE', ( #69701 ), #107176, .T. ) ;
#29016 = LINE ( 'NONE', #68917, #52186 ) ;
#29017 = DIRECTION ( 'NONE',  ( 0.000000000000000000, 0.000000000000000000, 1.000000000000000000 ) ) ;
#29018 = DIRECTION ( 'NONE',  ( 0.000000000000000000, 1.000000000000000000, 0.000000000000000000 ) ) ;
#29019 = AXIS2_PLACEMENT_3D ( 'NONE', #126126, #45652, #106492 ) ;
#29020 = LINE ( 'NONE', #77457, #84711 ) ;
#29021 = DIRECTION ( 'NONE',  ( 0.000000000000000000, -0.9999939076577903929, 0.003490651415223739937 ) ) ;
#29022 = EDGE_CURVE ( 'NONE', #37333, #113704, #99173, .T. ) ;
#29023 = CYLINDRICAL_SURFACE ( 'NONE', #14113, 7.699999999999999289 ) ;
#29024 = EDGE_CURVE ( 'NONE', #32318, #16607, #50762, .T. ) ;
#29025 = DIRECTION ( 'NONE',  ( 0.000000000000000000, 1.000000000000000000, 0.000000000000000000 ) ) ;
#29026 = CARTESIAN_POINT ( 'NONE',  ( -15.39999999999997904, 2.500000000000000000, 0.1000000000000000056 ) ) ;
#29027 = ADVANCED_FACE ( 'NONE', ( #10143 ), #19441, .T. ) ;
#29028 = CARTESIAN_POINT ( 'NONE',  ( 14.39999999999989555, 12.50000000000000000, -0.3464101615137782364 ) ) ;
#29029 = EDGE_CURVE ( 'NONE', #48878, #98420, #59183, .T. ) ;
#29030 = DIRECTION ( 'NONE',  ( 0.000000000000000000, -0.9999939076577903929, 0.003490651415223739937 ) ) ;
#29031 = ORIENTED_EDGE ( 'NONE', *, *, #10255, .T. ) ;
#29032 = ORIENTED_EDGE ( 'NONE', *, *, #95531, .T. ) ;
#29033 = ORIENTED_EDGE ( 'NONE', *, *, #96276, .T. ) ;
#29034 = VERTEX_POINT ( 'NONE', #88024 ) ;
#29035 = DIRECTION ( 'NONE',  ( 0.000000000000000000, 1.000000000000000000, 0.000000000000000000 ) ) ;
#29036 = DIRECTION ( 'NONE',  ( -0.000000000000000000, -1.000000000000000000, -0.000000000000000000 ) ) ;
#29038 = ORIENTED_EDGE ( 'NONE', *, *, #27847, .F. ) ;
#29037 = ORIENTED_EDGE ( 'NONE', *, *, #42802, .F. ) ;
#29039 = EDGE_CURVE ( 'NONE', #90795, #77606, #79995, .T. ) ;
#29040 = ORIENTED_EDGE ( 'NONE', *, *, #128407, .T. ) ;
#29041 = FACE_OUTER_BOUND ( 'NONE', #88375, .T. ) ;
#29042 = AXIS2_PLACEMENT_3D ( 'NONE', #86690, #125332, #97799 ) ;
#29043 = LINE ( 'NONE', #108859, #19536 ) ;
#29044 = DIRECTION ( 'NONE',  ( 0.000000000000000000, 1.000000000000000000, 0.000000000000000000 ) ) ;
#29046 = DIRECTION ( 'NONE',  ( -0.000000000000000000, -1.000000000000000000, -0.000000000000000000 ) ) ;
#29045 = AXIS2_PLACEMENT_3D ( 'NONE', #110493, #60757, #101970 ) ;
#29047 = CARTESIAN_POINT ( 'NONE',  ( -0.2000000000000347888, 12.50000000000000000, 0.2813168883297384459 ) ) ;
#29048 = DIRECTION ( 'NONE',  ( 0.000000000000000000, 1.000000000000000000, 0.000000000000000000 ) ) ;
#29049 = DIRECTION ( 'NONE',  ( -0.000000000000000000, -1.000000000000000000, -0.000000000000000000 ) ) ;
#29050 = ORIENTED_EDGE ( 'NONE', *, *, #112109, .F. ) ;
#29051 = VECTOR ( 'NONE', #126641, 1000.000000000000000 ) ;
#29053 = FACE_OUTER_BOUND ( 'NONE', #32051, .T. ) ;
#29052 = AXIS2_PLACEMENT_3D ( 'NONE', #28736, #98103, #68645 ) ;
#29054 = ORIENTED_EDGE ( 'NONE', *, *, #46315, .T. ) ;
#29055 = AXIS2_PLACEMENT_3D ( 'NONE', #127410, #88774, #37744 ) ;
#29056 = ORIENTED_EDGE ( 'NONE', *, *, #81991, .T. ) ;
#29057 = ORIENTED_EDGE ( 'NONE', *, *, #110575, .T. ) ;
#29058 = DIRECTION ( 'NONE',  ( 0.000000000000000000, 0.000000000000000000, 1.000000000000000000 ) ) ;
#29059 = EDGE_CURVE ( 'NONE', #81664, #72305, #56993, .T. ) ;
#29060 = ORIENTED_EDGE ( 'NONE', *, *, #117775, .F. ) ;
#29061 = ORIENTED_EDGE ( 'NONE', *, *, #20878, .T. ) ;
#29062 = CIRCLE ( 'NONE', #58300, 0.06509327318403745899 ) ;
#29063 = DIRECTION ( 'NONE',  ( -4.274815082592931898E-19, -0.9999939076577903929, -0.003490651415223739937 ) ) ;
#29064 = CIRCLE ( 'NONE', #102211, 0.06509327318403745899 ) ;
#29065 = DIRECTION ( 'NONE',  ( -0.000000000000000000, 1.000000000000000000, -0.000000000000000000 ) ) ;
#29066 = FACE_OUTER_BOUND ( 'NONE', #59679, .T. ) ;
#29067 = CARTESIAN_POINT ( 'NONE',  ( 14.39999999999989555, 12.50000000000000000, 0.4115034346978110880 ) ) ;
#29068 = LINE ( 'NONE', #82518, #81102 ) ;
#29069 = ADVANCED_FACE ( 'NONE', ( #89975 ), #18668, .T. ) ;
#29070 = ORIENTED_EDGE ( 'NONE', *, *, #17098, .F. ) ;
#29071 = EDGE_CURVE ( 'NONE', #87323, #47163, #78253, .T. ) ;
#29072 = DIRECTION ( 'NONE',  ( 0.000000000000000000, 0.000000000000000000, 1.000000000000000000 ) ) ;
#29073 = AXIS2_PLACEMENT_3D ( 'NONE', #105653, #35624, #65053 ) ;
#29074 = ORIENTED_EDGE ( 'NONE', *, *, #18396, .T. ) ;
#29076 = EDGE_CURVE ( 'NONE', #57844, #98275, #17274, .T. ) ;
#29075 = DIRECTION ( 'NONE',  ( 0.000000000000000000, 1.000000000000000000, 0.000000000000000000 ) ) ;
#29077 = ORIENTED_EDGE ( 'NONE', *, *, #87683, .T. ) ;
#29078 = DIRECTION ( 'NONE',  ( 0.000000000000000000, 0.000000000000000000, 1.000000000000000000 ) ) ;
#29079 = CARTESIAN_POINT ( 'NONE',  ( -8.100000000000010303, 2.500000000000000000, 4.676537180435972552 ) ) ;
#29080 = VERTEX_POINT ( 'NONE', #80826 ) ;
#29081 = FACE_BOUND ( 'NONE', #88903, .T. ) ;
#29082 = ADVANCED_FACE ( 'NONE', ( #120734 ), #67441, .T. ) ;
#29083 = CARTESIAN_POINT ( 'NONE',  ( -1.850000000000033396, 2.500000000000000000, -2.511473670974877948 ) ) ;
#29084 = EDGE_LOOP ( 'NONE', ( #40929, #84879, #92190, #102452 ) ) ;
#29085 = EDGE_CURVE ( 'NONE', #55389, #74101, #108331, .T. ) ;
#29086 = EDGE_CURVE ( 'NONE', #73329, #83060, #8832, .T. ) ;
#29087 = EDGE_CURVE ( 'NONE', #6145, #100851, #128657, .T. ) ;
#29088 = CIRCLE ( 'NONE', #85498, 0.09999999999999982514 ) ;
#29089 = DIRECTION ( 'NONE',  ( 0.000000000000000000, 1.000000000000000000, 0.000000000000000000 ) ) ;
#29090 = VERTEX_POINT ( 'NONE', #23100 ) ;
#29091 = VERTEX_POINT ( 'NONE', #5382 ) ;
#29092 = DIRECTION ( 'NONE',  ( 0.000000000000000000, 1.000000000000000000, 0.000000000000000000 ) ) ;
#29093 = DIRECTION ( 'NONE',  ( 0.000000000000000000, 0.000000000000000000, -1.000000000000000000 ) ) ;
#29094 = CARTESIAN_POINT ( 'NONE',  ( 4.599999999999939249, 12.50000000000000000, -3.637306695894650055 ) ) ;
#29096 = AXIS2_PLACEMENT_3D ( 'NONE', #81389, #11342, #110191 ) ;
#29095 = DIRECTION ( 'NONE',  ( 0.000000000000000000, 0.000000000000000000, 1.000000000000000000 ) ) ;
#29097 = ADVANCED_FACE ( 'NONE', ( #34226 ), #43402, .T. ) ;
#29098 = AXIS2_PLACEMENT_3D ( 'NONE', #30747, #33152, #109275 ) ;
#29099 = DIRECTION ( 'NONE',  ( 0.000000000000000000, -0.000000000000000000, 1.000000000000000000 ) ) ;
#29100 = VERTEX_POINT ( 'NONE', #54482 ) ;
#29101 = DIRECTION ( 'NONE',  ( 0.000000000000000000, 1.000000000000000000, 0.000000000000000000 ) ) ;
#29102 = CIRCLE ( 'NONE', #41628, 0.06509327318403745899 ) ;
#29103 = ORIENTED_EDGE ( 'NONE', *, *, #63810, .F. ) ;
#29104 = CARTESIAN_POINT ( 'NONE',  ( 9.149999999999920419, 2.500000000000000000, 1.572243186433545548 ) ) ;
#29105 = CARTESIAN_POINT ( 'NONE',  ( -5.600000000000023626, 2.500000000000000000, -4.676537180435977881 ) ) ;
#29106 = EDGE_LOOP ( 'NONE', ( #116837, #106072, #27312, #32210 ) ) ;
#29108 = AXIS2_PLACEMENT_3D ( 'NONE', #43159, #3845, #103991 ) ;
#29107 = CONICAL_SURFACE ( 'NONE', #45821, 0.1000000000000002554, 0.003490658503988666988 ) ;
#29109 = AXIS2_PLACEMENT_3D ( 'NONE', #97887, #6907, #8215 ) ;
#29110 = FACE_OUTER_BOUND ( 'NONE', #70940, .T. ) ;
#29111 = CARTESIAN_POINT ( 'NONE',  ( 179.5000000000000000, -1.000000000000025535, -7.634788798650553154 ) ) ;
#29112 = DIRECTION ( 'NONE',  ( 0.000000000000000000, 0.000000000000000000, 1.000000000000000000 ) ) ;
#29113 = LINE ( 'NONE', #16027, #31344 ) ;
#29114 = FACE_OUTER_BOUND ( 'NONE', #31643, .T. ) ;
#29115 = ORIENTED_EDGE ( 'NONE', *, *, #57810, .F. ) ;
#29117 = VECTOR ( 'NONE', #128782, 1000.000000000000000 ) ;
#29116 = AXIS2_PLACEMENT_3D ( 'NONE', #102620, #53542, #94100 ) ;
#29118 = CARTESIAN_POINT ( 'NONE',  ( 7.499999999999927169, 2.500000000000000000, 3.637306695894644726 ) ) ;
#29119 = CARTESIAN_POINT ( 'NONE',  ( -9.600000000000008527, 2.500000000000000000, -3.637306695894645614 ) ) ;
#29120 = DIRECTION ( 'NONE',  ( 0.000000000000000000, 0.000000000000000000, 1.000000000000000000 ) ) ;
#29121 = ORIENTED_EDGE ( 'NONE', *, *, #16582, .T. ) ;
#29122 = DIRECTION ( 'NONE',  ( -0.000000000000000000, 1.000000000000000000, -0.000000000000000000 ) ) ;
#29123 = EDGE_CURVE ( 'NONE', #37856, #100700, #21514, .T. ) ;
#29124 = VERTEX_POINT ( 'NONE', #53217 ) ;
#29125 = EDGE_LOOP ( 'NONE', ( #58702, #106124, #35774, #7563 ) ) ;
#29126 = LINE ( 'NONE', #16679, #94739 ) ;
#29127 = AXIS2_PLACEMENT_3D ( 'NONE', #6122, #76174, #113509 ) ;
#29128 = ORIENTED_EDGE ( 'NONE', *, *, #18555, .T. ) ;
#29129 = FACE_OUTER_BOUND ( 'NONE', #40113, .T. ) ;
#29130 = DIRECTION ( 'NONE',  ( -0.000000000000000000, -1.000000000000000000, -0.000000000000000000 ) ) ;
#29131 = ORIENTED_EDGE ( 'NONE', *, *, #53530, .T. ) ;
#29132 = CARTESIAN_POINT ( 'NONE',  ( 5.849999999999935696, 12.50000000000000000, -6.560283801567339701 ) ) ;
#29133 = AXIS2_PLACEMENT_3D ( 'NONE', #71909, #111828, #111149 ) ;
#29135 = EDGE_LOOP ( 'NONE', ( #50413, #89224 ) ) ;
#29134 = DIRECTION ( 'NONE',  ( 0.000000000000000000, 0.000000000000000000, 1.000000000000000000 ) ) ;
#29136 = CYLINDRICAL_SURFACE ( 'NONE', #21443, 5.000000000000000000 ) ;
#29137 = EDGE_CURVE ( 'NONE', #84308, #103467, #112777, .T. ) ;
#29138 = LINE ( 'NONE', #69033, #55073 ) ;
#29139 = AXIS2_PLACEMENT_3D ( 'NONE', #23779, #63701, #104263 ) ;
#29140 = EDGE_LOOP ( 'NONE', ( #47732, #10786, #86811, #92440 ) ) ;
#29141 = AXIS2_PLACEMENT_3D ( 'NONE', #116930, #88103, #128063 ) ;
#29142 = CONICAL_SURFACE ( 'NONE', #125273, 0.1000000000000002554, 0.003490658503988666988 ) ;
#29143 = ORIENTED_EDGE ( 'NONE', *, *, #97619, .T. ) ;
#29144 = ORIENTED_EDGE ( 'NONE', *, *, #90089, .F. ) ;
#29145 = DIRECTION ( 'NONE',  ( 0.000000000000000000, 0.000000000000000000, 1.000000000000000000 ) ) ;
#29146 = DIRECTION ( 'NONE',  ( -0.000000000000000000, -1.000000000000000000, -0.000000000000000000 ) ) ;
#29147 = LINE ( 'NONE', #79524, #58851 ) ;
#29148 = FACE_BOUND ( 'NONE', #111594, .T. ) ;
#29149 = VERTEX_POINT ( 'NONE', #65595 ) ;
#29150 = CIRCLE ( 'NONE', #10261, 0.06509327318403743123 ) ;
#29151 = CARTESIAN_POINT ( 'NONE',  ( 9.199999999999915801, 12.50000000000000000, 4.330127018922196314 ) ) ;
#29152 = CARTESIAN_POINT ( 'NONE',  ( 7.949999999999925571, 2.500000000000000000, 2.165063509461097713 ) ) ;
#29153 = ORIENTED_EDGE ( 'NONE', *, *, #115256, .T. ) ;
#29154 = DIRECTION ( 'NONE',  ( 0.000000000000000000, 0.000000000000000000, 1.000000000000000000 ) ) ;
#29155 = DIRECTION ( 'NONE',  ( 0.000000000000000000, -1.000000000000000000, 0.000000000000000000 ) ) ;
#29156 = AXIS2_PLACEMENT_3D ( 'NONE', #45387, #106231, #33626 ) ;
#29157 = DIRECTION ( 'NONE',  ( 0.000000000000000000, 1.000000000000000000, 0.000000000000000000 ) ) ;
#29158 = CARTESIAN_POINT ( 'NONE',  ( -1.850000000000033840, 2.500000000000000000, 6.841600689897072485 ) ) ;
#29159 = CARTESIAN_POINT ( 'NONE',  ( 6.649999999999930189, 12.50000000000000000, 5.802370205355744659 ) ) ;
#29160 = FACE_OUTER_BOUND ( 'NONE', #68524, .T. ) ;
#29161 = CARTESIAN_POINT ( 'NONE',  ( -0.2000000000000404232, 12.50000000000000000, 3.918623584224383727 ) ) ;
#29162 = EDGE_CURVE ( 'NONE', #28223, #15955, #23656, .T. ) ;
#29163 = EDGE_LOOP ( 'NONE', ( #122599, #81252, #60775, #61714 ) ) ;
#29164 = VERTEX_POINT ( 'NONE', #102942 ) ;
#29165 = ORIENTED_EDGE ( 'NONE', *, *, #34059, .T. ) ;
#29166 = EDGE_LOOP ( 'NONE', ( #27306, #30586, #76136, #104708 ) ) ;
#29167 = ORIENTED_EDGE ( 'NONE', *, *, #28267, .F. ) ;
#29168 = AXIS2_PLACEMENT_3D ( 'NONE', #118259, #59376, #29257 ) ;
#29169 = CARTESIAN_POINT ( 'NONE',  ( 1.899999999999949507, 12.50000000000000000, 4.048810130592458201 ) ) ;
#29170 = DIRECTION ( 'NONE',  ( -0.000000000000000000, -1.000000000000000000, -0.000000000000000000 ) ) ;
#29171 = ORIENTED_EDGE ( 'NONE', *, *, #112319, .T. ) ;
#29172 = FACE_BOUND ( 'NONE', #118081, .T. ) ;
#29173 = EDGE_CURVE ( 'NONE', #31947, #104830, #36297, .T. ) ;
#29174 = LINE ( 'NONE', #50727, #8144 ) ;
#29175 = CARTESIAN_POINT ( 'NONE',  ( -11.89999999999999503, 12.50000000000000000, 4.048810130592458201 ) ) ;
#29176 = EDGE_CURVE ( 'NONE', #27665, #108330, #63023, .T. ) ;
#29177 = DIRECTION ( 'NONE',  ( -0.000000000000000000, -1.000000000000000000, -0.000000000000000000 ) ) ;
#29178 = EDGE_CURVE ( 'NONE', #76002, #95427, #78501, .T. ) ;
#29179 =( BOUNDED_CURVE ( )  B_SPLINE_CURVE ( 2, ( #28346, #129144, #39473, #19131, #800, #98348, #59093 ),
 .UNSPECIFIED., .F., .F. ) 
 B_SPLINE_CURVE_WITH_KNOTS ( ( 3, 2, 2, 3 ),
 ( 0.5000000000000004441, 0.5238095238095242800, 0.5476190476190482270, 0.5714285714285719520 ),
 .UNSPECIFIED. ) 
 CURVE ( )  GEOMETRIC_REPRESENTATION_ITEM ( )  RATIONAL_B_SPLINE_CURVE ( ( 0.9999999999999974465, 0.8660254037844412611, 1.000000000000000000, 0.8660254037844387076, 1.000000000000000000, 0.8660254037844355990, 1.000000000000003109 ) ) 
 REPRESENTATION_ITEM ( '' )  );
#29180 = FACE_OUTER_BOUND ( 'NONE', #64658, .T. ) ;
#29181 = ADVANCED_FACE ( 'NONE', ( #115307 ), #83320, .T. ) ;
#29182 = CARTESIAN_POINT ( 'NONE',  ( -3.100000000000028511, 2.500000000000000000, -4.676537180435977881 ) ) ;
#29183 = EDGE_CURVE ( 'NONE', #95681, #18715, #84292, .T. ) ;
#29184 = VERTEX_POINT ( 'NONE', #45974 ) ;
#29185 = EDGE_CURVE ( 'NONE', #99172, #110598, #55049, .T. ) ;
#29186 = AXIS2_PLACEMENT_3D ( 'NONE', #39548, #43397, #112774 ) ;
#29187 = ORIENTED_EDGE ( 'NONE', *, *, #70254, .F. ) ;
#29188 = VERTEX_POINT ( 'NONE', #74139 ) ;
#29189 = ORIENTED_EDGE ( 'NONE', *, *, #102583, .F. ) ;
#29190 = DIRECTION ( 'NONE',  ( 0.000000000000000000, 0.000000000000000000, -1.000000000000000000 ) ) ;
#29191 = CARTESIAN_POINT ( 'NONE',  ( 4.599999999999936584, 2.500000000000000000, 4.330127018922196314 ) ) ;
#29192 = CIRCLE ( 'NONE', #4023, 0.06509327318403745899 ) ;
#29193 = EDGE_LOOP ( 'NONE', ( #21759, #1352, #6900, #10160 ) ) ;
#29194 = ADVANCED_FACE ( 'NONE', ( #63679 ), #128229, .T. ) ;
#29195 = CARTESIAN_POINT ( 'NONE',  ( 12.69999999999989981, 2.500000000000000000, -0.4464101615137783252 ) ) ;
#29196 = EDGE_CURVE ( 'NONE', #66128, #15541, #96806, .T. ) ;
#29197 = CARTESIAN_POINT ( 'NONE',  ( -15.59999999999998010, 12.50000000000000000, -0.3464101615137759604 ) ) ;
#29198 = EDGE_CURVE ( 'NONE', #88710, #119959, #48806, .T. ) ;
#29201 = VECTOR ( 'NONE', #4965, 1000.000000000000000 ) ;
#29200 = FACE_OUTER_BOUND ( 'NONE', #81494, .T. ) ;
#29199 = CONICAL_SURFACE ( 'NONE', #81421, 0.1000000000000002554, 0.003490658503988666988 ) ;
#29202 = CARTESIAN_POINT ( 'NONE',  ( 184.4010416670080872, -4.367472073101519747, 7.564683531249999149 ) ) ;
#29203 = FACE_OUTER_BOUND ( 'NONE', #84235, .T. ) ;
#29204 = DIRECTION ( 'NONE',  ( 0.000000000000000000, 1.000000000000000000, 0.000000000000000000 ) ) ;
#29205 = AXIS2_PLACEMENT_3D ( 'NONE', #102414, #34334, #53320 ) ;
#29206 = DIRECTION ( 'NONE',  ( 0.000000000000000000, 0.000000000000000000, 1.000000000000000000 ) ) ;
#29207 = VERTEX_POINT ( 'NONE', #124532 ) ;
#29208 = DIRECTION ( 'NONE',  ( 0.000000000000000000, 0.000000000000000000, 1.000000000000000000 ) ) ;
#29209 = CIRCLE ( 'NONE', #66820, 0.09999999999999982514 ) ;
#29210 = VERTEX_POINT ( 'NONE', #34875 ) ;
#29211 = VERTEX_POINT ( 'NONE', #74782 ) ;
#29212 = CARTESIAN_POINT ( 'NONE',  ( 8.149999999999923972, 2.500000000000000000, 2.511473670974873507 ) ) ;
#29213 = CARTESIAN_POINT ( 'NONE',  ( -3.550000000000028244, 2.500000000000000000, 2.611473670974873151 ) ) ;
#29214 = CARTESIAN_POINT ( 'NONE',  ( 1.849999999999950573, 2.500000000000000000, 2.511473670974873507 ) ) ;
#29215 = ORIENTED_EDGE ( 'NONE', *, *, #72214, .F. ) ;
#29216 = ORIENTED_EDGE ( 'NONE', *, *, #90518, .T. ) ;
#29217 = CARTESIAN_POINT ( 'NONE',  ( 3.149999999999946176, 2.500000000000000000, -2.511473670974877948 ) ) ;
#29218 = CARTESIAN_POINT ( 'NONE',  ( -0.8500000000000386136, 2.500000000000000000, 1.472243186433545459 ) ) ;
#29219 = CARTESIAN_POINT ( 'NONE',  ( -3.100000000000028955, 2.500000000000000000, 4.576537180435972019 ) ) ;
#29221 = ORIENTED_EDGE ( 'NONE', *, *, #90322, .T. ) ;
#29220 = CIRCLE ( 'NONE', #102368, 0.1000000000000002554 ) ;
#29222 = DIRECTION ( 'NONE',  ( -4.274815082592931898E-19, -0.9999939076577903929, -0.003490651415223739937 ) ) ;
#29223 = VERTEX_POINT ( 'NONE', #64938 ) ;
#29224 = FACE_OUTER_BOUND ( 'NONE', #105081, .T. ) ;
#29225 = AXIS2_PLACEMENT_3D ( 'NONE', #20985, #91659, #41931 ) ;
#29226 = AXIS2_PLACEMENT_3D ( 'NONE', #107138, #66569, #127446 ) ;
#29227 = ORIENTED_EDGE ( 'NONE', *, *, #80000, .F. ) ;
#29228 = DIRECTION ( 'NONE',  ( -0.000000000000000000, 1.000000000000000000, -0.000000000000000000 ) ) ;
#29229 = DIRECTION ( 'NONE',  ( 0.000000000000000000, 1.000000000000000000, 0.000000000000000000 ) ) ;
#29230 = CARTESIAN_POINT ( 'NONE',  ( -6.900000000000019007, 12.50000000000000000, -4.741630453620016006 ) ) ;
#29231 = ADVANCED_FACE ( 'NONE', ( #24390 ), #63373, .T. ) ;
#29232 = DIRECTION ( 'NONE',  ( 0.000000000000000000, 0.000000000000000000, 1.000000000000000000 ) ) ;
#29233 = EDGE_LOOP ( 'NONE', ( #134, #7557, #77820, #31032 ) ) ;
#29235 = AXIS2_PLACEMENT_3D ( 'NONE', #27563, #45950, #125146 ) ;
#29234 = AXIS2_PLACEMENT_3D ( 'NONE', #42268, #72378, #44183 ) ;
#29236 = ADVANCED_FACE ( 'NONE', ( #55140 ), #113541, .T. ) ;
#29237 = DIRECTION ( 'NONE',  ( -0.000000000000000000, 1.000000000000000000, -0.000000000000000000 ) ) ;
#29238 = EDGE_CURVE ( 'NONE', #84136, #107557, #78033, .T. ) ;
#29239 = VERTEX_POINT ( 'NONE', #19051 ) ;
#29240 = ORIENTED_EDGE ( 'NONE', *, *, #103566, .T. ) ;
#29241 = CARTESIAN_POINT ( 'NONE',  ( 14.59999999999989484, 2.500000000000000000, -2.276824562219559311E-15 ) ) ;
#29242 = CARTESIAN_POINT ( 'NONE',  ( 2.299999999999946976, 12.50000000000000000, 4.676537180435972552 ) ) ;
#29243 = LINE ( 'NONE', #78988, #5151 ) ;
#29244 = CARTESIAN_POINT ( 'NONE',  ( 187.1093750003414016, 9.264065473108010111E-16, -7.564683531250000925 ) ) ;
#29245 = CARTESIAN_POINT ( 'NONE',  ( 9.999999999999912959, 2.500000000000000000, -5.022947341949754119 ) ) ;
#29246 = EDGE_CURVE ( 'NONE', #69185, #12706, #46744, .T. ) ;
#29247 = DIRECTION ( 'NONE',  ( -0.000000000000000000, 1.000000000000000000, -0.000000000000000000 ) ) ;
#29248 = AXIS2_PLACEMENT_3D ( 'NONE', #114726, #5413, #25063 ) ;
#29249 = CONICAL_SURFACE ( 'NONE', #102396, 0.1000000000000002554, 0.003490658503988666988 ) ;
#29250 = DIRECTION ( 'NONE',  ( -0.000000000000000000, 1.000000000000000000, -0.000000000000000000 ) ) ;
#29251 = DIRECTION ( 'NONE',  ( 0.000000000000000000, 0.000000000000000000, 1.000000000000000000 ) ) ;
#29252 = CARTESIAN_POINT ( 'NONE',  ( 15.79999999999989058, 2.500000000000000000, 0.09999999999999761857 ) ) ;
#29253 = CONICAL_SURFACE ( 'NONE', #66879, 0.1000000000000000056, 0.003490658503988666988 ) ;
#29254 = EDGE_LOOP ( 'NONE', ( #54043, #101967 ) ) ;
#29255 = VECTOR ( 'NONE', #74112, 1000.000000000000000 ) ;
#29256 = CARTESIAN_POINT ( 'NONE',  ( 127.5000000000000000, -2.000000000000000000, 2.000000000000001776 ) ) ;
#29257 = DIRECTION ( 'NONE',  ( 0.000000000000000000, 0.000000000000000000, 1.000000000000000000 ) ) ;
#29258 = LINE ( 'NONE', #15698, #78876 ) ;
#29259 = EDGE_CURVE ( 'NONE', #74685, #66198, #25810, .T. ) ;
#29260 = FACE_OUTER_BOUND ( 'NONE', #100562, .T. ) ;
#29261 = CARTESIAN_POINT ( 'NONE',  ( 9.199999999999915801, 2.500000000000000000, 4.330127018922196314 ) ) ;
#29262 = VERTEX_POINT ( 'NONE', #57053 ) ;
#29263 = DIRECTION ( 'NONE',  ( -0.000000000000000000, -1.000000000000000000, -0.000000000000000000 ) ) ;
#29264 = DIRECTION ( 'NONE',  ( -0.000000000000000000, 1.000000000000000000, -0.000000000000000000 ) ) ;
#29266 = ORIENTED_EDGE ( 'NONE', *, *, #102136, .T. ) ;
#29265 = LINE ( 'NONE', #30566, #27518 ) ;
#29267 = VERTEX_POINT ( 'NONE', #57724 ) ;
#29268 = DIRECTION ( 'NONE',  ( 0.000000000000000000, 0.000000000000000000, 1.000000000000000000 ) ) ;
#29270 = VERTEX_POINT ( 'NONE', #16475 ) ;
#29269 = EDGE_CURVE ( 'NONE', #85304, #103404, #66875, .T. ) ;
#29271 = VERTEX_POINT ( 'NONE', #128413 ) ;
#29272 = EDGE_LOOP ( 'NONE', ( #7401, #47047 ) ) ;
#29273 = DIRECTION ( 'NONE',  ( 0.000000000000000000, 0.000000000000000000, 1.000000000000000000 ) ) ;
#29274 = CONICAL_SURFACE ( 'NONE', #102430, 0.1000000000000000056, 0.003490658503988666988 ) ;
#29275 = CARTESIAN_POINT ( 'NONE',  ( 3.349999999999942801, 12.50000000000000000, 2.857883832488649301 ) ) ;
#29276 = FACE_OUTER_BOUND ( 'NONE', #67210, .T. ) ;
#29277 = CARTESIAN_POINT ( 'NONE',  ( 2.949999999999946887, 2.500000000000000000, -6.595190528383302109 ) ) ;
#29278 = EDGE_LOOP ( 'NONE', ( #116737, #23005 ) ) ;
#29279 = CONICAL_SURFACE ( 'NONE', #56446, 0.09999999999999982514, 0.003490658503988666988 ) ;
#29280 = DIRECTION ( 'NONE',  ( 0.000000000000000000, 1.000000000000000000, 0.000000000000000000 ) ) ;
#29281 = ORIENTED_EDGE ( 'NONE', *, *, #61721, .T. ) ;
#29282 = DIRECTION ( 'NONE',  ( 0.000000000000000000, 0.000000000000000000, 1.000000000000000000 ) ) ;
#29283 = CARTESIAN_POINT ( 'NONE',  ( 16.86689433361522461, 2.548103353434407747, 5.776876940644654290 ) ) ;
#29284 = CARTESIAN_POINT ( 'NONE',  ( 6.649999999999927525, 2.500000000000000000, 2.065063509461097624 ) ) ;
#29285 = ADVANCED_FACE ( 'NONE', ( #66232 ), #56414, .T. ) ;
#29286 = DIRECTION ( 'NONE',  ( 0.000000000000000000, 0.000000000000000000, -1.000000000000000000 ) ) ;
#29287 = ORIENTED_EDGE ( 'NONE', *, *, #60916, .T. ) ;
#29289 = AXIS2_PLACEMENT_3D ( 'NONE', #7855, #7204, #6531 ) ;
#29288 = AXIS2_PLACEMENT_3D ( 'NONE', #127136, #106199, #56434 ) ;
#29290 = ORIENTED_EDGE ( 'NONE', *, *, #57717, .T. ) ;
#29291 = ORIENTED_EDGE ( 'NONE', *, *, #115934, .F. ) ;
#29292 = VERTEX_POINT ( 'NONE', #127110 ) ;
#29293 = ORIENTED_EDGE ( 'NONE', *, *, #4601, .T. ) ;
#29294 = CARTESIAN_POINT ( 'NONE',  ( -5.400000000000023448, 12.50000000000000000, -4.330127018922201643 ) ) ;
#29295 = DIRECTION ( 'NONE',  ( 0.000000000000000000, -0.9999939076577903929, 0.003490651415223739937 ) ) ;
#29296 = EDGE_CURVE ( 'NONE', #58654, #12633, #96329, .T. ) ;
#29297 = DIRECTION ( 'NONE',  ( -4.274815082592931898E-19, -0.9999939076577903929, -0.003490651415223739937 ) ) ;
#29298 = FACE_BOUND ( 'NONE', #76187, .T. ) ;
#29299 = DIRECTION ( 'NONE',  ( 0.000000000000000000, 1.000000000000000000, 0.000000000000000000 ) ) ;
#29300 = CARTESIAN_POINT ( 'NONE',  ( 186.0729166673494319, 4.445597072760120838, -7.699999999999998401 ) ) ;
#29301 = DIRECTION ( 'NONE',  ( 0.000000000000000000, -0.000000000000000000, 1.000000000000000000 ) ) ;
#29302 = FACE_OUTER_BOUND ( 'NONE', #87189, .T. ) ;
#29303 = DIRECTION ( 'NONE',  ( 0.000000000000000000, 0.000000000000000000, 1.000000000000000000 ) ) ;
#29304 = DIRECTION ( 'NONE',  ( 0.000000000000000000, 0.000000000000000000, 1.000000000000000000 ) ) ;
#29305 = DIRECTION ( 'NONE',  ( 0.000000000000000000, -0.9999939076577903929, 0.003490651415223739937 ) ) ;
#29306 = CONICAL_SURFACE ( 'NONE', #31457, 0.09999999999999999167, 0.003490658503988666988 ) ;
#29307 = DIRECTION ( 'NONE',  ( 0.000000000000000000, 1.000000000000000000, 0.000000000000000000 ) ) ;
#29308 = EDGE_CURVE ( 'NONE', #76747, #104576, #27861, .T. ) ;
#29309 = ORIENTED_EDGE ( 'NONE', *, *, #47576, .F. ) ;
#29310 = ORIENTED_EDGE ( 'NONE', *, *, #54545, .F. ) ;
#29311 = ORIENTED_EDGE ( 'NONE', *, *, #57561, .F. ) ;
#29312 = ORIENTED_EDGE ( 'NONE', *, *, #43933, .T. ) ;
#29313 = CARTESIAN_POINT ( 'NONE',  ( -12.09999999999999609, 2.500000000000000000, 0.7928203230275536750 ) ) ;
#29314 = CARTESIAN_POINT ( 'NONE',  ( 0.5999999999999555689, 2.500000000000000000, 4.576537180435972019 ) ) ;
#29315 = FACE_BOUND ( 'NONE', #96771, .T. ) ;
#29316 = CIRCLE ( 'NONE', #27242, 0.06509327318403741736 ) ;
#29317 = DIRECTION ( 'NONE',  ( 0.000000000000000000, 0.000000000000000000, 1.000000000000000000 ) ) ;
#29318 = ADVANCED_FACE ( 'NONE', ( #67506 ), #65504, .T. ) ;
#29319 = EDGE_LOOP ( 'NONE', ( #21798, #61844 ) ) ;
#29320 = EDGE_CURVE ( 'NONE', #105793, #15536, #40400, .T. ) ;
#29321 = PLANE ( 'NONE',  #75955 ) ;
#29322 = CARTESIAN_POINT ( 'NONE',  ( -11.25000000000000000, 2.500000000000000000, 2.757883832488649656 ) ) ;
#29323 = ADVANCED_FACE ( 'NONE', ( #86518 ), #119893, .T. ) ;
#29324 = DIRECTION ( 'NONE',  ( 0.000000000000000000, -0.9999939076577903929, 0.003490651415223739937 ) ) ;
#29325 = FACE_OUTER_BOUND ( 'NONE', #73135, .T. ) ;
#29326 = ADVANCED_FACE ( 'NONE', ( #7957 ), #15323, .T. ) ;
#29327 = CARTESIAN_POINT ( 'NONE',  ( 7.099999999999928590, 12.50000000000000000, -4.330127018922201643 ) ) ;
#29329 = EDGE_CURVE ( 'NONE', #7687, #50249, #116622, .T. ) ;
#29328 = AXIS2_PLACEMENT_3D ( 'NONE', #16390, #85794, #65513 ) ;
#29330 = EDGE_LOOP ( 'NONE', ( #25678, #75069, #54062, #11713 ) ) ;
#29331 = CARTESIAN_POINT ( 'NONE',  ( 4.599999999999940137, 2.500000000000000000, -5.022947341949754119 ) ) ;
#29332 = VECTOR ( 'NONE', #93017, 1000.000000000000000 ) ;
#29333 = AXIS2_PLACEMENT_3D ( 'NONE', #122979, #119, #89160 ) ;
#29334 = ORIENTED_EDGE ( 'NONE', *, *, #17755, .F. ) ;
#29335 = EDGE_CURVE ( 'NONE', #22598, #116333, #98963, .T. ) ;
#29336 = EDGE_LOOP ( 'NONE', ( #21621, #99236 ) ) ;
#29337 = CARTESIAN_POINT ( 'NONE',  ( 6.649999999999930189, 12.50000000000000000, 7.122917578226811486 ) ) ;
#29338 = ADVANCED_FACE ( 'NONE', ( #129055 ), #111482, .T. ) ;
#29339 = CARTESIAN_POINT ( 'NONE',  ( -0.4000000000000331624, 12.50000000000000000, 0.000000000000000000 ) ) ;
#29340 = ORIENTED_EDGE ( 'NONE', *, *, #120908, .F. ) ;
#29341 = EDGE_CURVE ( 'NONE', #33171, #56826, #32083, .T. ) ;
#29342 = CIRCLE ( 'NONE', #96206, 0.06509327318403745899 ) ;
#29343 = ADVANCED_FACE ( 'NONE', ( #118556 ), #105221, .T. ) ;
#29344 = CARTESIAN_POINT ( 'NONE',  ( 8.349999999999919709, 2.500000000000000000, 6.595190528383296780 ) ) ;
#29345 = EDGE_CURVE ( 'NONE', #93190, #43830, #9259, .T. ) ;
#29346 = DIRECTION ( 'NONE',  ( -0.000000000000000000, -1.000000000000000000, -0.000000000000000000 ) ) ;
#29347 = EDGE_LOOP ( 'NONE', ( #55017, #84769, #78861, #82899 ) ) ;
#29348 = CARTESIAN_POINT ( 'NONE',  ( 2.049999999999948308, 12.50000000000000000, 6.495190528383297135 ) ) ;
#29349 = AXIS2_PLACEMENT_3D ( 'NONE', #98191, #37357, #7216 ) ;
#29350 = VERTEX_POINT ( 'NONE', #99584 ) ;
#29351 = DIRECTION ( 'NONE',  ( 0.000000000000000000, 0.000000000000000000, 1.000000000000000000 ) ) ;
#29352 = ADVANCED_FACE ( 'NONE', ( #1358 ), #86432, .T. ) ;
#29353 = EDGE_LOOP ( 'NONE', ( #48852, #103251 ) ) ;
#29354 = CARTESIAN_POINT ( 'NONE',  ( 5.849999999999935696, 2.500000000000000000, -7.188010851410854052 ) ) ;
#29355 = FACE_BOUND ( 'NONE', #107959, .T. ) ;
#29356 = ORIENTED_EDGE ( 'NONE', *, *, #116485, .F. ) ;
#29357 = CARTESIAN_POINT ( 'NONE',  ( -5.400000000000020783, 2.500000000000000000, 0.6928203230275494784 ) ) ;
#29358 = ORIENTED_EDGE ( 'NONE', *, *, #50456, .F. ) ;
#29359 = CARTESIAN_POINT ( 'NONE',  ( 2.891205793294708895E-16, 2.000000000000000000, 2.000000000000020428 ) ) ;
#29360 = LINE ( 'NONE', #60742, #105212 ) ;
#29361 = DIRECTION ( 'NONE',  ( 1.000000000000000000, -0.000000000000000000, -0.000000000000000000 ) ) ;
#29362 = CARTESIAN_POINT ( 'NONE',  ( 129.5000000000000000, 0.000000000000000000, 0.000000000000000000 ) ) ;
#29363 = CARTESIAN_POINT ( 'NONE',  ( -4.600000000000024514, 12.50000000000000000, 5.022947341949748790 ) ) ;
#29364 = ORIENTED_EDGE ( 'NONE', *, *, #87253, .T. ) ;
#29365 = ORIENTED_EDGE ( 'NONE', *, *, #94325, .T. ) ;
#29366 = VERTEX_POINT ( 'NONE', #111296 ) ;
#29367 = FACE_OUTER_BOUND ( 'NONE', #75407, .T. ) ;
#29368 = FACE_OUTER_BOUND ( 'NONE', #82699, .T. ) ;
#29370 = DIRECTION ( 'NONE',  ( 0.000000000000000000, 1.000000000000000000, 0.000000000000000000 ) ) ;
#29369 = AXIS2_PLACEMENT_3D ( 'NONE', #32459, #80893, #90703 ) ;
#29372 = ORIENTED_EDGE ( 'NONE', *, *, #58574, .F. ) ;
#29371 = EDGE_LOOP ( 'NONE', ( #83777, #14926 ) ) ;
#29373 = ORIENTED_EDGE ( 'NONE', *, *, #54256, .F. ) ;
#29374 = CONICAL_SURFACE ( 'NONE', #10556, 0.1000000000000002554, 0.003490658503988666988 ) ;
#29375 = DIRECTION ( 'NONE',  ( -0.000000000000000000, -1.000000000000000000, -0.000000000000000000 ) ) ;
#29376 = DIRECTION ( 'NONE',  ( 0.000000000000000000, 0.000000000000000000, 1.000000000000000000 ) ) ;
#29377 = SHAPE_DEFINITION_REPRESENTATION ( #88883, #102928 ) ;
#29379 = VECTOR ( 'NONE', #94478, 1000.000000000000000 ) ;
#29378 = CONICAL_SURFACE ( 'NONE', #25148, 0.09999999999999982514, 0.003490658503988666988 ) ;
#29380 = DIRECTION ( 'NONE',  ( 0.000000000000000000, 0.000000000000000000, -1.000000000000000000 ) ) ;
#29381 = DIRECTION ( 'NONE',  ( 0.000000000000000000, 1.000000000000000000, 0.000000000000000000 ) ) ;
#29382 = FACE_OUTER_BOUND ( 'NONE', #62896, .T. ) ;
#29383 = CARTESIAN_POINT ( 'NONE',  ( -10.84999999999999964, 12.50000000000000000, 7.122917578226811486 ) ) ;
#29384 = DIRECTION ( 'NONE',  ( 0.000000000000000000, 1.000000000000000000, 0.000000000000000000 ) ) ;
#29385 = CARTESIAN_POINT ( 'NONE',  ( 13.34999999999989662, 2.500000000000000000, -2.757883832488654097 ) ) ;
#29386 = EDGE_LOOP ( 'NONE', ( #94260, #106507, #19217, #22736 ) ) ;
#29387 = ORIENTED_EDGE ( 'NONE', *, *, #58998, .T. ) ;
#29388 = EDGE_CURVE ( 'NONE', #19644, #103729, #21661, .T. ) ;
#29389 = DIRECTION ( 'NONE',  ( -0.000000000000000000, 1.000000000000000000, -0.000000000000000000 ) ) ;
#29390 = EDGE_CURVE ( 'NONE', #84227, #69984, #41953, .T. ) ;
#29391 = CARTESIAN_POINT ( 'NONE',  ( 6.049999999999932321, 12.50000000000000000, 6.841600689897072485 ) ) ;
#29392 = EDGE_LOOP ( 'NONE', ( #62358, #74356 ) ) ;
#29393 = ORIENTED_EDGE ( 'NONE', *, *, #24321, .T. ) ;
#29394 = CARTESIAN_POINT ( 'NONE',  ( 185.2760416670080588, 6.551208109652274736, 3.782341765625001351 ) ) ;
#29395 = FACE_OUTER_BOUND ( 'NONE', #61343, .T. ) ;
#29396 = CARTESIAN_POINT ( 'NONE',  ( 8.749999999999953815, 12.50000000000000000, -2.099970236277064473 ) ) ;
#29397 = EDGE_CURVE ( 'NONE', #46240, #48600, #9901, .T. ) ;
#29398 = DIRECTION ( 'NONE',  ( 0.000000000000000000, 0.000000000000000000, 1.000000000000000000 ) ) ;
#29399 = CARTESIAN_POINT ( 'NONE',  ( 12.04999999999990479, 2.500000000000000000, 2.165063509461097713 ) ) ;
#29400 = CARTESIAN_POINT ( 'NONE',  ( -6.050000000000020250, 2.500000000000000000, -6.841600689897078702 ) ) ;
#29401 = CARTESIAN_POINT ( 'NONE',  ( -13.09999999999999254, 12.50000000000000000, -4.676537180435975216 ) ) ;
#29402 = CARTESIAN_POINT ( 'NONE',  ( 0.8499999999999545697, 12.50000000000000000, -1.472243186433550122 ) ) ;
#29403 = VECTOR ( 'NONE', #41328, 1000.000000000000000 ) ;
#29405 = EDGE_LOOP ( 'NONE', ( #39247, #85397, #60714, #126785 ) ) ;
#29404 = CIRCLE ( 'NONE', #27313, 0.06509327318403745899 ) ;
#29406 = ORIENTED_EDGE ( 'NONE', *, *, #10123, .F. ) ;
#29407 = EDGE_LOOP ( 'NONE', ( #73400, #128312 ) ) ;
#29408 = ORIENTED_EDGE ( 'NONE', *, *, #36845, .T. ) ;
#29409 = DIRECTION ( 'NONE',  ( -0.000000000000000000, -1.000000000000000000, -0.000000000000000000 ) ) ;
#29410 = CARTESIAN_POINT ( 'NONE',  ( -3.150000000000033218, 2.500000000000000000, -6.841600689897078702 ) ) ;
#29411 = CONICAL_SURFACE ( 'NONE', #48183, 0.1000000000000002554, 0.003490658503988666988 ) ;
#29412 = VERTEX_POINT ( 'NONE', #121140 ) ;
#29413 = CARTESIAN_POINT ( 'NONE',  ( 9.349999999999919709, 2.500000000000000000, 1.718653347947321386 ) ) ;
#29414 = CARTESIAN_POINT ( 'NONE',  ( 3.749999999999978684, 2.500000000000000000, -2.165063509461101710 ) ) ;
#29415 = DIRECTION ( 'NONE',  ( 0.000000000000000000, 0.000000000000000000, 1.000000000000000000 ) ) ;
#29417 = ORIENTED_EDGE ( 'NONE', *, *, #42037, .T. ) ;
#29416 = CARTESIAN_POINT ( 'NONE',  ( 0.7999999999999612976, 12.50000000000000000, -1.084202172485504434E-16 ) ) ;
#29418 = DIRECTION ( 'NONE',  ( -0.000000000000000000, -1.000000000000000000, -0.000000000000000000 ) ) ;
#29419 = FACE_OUTER_BOUND ( 'NONE', #96747, .T. ) ;
#29421 = ADVANCED_FACE ( 'NONE', ( #20370 ), #62238, .T. ) ;
#29420 = AXIS2_PLACEMENT_3D ( 'NONE', #49082, #58251, #59561 ) ;
#29422 = EDGE_LOOP ( 'NONE', ( #106292, #53386, #103981, #42420 ) ) ;
#29423 = VECTOR ( 'NONE', #39137, 1000.000000000000000 ) ;
#29424 = ORIENTED_EDGE ( 'NONE', *, *, #99768, .F. ) ;
#29425 = ORIENTED_EDGE ( 'NONE', *, *, #108634, .F. ) ;
#29426 = EDGE_LOOP ( 'NONE', ( #127737, #47956, #18737, #67731 ) ) ;
#29427 = DIRECTION ( 'NONE',  ( 0.000000000000000000, -0.000000000000000000, 1.000000000000000000 ) ) ;
#29428 = CIRCLE ( 'NONE', #31570, 0.09999999999999982514 ) ;
#29429 = CARTESIAN_POINT ( 'NONE',  ( 11.04999999999990834, 12.50000000000000000, -6.776507416713039689 ) ) ;
#29430 = CARTESIAN_POINT ( 'NONE',  ( -5.850000000000019185, 12.50000000000000000, 6.495190528383297135 ) ) ;
#29431 = AXIS2_PLACEMENT_3D ( 'NONE', #35742, #105771, #106406 ) ;
#29433 = EDGE_LOOP ( 'NONE', ( #51187, #112939, #68812, #24899 ) ) ;
#29432 = EDGE_CURVE ( 'NONE', #60192, #13704, #7094, .T. ) ;
#29434 = DIRECTION ( 'NONE',  ( 0.000000000000000000, 0.000000000000000000, -1.000000000000000000 ) ) ;
#29435 = FACE_OUTER_BOUND ( 'NONE', #22637, .T. ) ;
#29436 = DIRECTION ( 'NONE',  ( 0.000000000000000000, -0.000000000000000000, 1.000000000000000000 ) ) ;
#29437 = LINE ( 'NONE', #40564, #31734 ) ;
#29438 = ADVANCED_FACE ( 'NONE', ( #39392 ), #40678, .T. ) ;
#29439 = ORIENTED_EDGE ( 'NONE', *, *, #75564, .F. ) ;
#29440 = CARTESIAN_POINT ( 'NONE',  ( 187.3750000000000000, 8.891194145520236347, 5.444286225454521982E-16 ) ) ;
#29441 = ORIENTED_EDGE ( 'NONE', *, *, #18647, .T. ) ;
#29442 = VERTEX_POINT ( 'NONE', #121773 ) ;
#29443 = FACE_OUTER_BOUND ( 'NONE', #113295, .T. ) ;
#29444 = EDGE_CURVE ( 'NONE', #40822, #100700, #119211, .T. ) ;
#29445 = DIRECTION ( 'NONE',  ( 0.000000000000000000, 0.000000000000000000, 1.000000000000000000 ) ) ;
#29446 = FACE_BOUND ( 'NONE', #78400, .T. ) ;
#29447 = DIRECTION ( 'NONE',  ( 0.000000000000000000, 0.000000000000000000, -1.000000000000000000 ) ) ;
#29448 = FACE_OUTER_BOUND ( 'NONE', #118119, .T. ) ;
#29449 = DIRECTION ( 'NONE',  ( 0.000000000000000000, -0.9999939076577903929, 0.003490651415223739937 ) ) ;
#29450 = CIRCLE ( 'NONE', #35707, 0.06509327318403745899 ) ;
#29452 = EDGE_LOOP ( 'NONE', ( #52049, #70215 ) ) ;
#29451 = AXIS2_PLACEMENT_3D ( 'NONE', #80751, #71556, #70922 ) ;
#29454 = AXIS2_PLACEMENT_3D ( 'NONE', #25827, #95859, #33710 ) ;
#29453 = FACE_OUTER_BOUND ( 'NONE', #37536, .T. ) ;
#29455 = DIRECTION ( 'NONE',  ( -0.000000000000000000, 1.000000000000000000, -0.000000000000000000 ) ) ;
#29456 = LINE ( 'NONE', #110582, #13109 ) ;
#29457 = CARTESIAN_POINT ( 'NONE',  ( 186.5312500006828031, 9.429780353434619030E-16, -7.700000000000000178 ) ) ;
#29458 = EDGE_LOOP ( 'NONE', ( #60417, #81177 ) ) ;
#29459 = DIRECTION ( 'NONE',  ( 0.000000000000000000, 0.000000000000000000, 1.000000000000000000 ) ) ;
#29460 = CIRCLE ( 'NONE', #73357, 0.06509327318403743123 ) ;
#29461 = CARTESIAN_POINT ( 'NONE',  ( 8.949999999999917577, 2.500000000000000000, 6.148780366869520009 ) ) ;
#29462 = ORIENTED_EDGE ( 'NONE', *, *, #52511, .T. ) ;
#29463 = VERTEX_POINT ( 'NONE', #49842 ) ;
#29464 = PLANE ( 'NONE',  #100357 ) ;
#29465 = CARTESIAN_POINT ( 'NONE',  ( 14.34999999999989306, 2.500000000000000000, -2.511473670974877948 ) ) ;
#29466 = FACE_BOUND ( 'NONE', #755, .T. ) ;
#29467 = CARTESIAN_POINT ( 'NONE',  ( 2.299999999999949640, 2.500000000000000000, -0.3464101615137782364 ) ) ;
#29468 = EDGE_CURVE ( 'NONE', #53781, #56111, #25899, .T. ) ;
#29469 = CARTESIAN_POINT ( 'NONE',  ( 4.999999999999935163, 2.500000000000000000, 3.637306695894644726 ) ) ;
#29470 = ORIENTED_EDGE ( 'NONE', *, *, #4632, .T. ) ;
#29471 = FACE_OUTER_BOUND ( 'NONE', #76076, .T. ) ;
#29472 = EDGE_CURVE ( 'NONE', #70518, #42007, #27952, .T. ) ;
#29473 = CARTESIAN_POINT ( 'NONE',  ( 185.0416666666666856, -4.445597072760122614, 7.699999999999998401 ) ) ;
#29474 = EDGE_CURVE ( 'NONE', #2432, #29267, #124092, .T. ) ;
#29475 = ORIENTED_EDGE ( 'NONE', *, *, #83564, .T. ) ;
#29476 = DIRECTION ( 'NONE',  ( -4.274815082592931898E-19, -0.9999939076577903929, -0.003490651415223739937 ) ) ;
#29477 = CARTESIAN_POINT ( 'NONE',  ( 1.899999999999949507, 12.50000000000000000, 4.676537180435972552 ) ) ;
#29478 = VECTOR ( 'NONE', #58808, 1000.000000000000000 ) ;
#29479 = EDGE_CURVE ( 'NONE', #64667, #32289, #34239, .T. ) ;
#29480 = ADVANCED_FACE ( 'NONE', ( #81846 ), #101510, .T. ) ;
#29481 = CARTESIAN_POINT ( 'NONE',  ( 6.649999999999931966, 12.50000000000000000, -5.802370205355749988 ) ) ;
#29482 = EDGE_CURVE ( 'NONE', #105720, #95522, #70118, .T. ) ;
#29483 = DIRECTION ( 'NONE',  ( 0.000000000000000000, -0.9999939076577903929, 0.003490651415223739937 ) ) ;
#29484 = AXIS2_PLACEMENT_3D ( 'NONE', #63180, #122744, #44176 ) ;
#29485 = ORIENTED_EDGE ( 'NONE', *, *, #89886, .T. ) ;
#29486 =( NAMED_UNIT ( * ) PLANE_ANGLE_UNIT ( ) SI_UNIT ( $, .RADIAN. ) );
#29487 = EDGE_CURVE ( 'NONE', #63009, #105656, #119996, .T. ) ;
#29488 = CARTESIAN_POINT ( 'NONE',  ( -9.999999999999969802, 2.500000000000000000, -2.276824562219559311E-15 ) ) ;
#29489 = DIRECTION ( 'NONE',  ( -4.274815082592931898E-19, -0.9999939076577903929, -0.003490651415223739937 ) ) ;
#29490 = CARTESIAN_POINT ( 'NONE',  ( 11.44999999999991047, 2.500000000000000000, -2.511473670974877948 ) ) ;
#29491 = ORIENTED_EDGE ( 'NONE', *, *, #23975, .F. ) ;
#29492 = ORIENTED_EDGE ( 'NONE', *, *, #64625, .F. ) ;
#29493 = CARTESIAN_POINT ( 'NONE',  ( -13.54999999999998828, 2.500000000000000000, -2.511473670974875727 ) ) ;
#29495 = ADVANCED_FACE ( 'NONE', ( #70754 ), #7000, .T. ) ;
#29494 = VECTOR ( 'NONE', #34757, 1000.000000000000000 ) ;
#29496 = ORIENTED_EDGE ( 'NONE', *, *, #88736, .F. ) ;
#29497 = CARTESIAN_POINT ( 'NONE',  ( -11.64999999999999680, 2.500000000000000000, 7.088010851410848190 ) ) ;
#29498 = CIRCLE ( 'NONE', #50415, 0.06509327318403745899 ) ;
#29499 = CARTESIAN_POINT ( 'NONE',  ( 17.50000000000000000, -2.499999999999999556, 3.666666666666668739 ) ) ;
#29500 = CARTESIAN_POINT ( 'NONE',  ( 11.04999999999990834, 2.500000000000000000, -6.841600689897077814 ) ) ;
#29501 = ORIENTED_EDGE ( 'NONE', *, *, #116820, .T. ) ;
#29502 = CARTESIAN_POINT ( 'NONE',  ( 4.199999999999939782, 12.50000000000000000, -2.276824562219559311E-15 ) ) ;
#29503 = FACE_OUTER_BOUND ( 'NONE', #104371, .T. ) ;
#29504 = CARTESIAN_POINT ( 'NONE',  ( -5.400000000000020783, 12.50000000000000000, 0.7579135962115869374 ) ) ;
#29505 = LINE ( 'NONE', #9863, #39102 ) ;
#29506 = DIRECTION ( 'NONE',  ( 0.000000000000000000, 0.000000000000000000, 1.000000000000000000 ) ) ;
#29507 = DIRECTION ( 'NONE',  ( 0.000000000000000000, 1.000000000000000000, 0.000000000000000000 ) ) ;
#29508 = CIRCLE ( 'NONE', #8638, 0.1000000000000002554 ) ;
#29509 = ORIENTED_EDGE ( 'NONE', *, *, #11719, .F. ) ;
#29510 = AXIS2_PLACEMENT_3D ( 'NONE', #10896, #50860, #101892 ) ;
#29511 = EDGE_LOOP ( 'NONE', ( #71415, #94151, #61794, #22815 ) ) ;
#29512 = DIRECTION ( 'NONE',  ( -0.000000000000000000, 1.000000000000000000, -0.000000000000000000 ) ) ;
#29513 = VERTEX_POINT ( 'NONE', #22321 ) ;
#29514 = CARTESIAN_POINT ( 'NONE',  ( 106.3595699872024198, 6.079292664285325998, 4.726105526114997346 ) ) ;
#29516 = EDGE_LOOP ( 'NONE', ( #119860, #75810, #33518, #78928 ) ) ;
#29515 = ORIENTED_EDGE ( 'NONE', *, *, #29432, .T. ) ;
#29517 = EDGE_LOOP ( 'NONE', ( #113054, #41607 ) ) ;
#29518 = PLANE ( 'NONE',  #73040 ) ;
#29519 = CIRCLE ( 'NONE', #125640, 0.1000000000000000472 ) ;
#29520 = CARTESIAN_POINT ( 'NONE',  ( 11.24999999999994316, 2.500000000000000000, 2.065063509461097624 ) ) ;
#29521 = CARTESIAN_POINT ( 'NONE',  ( -5.400000000000020783, 2.500000000000000000, 4.922947341949748257 ) ) ;
#29522 =( NAMED_UNIT ( * ) PLANE_ANGLE_UNIT ( ) SI_UNIT ( $, .RADIAN. ) );
#29523 = CARTESIAN_POINT ( 'NONE',  ( 11.04999999999990834, 12.50000000000000000, -6.841600689897077814 ) ) ;
#29524 = AXIS2_PLACEMENT_3D ( 'NONE', #97874, #70355, #60562 ) ;
#29525 = VECTOR ( 'NONE', #75092, 1000.000000000000000 ) ;
#29526 = DIRECTION ( 'NONE',  ( -0.000000000000000000, 1.000000000000000000, -0.000000000000000000 ) ) ;
#29527 = DIRECTION ( 'NONE',  ( 0.000000000000000000, 0.000000000000000000, 1.000000000000000000 ) ) ;
#29528 = CARTESIAN_POINT ( 'NONE',  ( 6.849999999999927702, 2.500000000000000000, 1.818653347947321475 ) ) ;
#29529 = CARTESIAN_POINT ( 'NONE',  ( 13.29999999999990301, 2.500000000000000000, 4.430127018922196847 ) ) ;
#29530 = DIRECTION ( 'NONE',  ( -0.000000000000000000, 1.000000000000000000, -0.000000000000000000 ) ) ;
#29531 = EDGE_LOOP ( 'NONE', ( #128637, #120270 ) ) ;
#29532 = EDGE_LOOP ( 'NONE', ( #62621, #23387, #66843, #76365 ) ) ;
#29533 = EDGE_CURVE ( 'NONE', #62131, #43475, #2923, .T. ) ;
#29534 = DIRECTION ( 'NONE',  ( 0.000000000000000000, 0.000000000000000000, 1.000000000000000000 ) ) ;
#29535 = ORIENTED_EDGE ( 'NONE', *, *, #18790, .F. ) ;
#29536 = ORIENTED_EDGE ( 'NONE', *, *, #41169, .F. ) ;
#29537 = CARTESIAN_POINT ( 'NONE',  ( 7.499999999999925393, 2.500000000000000000, -0.5928203230275541635 ) ) ;
#29538 = ADVANCED_FACE ( 'NONE', ( #73978 ), #128321, .T. ) ;
#29539 = CARTESIAN_POINT ( 'NONE',  ( -7.700000000000016165, 2.500000000000000000, -4.083716857408426826 ) ) ;
#29540 = DIRECTION ( 'NONE',  ( -4.274815082592931898E-19, -0.9999939076577903929, -0.003490651415223739937 ) ) ;
#29541 = CONICAL_SURFACE ( 'NONE', #10725, 0.1000000000000000472, 0.003490658503988666988 ) ;
#29542 = CARTESIAN_POINT ( 'NONE',  ( 9.999999999999916511, 12.50000000000000000, -0.6928203230275541413 ) ) ;
#29543 = ORIENTED_EDGE ( 'NONE', *, *, #108190, .T. ) ;
#29544 = AXIS2_PLACEMENT_3D ( 'NONE', #108742, #118564, #89113 ) ;
#29545 = CIRCLE ( 'NONE', #10726, 0.1000000000000000472 ) ;
#29546 = ORIENTED_EDGE ( 'NONE', *, *, #107956, .T. ) ;
#29547 = DIRECTION ( 'NONE',  ( 0.000000000000000000, 0.000000000000000000, -1.000000000000000000 ) ) ;
#29548 = VERTEX_POINT ( 'NONE', #32789 ) ;
#29549 = DIRECTION ( 'NONE',  ( 0.000000000000000000, 0.000000000000000000, -1.000000000000000000 ) ) ;
#29550 = ORIENTED_EDGE ( 'NONE', *, *, #94428, .T. ) ;
#29551 = CIRCLE ( 'NONE', #108945, 0.06509327318403745899 ) ;
#29552 = ORIENTED_EDGE ( 'NONE', *, *, #70162, .F. ) ;
#29553 = DIRECTION ( 'NONE',  ( 0.000000000000000000, 0.000000000000000000, -1.000000000000000000 ) ) ;
#29554 = CARTESIAN_POINT ( 'NONE',  ( 81.97061111377811926, -3.937853021331575221, -6.123961096638185886 ) ) ;
#29555 = DIRECTION ( 'NONE',  ( 0.000000000000000000, -0.9999939076577903929, 0.003490651415223739937 ) ) ;
#29556 = DIRECTION ( 'NONE',  ( 0.000000000000000000, -0.000000000000000000, 1.000000000000000000 ) ) ;
#29557 = CARTESIAN_POINT ( 'NONE',  ( 0.8499999999999536815, 12.50000000000000000, 6.430097255199259010 ) ) ;
#29558 = ORIENTED_EDGE ( 'NONE', *, *, #121927, .F. ) ;
#29559 = DIRECTION ( 'NONE',  ( 0.000000000000000000, 0.000000000000000000, 1.000000000000000000 ) ) ;
#29560 = FACE_OUTER_BOUND ( 'NONE', #4705, .T. ) ;
#29561 = DIRECTION ( 'NONE',  ( 0.000000000000000000, 0.000000000000000000, 1.000000000000000000 ) ) ;
#29562 = DIRECTION ( 'NONE',  ( 0.000000000000000000, 0.000000000000000000, -1.000000000000000000 ) ) ;
#29563 = CARTESIAN_POINT ( 'NONE',  ( -8.950000000000006395, 2.500000000000000000, 6.841600689897072485 ) ) ;
#29564 = ADVANCED_FACE ( 'NONE', ( #55622 ), #24234, .T. ) ;
#29565 = EDGE_LOOP ( 'NONE', ( #115627, #73761, #80403, #23448 ) ) ;
#29566 = EDGE_LOOP ( 'NONE', ( #12908, #87989 ) ) ;
#29567 = DIRECTION ( 'NONE',  ( -4.274815082592931898E-19, -0.9999939076577903929, -0.003490651415223739937 ) ) ;
#29568 = ORIENTED_EDGE ( 'NONE', *, *, #14711, .F. ) ;
#29569 = CARTESIAN_POINT ( 'NONE',  ( 17.48308156489508747, -2.102418598455126020, 4.293689242909404236 ) ) ;
#29570 = AXIS2_PLACEMENT_3D ( 'NONE', #12957, #73191, #24094 ) ;
#29572 = EDGE_CURVE ( 'NONE', #88750, #30265, #54971, .T. ) ;
#29571 = DIRECTION ( 'NONE',  ( -4.274815082592931898E-19, -0.9999939076577903929, -0.003490651415223739937 ) ) ;
#29574 = ORIENTED_EDGE ( 'NONE', *, *, #126983, .F. ) ;
#29573 = EDGE_CURVE ( 'NONE', #32088, #7687, #80194, .T. ) ;
#29575 = LINE ( 'NONE', #111336, #57840 ) ;
#29576 = DIRECTION ( 'NONE',  ( 0.000000000000000000, 0.000000000000000000, 1.000000000000000000 ) ) ;
#29577 = DIRECTION ( 'NONE',  ( 0.000000000000000000, 1.000000000000000000, 0.000000000000000000 ) ) ;
#29578 = ADVANCED_FACE ( 'NONE', ( #2636 ), #63557, .T. ) ;
#29579 = DIRECTION ( 'NONE',  ( 0.000000000000000000, -0.9999939076577903929, 0.003490651415223739937 ) ) ;
#29580 = AXIS2_PLACEMENT_3D ( 'NONE', #92205, #2525, #122338 ) ;
#29581 = AXIS2_PLACEMENT_3D ( 'NONE', #48379, #50315, #18903 ) ;
#29582 = DIRECTION ( 'NONE',  ( 0.000000000000000000, 0.000000000000000000, 1.000000000000000000 ) ) ;
#29583 = EDGE_CURVE ( 'NONE', #86749, #32777, #22950, .T. ) ;
#29584 = VERTEX_POINT ( 'NONE', #82525 ) ;
#29585 = ADVANCED_FACE ( 'NONE', ( #122441 ), #44689, .T. ) ;
#29586 = DIRECTION ( 'NONE',  ( 0.000000000000000000, -0.000000000000000000, 1.000000000000000000 ) ) ;
#29587 = DIRECTION ( 'NONE',  ( 0.000000000000000000, 0.000000000000000000, 1.000000000000000000 ) ) ;
#29588 = CARTESIAN_POINT ( 'NONE',  ( -4.294665249841745289E-14, 2.500000000000000000, 4.922947341949748257 ) ) ;
#29589 = CIRCLE ( 'NONE', #108994, 0.06509327318403745899 ) ;
#29590 = CIRCLE ( 'NONE', #14888, 0.1000000000000002554 ) ;
#29591 = ORIENTED_EDGE ( 'NONE', *, *, #3601, .F. ) ;
#29592 = DIRECTION ( 'NONE',  ( 0.000000000000000000, 0.000000000000000000, 1.000000000000000000 ) ) ;
#29593 = AXIS2_PLACEMENT_3D ( 'NONE', #111685, #10869, #50828 ) ;
#29594 = ORIENTED_EDGE ( 'NONE', *, *, #123882, .T. ) ;
#29595 = DIRECTION ( 'NONE',  ( 0.000000000000000000, -0.9999939076577903929, 0.003490651415223739937 ) ) ;
#29596 = PLANE ( 'NONE',  #119815 ) ;
#29597 = VECTOR ( 'NONE', #89341, 1000.000000000000000 ) ;
#29598 = DIRECTION ( 'NONE',  ( 0.000000000000000000, 1.000000000000000000, 0.000000000000000000 ) ) ;
#29599 = ORIENTED_EDGE ( 'NONE', *, *, #120436, .F. ) ;
#29600 = DIRECTION ( 'NONE',  ( 0.000000000000000000, 1.000000000000000000, 0.000000000000000000 ) ) ;
#29601 = DIRECTION ( 'NONE',  ( -0.000000000000000000, 1.000000000000000000, -0.000000000000000000 ) ) ;
#29602 = CIRCLE ( 'NONE', #77620, 0.06509327318403745899 ) ;
#29603 = VECTOR ( 'NONE', #103104, 1000.000000000000000 ) ;
#29604 = ORIENTED_EDGE ( 'NONE', *, *, #58155, .T. ) ;
#29605 = DIRECTION ( 'NONE',  ( 0.000000000000000000, 0.000000000000000000, 1.000000000000000000 ) ) ;
#29606 = ORIENTED_EDGE ( 'NONE', *, *, #59743, .F. ) ;
#29607 = DIRECTION ( 'NONE',  ( 0.000000000000000000, 0.000000000000000000, 1.000000000000000000 ) ) ;
#29608 = ADVANCED_FACE ( 'NONE', ( #13099 ), #48900, .T. ) ;
#29609 = EDGE_LOOP ( 'NONE', ( #42181, #65434 ) ) ;
#29610 = DIRECTION ( 'NONE',  ( 0.000000000000000000, 0.000000000000000000, 1.000000000000000000 ) ) ;
#29611 = CARTESIAN_POINT ( 'NONE',  ( 0.1999999999999562961, 2.500000000000000000, 4.676537180435972552 ) ) ;
#29612 = ORIENTED_EDGE ( 'NONE', *, *, #8514, .F. ) ;
#29613 = ORIENTED_EDGE ( 'NONE', *, *, #110149, .T. ) ;
#29614 = DIRECTION ( 'NONE',  ( 0.000000000000000000, 1.000000000000000000, 0.000000000000000000 ) ) ;
#29615 = LINE ( 'NONE', #49284, #420 ) ;
#29616 = VERTEX_POINT ( 'NONE', #104084 ) ;
#29617 = ADVANCED_FACE ( 'NONE', ( #54334 ), #92983, .T. ) ;
#29618 = DIRECTION ( 'NONE',  ( 0.000000000000000000, 0.000000000000000000, -1.000000000000000000 ) ) ;
#29619 = CARTESIAN_POINT ( 'NONE',  ( 186.9843750003414016, -8.734944146203032389, -1.604583208406767949E-15 ) ) ;
#29620 = DIRECTION ( 'NONE',  ( -4.274815082592931898E-19, -0.9999939076577903929, -0.003490651415223739937 ) ) ;
#29621 = AXIS2_PLACEMENT_3D ( 'NONE', #59584, #9805, #89659 ) ;
#29622 = CARTESIAN_POINT ( 'NONE',  ( 0.8499999999999557909, 2.500000000000000000, -7.188010851410854052 ) ) ;
#29623 = DIRECTION ( 'NONE',  ( 0.000000000000000000, -0.000000000000000000, 1.000000000000000000 ) ) ;
#29624 = AXIS2_PLACEMENT_3D ( 'NONE', #54815, #77674, #125494 ) ;
#29625 = EDGE_CURVE ( 'NONE', #41344, #67957, #3303, .T. ) ;
#29626 = CONICAL_SURFACE ( 'NONE', #127825, 0.1000000000000002554, 0.003490658503988666988 ) ;
#29627 = DIRECTION ( 'NONE',  ( -0.000000000000000000, 1.000000000000000000, -0.000000000000000000 ) ) ;
#29628 = CARTESIAN_POINT ( 'NONE',  ( 5.449999999999936229, 2.500000000000000000, 6.495190528383297135 ) ) ;
#29629 = EDGE_CURVE ( 'NONE', #127552, #54932, #99069, .T. ) ;
#29630 = EDGE_CURVE ( 'NONE', #76614, #45205, #17468, .T. ) ;
#29631 = CIRCLE ( 'NONE', #52613, 0.06509327318403741736 ) ;
#29632 = ORIENTED_EDGE ( 'NONE', *, *, #75925, .T. ) ;
#29634 = EDGE_LOOP ( 'NONE', ( #40156, #80487 ) ) ;
#29633 = AXIS2_PLACEMENT_3D ( 'NONE', #93268, #6611, #66206 ) ;
#29636 = ORIENTED_EDGE ( 'NONE', *, *, #56586, .T. ) ;
#29635 = EDGE_CURVE ( 'NONE', #44929, #61864, #76079, .T. ) ;
#29637 = ORIENTED_EDGE ( 'NONE', *, *, #59327, .T. ) ;
#29638 = DIRECTION ( 'NONE',  ( 0.000000000000000000, 1.000000000000000000, 0.000000000000000000 ) ) ;
#29639 = DIRECTION ( 'NONE',  ( 0.000000000000000000, 0.000000000000000000, 1.000000000000000000 ) ) ;
#29640 = AXIS2_PLACEMENT_3D ( 'NONE', #104501, #107070, #78291 ) ;
#29641 = CARTESIAN_POINT ( 'NONE',  ( -5.650000000000019895, 2.500000000000000000, 2.511473670974873507 ) ) ;
#29643 = ORIENTED_EDGE ( 'NONE', *, *, #6028, .F. ) ;
#29642 = CIRCLE ( 'NONE', #125764, 0.1000000000000000472 ) ;
#29644 = FACE_BOUND ( 'NONE', #129282, .T. ) ;
#29645 = VERTEX_POINT ( 'NONE', #73319 ) ;
#29646 = CARTESIAN_POINT ( 'NONE',  ( 6.849999999999927702, 12.50000000000000000, 1.753560074763284016 ) ) ;
#29647 = CARTESIAN_POINT ( 'NONE',  ( -9.350000000000006750, 2.500000000000000000, 1.818653347947321475 ) ) ;
#29648 = EDGE_CURVE ( 'NONE', #53411, #63511, #42647, .T. ) ;
#29649 = AXIS2_PLACEMENT_3D ( 'NONE', #25260, #34476, #74384 ) ;
#29650 = EDGE_CURVE ( 'NONE', #117332, #51834, #59375, .T. ) ;
#29651 = CARTESIAN_POINT ( 'NONE',  ( 8.949999999999921130, 2.500000000000000000, 1.918653347947321564 ) ) ;
#29652 = ADVANCED_FACE ( 'NONE', ( #64789 ), #4949, .T. ) ;
#29653 = DIRECTION ( 'NONE',  ( 0.000000000000000000, 1.000000000000000000, 0.000000000000000000 ) ) ;
#29654 = DIRECTION ( 'NONE',  ( 0.000000000000000000, 0.000000000000000000, -1.000000000000000000 ) ) ;
#29655 = DIRECTION ( 'NONE',  ( 0.000000000000000000, 0.000000000000000000, 1.000000000000000000 ) ) ;
#29656 = FACE_OUTER_BOUND ( 'NONE', #100523, .T. ) ;
#29657 = CARTESIAN_POINT ( 'NONE',  ( 8.149999999999920419, 2.500000000000000000, 6.148780366869520897 ) ) ;
#29658 = CARTESIAN_POINT ( 'NONE',  ( -12.89999999999999147, 2.500000000000000000, 3.537306695894645081 ) ) ;
#29659 = CARTESIAN_POINT ( 'NONE',  ( 7.899999999999924860, 12.50000000000000000, -4.265033745738164406 ) ) ;
#29660 = ORIENTED_EDGE ( 'NONE', *, *, #46707, .F. ) ;
#29661 = ORIENTED_EDGE ( 'NONE', *, *, #3336, .T. ) ;
#29662 = ORIENTED_EDGE ( 'NONE', *, *, #52156, .T. ) ;
#29663 = ORIENTED_EDGE ( 'NONE', *, *, #25565, .T. ) ;
#29664 = FACE_OUTER_BOUND ( 'NONE', #49914, .T. ) ;
#29665 = DIRECTION ( 'NONE',  ( 0.000000000000000000, 0.000000000000000000, 1.000000000000000000 ) ) ;
#29667 = ORIENTED_EDGE ( 'NONE', *, *, #98583, .T. ) ;
#29666 = ORIENTED_EDGE ( 'NONE', *, *, #74680, .T. ) ;
#29668 = VERTEX_POINT ( 'NONE', #125637 ) ;
#29669 = DIRECTION ( 'NONE',  ( -0.000000000000000000, 1.000000000000000000, -0.000000000000000000 ) ) ;
#29670 = AXIS2_PLACEMENT_3D ( 'NONE', #102497, #52115, #2336 ) ;
#29671 = CIRCLE ( 'NONE', #52641, 0.06509327318403745899 ) ;
#29672 = PLANE ( 'NONE',  #101106 ) ;
#29673 = FACE_OUTER_BOUND ( 'NONE', #77778, .T. ) ;
#29674 = DIRECTION ( 'NONE',  ( 0.000000000000000000, 0.000000000000000000, 1.000000000000000000 ) ) ;
#29675 = DIRECTION ( 'NONE',  ( 0.000000000000000000, -0.000000000000000000, 1.000000000000000000 ) ) ;
#29676 = CARTESIAN_POINT ( 'NONE',  ( -4.250072516143177381E-14, 2.500000000000000000, -3.537306695894649966 ) ) ;
#29677 = DIRECTION ( 'NONE',  ( 0.000000000000000000, -0.000000000000000000, 1.000000000000000000 ) ) ;
#29678 = ORIENTED_EDGE ( 'NONE', *, *, #107155, .F. ) ;
#29679 = CIRCLE ( 'NONE', #123739, 0.1000000000000002554 ) ;
#29680 = AXIS2_PLACEMENT_3D ( 'NONE', #27742, #38232, #87306 ) ;
#29681 = DIRECTION ( 'NONE',  ( 0.000000000000000000, -0.000000000000000000, 1.000000000000000000 ) ) ;
#29682 = ORIENTED_EDGE ( 'NONE', *, *, #59128, .T. ) ;
#29683 = CONICAL_SURFACE ( 'NONE', #59017, 0.1000000000000000056, 0.003490658503988666988 ) ;
#29684 = ORIENTED_EDGE ( 'NONE', *, *, #106153, .T. ) ;
#29685 = AXIS2_PLACEMENT_3D ( 'NONE', #73657, #114874, #3641 ) ;
#29686 = EDGE_CURVE ( 'NONE', #7993, #1900, #5860, .T. ) ;
#29687 = ORIENTED_EDGE ( 'NONE', *, *, #11465, .T. ) ;
#29688 = CARTESIAN_POINT ( 'NONE',  ( -11.44999999999999751, 2.500000000000000000, -6.941600689897074794 ) ) ;
#29689 = ORIENTED_EDGE ( 'NONE', *, *, #78158, .T. ) ;
#29690 = EDGE_LOOP ( 'NONE', ( #128935, #86489, #45861, #32585 ) ) ;
#29691 = AXIS2_PLACEMENT_3D ( 'NONE', #117311, #67591, #16550 ) ;
#29692 = EDGE_CURVE ( 'NONE', #57270, #80732, #47110, .T. ) ;
#29693 = DIRECTION ( 'NONE',  ( 0.000000000000000000, 0.000000000000000000, -1.000000000000000000 ) ) ;
#29694 = CARTESIAN_POINT ( 'NONE',  ( -9.350000000000006750, 12.50000000000000000, -1.818653347947325916 ) ) ;
#29695 = DIRECTION ( 'NONE',  ( 0.000000000000000000, -0.9999939076577903929, 0.003490651415223739937 ) ) ;
#29696 = AXIS2_PLACEMENT_3D ( 'NONE', #108169, #9981, #70194 ) ;
#29697 = CIRCLE ( 'NONE', #10878, 0.1000000000000000472 ) ;
#29698 = DIRECTION ( 'NONE',  ( -0.000000000000000000, 1.000000000000000000, -0.000000000000000000 ) ) ;
#29699 = CIRCLE ( 'NONE', #2572, 0.09999999999999982514 ) ;
#29700 = ORIENTED_EDGE ( 'NONE', *, *, #70432, .F. ) ;
#29701 = LINE ( 'NONE', #128576, #42826 ) ;
#29702 = ORIENTED_EDGE ( 'NONE', *, *, #105961, .F. ) ;
#29703 = FACE_OUTER_BOUND ( 'NONE', #76273, .T. ) ;
#29704 = EDGE_LOOP ( 'NONE', ( #122495, #13515, #119140, #33190 ) ) ;
#29705 = DIRECTION ( 'NONE',  ( -0.000000000000000000, 1.000000000000000000, -0.000000000000000000 ) ) ;
#29706 = LINE ( 'NONE', #40180, #44110 ) ;
#29707 = ORIENTED_EDGE ( 'NONE', *, *, #127512, .F. ) ;
#29708 = CARTESIAN_POINT ( 'NONE',  ( -3.750000000000027534, 12.50000000000000000, -1.472243186433550122 ) ) ;
#29709 = PLANE ( 'NONE',  #52017 ) ;
#29710 = VERTEX_POINT ( 'NONE', #7149 ) ;
#29711 = DIRECTION ( 'NONE',  ( 0.000000000000000000, 0.000000000000000000, -1.000000000000000000 ) ) ;
#29712 = ORIENTED_EDGE ( 'NONE', *, *, #110607, .F. ) ;
#29713 = VERTEX_POINT ( 'NONE', #126949 ) ;
#29714 = FACE_OUTER_BOUND ( 'NONE', #6044, .T. ) ;
#29715 = CARTESIAN_POINT ( 'NONE',  ( 6.649999999999930189, 2.500000000000000000, -2.857883832488653741 ) ) ;
#29716 = CARTESIAN_POINT ( 'NONE',  ( 184.5052083336747444, -6.551208109652278289, 3.782341765624995134 ) ) ;
#29717 = CARTESIAN_POINT ( 'NONE',  ( 10.39999999999991154, 2.500000000000000000, 5.022947341949748790 ) ) ;
#29718 = DIRECTION ( 'NONE',  ( 0.000000000000000000, 1.000000000000000000, 0.000000000000000000 ) ) ;
#29719 = VERTEX_POINT ( 'NONE', #45814 ) ;
#29720 = LINE ( 'NONE', #38266, #88485 ) ;
#29721 = CONICAL_SURFACE ( 'NONE', #71577, 0.09999999999999982514, 0.003490658503988666988 ) ;
#29722 = AXIS2_PLACEMENT_3D ( 'NONE', #121138, #1998, #92315 ) ;
#29723 = ORIENTED_EDGE ( 'NONE', *, *, #6392, .F. ) ;
#29724 = DIRECTION ( 'NONE',  ( 0.000000000000000000, -0.000000000000000000, 1.000000000000000000 ) ) ;
#29726 = EDGE_CURVE ( 'NONE', #52060, #2207, #48382, .T. ) ;
#29725 = DIRECTION ( 'NONE',  ( 0.000000000000000000, 0.000000000000000000, -1.000000000000000000 ) ) ;
#29727 = CONICAL_SURFACE ( 'NONE', #79902, 0.09999999999999982514, 0.003490658503988666988 ) ;
#29728 = CIRCLE ( 'NONE', #25508, 2.000000000000000000 ) ;
#29729 = AXIS2_PLACEMENT_3D ( 'NONE', #112596, #123056, #22296 ) ;
#29730 = VECTOR ( 'NONE', #66359, 1000.000000000000000 ) ;
#29731 = CIRCLE ( 'NONE', #102875, 4.000000000000000000 ) ;
#29732 = EDGE_CURVE ( 'NONE', #63696, #109777, #78144, .T. ) ;
#29733 = CARTESIAN_POINT ( 'NONE',  ( -4.600000000000025402, 2.500000000000000000, -0.1000000000000023925 ) ) ;
#29734 = CARTESIAN_POINT ( 'NONE',  ( -12.89999999999999325, 12.50000000000000000, -3.637306695894647390 ) ) ;
#29735 = DIRECTION ( 'NONE',  ( 0.000000000000000000, 0.000000000000000000, 1.000000000000000000 ) ) ;
#29736 = DIRECTION ( 'NONE',  ( 1.000000000000000000, 0.000000000000000000, 0.000000000000000000 ) ) ;
#29737 = EDGE_CURVE ( 'NONE', #68264, #57867, #21701, .T. ) ;
#29738 = CARTESIAN_POINT ( 'NONE',  ( 15.39999999999989200, 2.500000000000000000, 0.6928203230275494784 ) ) ;
#29739 = VERTEX_POINT ( 'NONE', #106017 ) ;
#29740 = AXIS2_PLACEMENT_3D ( 'NONE', #115012, #6332, #126136 ) ;
#29741 = DIRECTION ( 'NONE',  ( 0.000000000000000000, 1.000000000000000000, 0.000000000000000000 ) ) ;
#29742 = DIRECTION ( 'NONE',  ( -0.000000000000000000, 1.000000000000000000, 1.846105847067148022E-16 ) ) ;
#29743 = CARTESIAN_POINT ( 'NONE',  ( -4.800000000000022915, 12.50000000000000000, -0.3464101615137783474 ) ) ;
#29744 = ADVANCED_FACE ( 'NONE', ( #116463 ), #44784, .T. ) ;
#29745 = EDGE_CURVE ( 'NONE', #14967, #81450, #111577, .T. ) ;
#29746 = EDGE_CURVE ( 'NONE', #27555, #72458, #85716, .T. ) ;
#29747 = ORIENTED_EDGE ( 'NONE', *, *, #71294, .F. ) ;
#29748 = DIRECTION ( 'NONE',  ( 0.000000000000000000, 0.000000000000000000, 1.000000000000000000 ) ) ;
#29749 = ORIENTED_EDGE ( 'NONE', *, *, #6487, .F. ) ;
#29750 = ORIENTED_EDGE ( 'NONE', *, *, #107036, .T. ) ;
#29751 = DIRECTION ( 'NONE',  ( -4.274815082592931898E-19, -0.9999939076577903929, -0.003490651415223739937 ) ) ;
#29752 = VERTEX_POINT ( 'NONE', #18906 ) ;
#29753 = FACE_OUTER_BOUND ( 'NONE', #82929, .T. ) ;
#29754 = DIRECTION ( 'NONE',  ( 0.000000000000000000, 0.000000000000000000, 1.000000000000000000 ) ) ;
#29755 = CIRCLE ( 'NONE', #115504, 0.06509327318403745899 ) ;
#29756 = ORIENTED_EDGE ( 'NONE', *, *, #99182, .T. ) ;
#29757 = DIRECTION ( 'NONE',  ( -4.274815082592931898E-19, -0.9999939076577903929, -0.003490651415223739937 ) ) ;
#29759 = ORIENTED_EDGE ( 'NONE', *, *, #15762, .F. ) ;
#29758 = DIRECTION ( 'NONE',  ( -4.274815082592931898E-19, -0.9999939076577903929, -0.003490651415223739937 ) ) ;
#29760 = CARTESIAN_POINT ( 'NONE',  ( -6.850000000000013856, 12.50000000000000000, 1.753560074763284016 ) ) ;
#29761 = VECTOR ( 'NONE', #26545, 1000.000000000000000 ) ;
#29762 = ORIENTED_EDGE ( 'NONE', *, *, #29246, .T. ) ;
#29763 = CIRCLE ( 'NONE', #25540, 0.06509327318403745899 ) ;
#29764 = AXIS2_PLACEMENT_3D ( 'NONE', #50570, #81339, #121255 ) ;
#29765 = CIRCLE ( 'NONE', #36033, 0.06509327318403745899 ) ;
#29766 = VERTEX_POINT ( 'NONE', #108590 ) ;
#29767 = EDGE_LOOP ( 'NONE', ( #111938, #82639, #83200, #109096 ) ) ;
#29768 = DIRECTION ( 'NONE',  ( -0.000000000000000000, -1.000000000000000000, -0.000000000000000000 ) ) ;
#29769 = CARTESIAN_POINT ( 'NONE',  ( 183.8645833340161175, -6.668395609140180369, 3.849999999999994760 ) ) ;
#29770 = DIRECTION ( 'NONE',  ( 0.000000000000000000, 0.000000000000000000, -1.000000000000000000 ) ) ;
#29771 = FACE_BOUND ( 'NONE', #17621, .T. ) ;
#29772 = ORIENTED_EDGE ( 'NONE', *, *, #50141, .T. ) ;
#29773 = CARTESIAN_POINT ( 'NONE',  ( 12.29999999999990301, 12.50000000000000000, -0.3464101615137782364 ) ) ;
#29774 = CARTESIAN_POINT ( 'NONE',  ( 3.549999999999943867, 2.500000000000000000, -6.248780366869526759 ) ) ;
#29775 = CIRCLE ( 'NONE', #4606, 0.1000000000000002554 ) ;
#29776 = ORIENTED_EDGE ( 'NONE', *, *, #94585, .T. ) ;
#29777 = AXIS2_PLACEMENT_3D ( 'NONE', #80660, #49275, #121859 ) ;
#29778 = CARTESIAN_POINT ( 'NONE',  ( -0.4500000000000397571, 12.50000000000000000, -6.495190528383302464 ) ) ;
#29779 = LINE ( 'NONE', #127979, #3156 ) ;
#29780 = AXIS2_PLACEMENT_3D ( 'NONE', #113223, #3284, #12444 ) ;
#29781 = CONICAL_SURFACE ( 'NONE', #40255, 0.1000000000000002554, 0.003490658503988666988 ) ;
#29782 = AXIS2_PLACEMENT_3D ( 'NONE', #94363, #125128, #15800 ) ;
#29784 = EDGE_CURVE ( 'NONE', #35476, #117024, #127589, .T. ) ;
#29783 = CARTESIAN_POINT ( 'NONE',  ( -5.000000000000023093, 12.50000000000000000, 5.022947341949748790 ) ) ;
#29785 = DIRECTION ( 'NONE',  ( 0.000000000000000000, 1.000000000000000000, 0.000000000000000000 ) ) ;
#29786 = DIRECTION ( 'NONE',  ( 0.000000000000000000, 0.000000000000000000, -1.000000000000000000 ) ) ;
#29787 = EDGE_CURVE ( 'NONE', #78590, #12380, #82447, .T. ) ;
#29788 = CARTESIAN_POINT ( 'NONE',  ( -2.100000000000033396, 12.50000000000000000, -0.6928203230275542523 ) ) ;
#29789 = CARTESIAN_POINT ( 'NONE',  ( -14.34999999999998543, 12.50000000000000000, -2.511473670974875727 ) ) ;
#29790 = EDGE_CURVE ( 'NONE', #60953, #22036, #18271, .T. ) ;
#29791 = VERTEX_POINT ( 'NONE', #38588 ) ;
#29792 = VECTOR ( 'NONE', #111908, 1000.000000000000000 ) ;
#29793 = ORIENTED_EDGE ( 'NONE', *, *, #32603, .T. ) ;
#29794 = ORIENTED_EDGE ( 'NONE', *, *, #37934, .F. ) ;
#29795 = EDGE_LOOP ( 'NONE', ( #110166, #31548 ) ) ;
#29796 = ORIENTED_EDGE ( 'NONE', *, *, #84103, .F. ) ;
#29797 = PLANE ( 'NONE',  #104847 ) ;
#29798 = EDGE_CURVE ( 'NONE', #99999, #80146, #61514, .T. ) ;
#29799 = DIRECTION ( 'NONE',  ( -4.274815082592931898E-19, -0.9999939076577903929, -0.003490651415223739937 ) ) ;
#29801 = ADVANCED_FACE ( 'NONE', ( #26169 ), #95553, .T. ) ;
#29800 = ORIENTED_EDGE ( 'NONE', *, *, #127484, .T. ) ;
#29802 = FACE_BOUND ( 'NONE', #94651, .T. ) ;
#29803 = CARTESIAN_POINT ( 'NONE',  ( 8.149999999999923972, 2.500000000000000000, 1.918653347947321564 ) ) ;
#29804 = ADVANCED_FACE ( 'NONE', ( #47747 ), #17563, .T. ) ;
#29805 = EDGE_CURVE ( 'NONE', #89331, #42654, #56261, .T. ) ;
#29806 = EDGE_CURVE ( 'NONE', #7162, #107859, #28753, .T. ) ;
#29807 = DIRECTION ( 'NONE',  ( 0.000000000000000000, 0.000000000000000000, -1.000000000000000000 ) ) ;
#29808 = DIRECTION ( 'NONE',  ( 0.000000000000000000, 0.000000000000000000, 1.000000000000000000 ) ) ;
#29809 = LINE ( 'NONE', #81489, #37036 ) ;
#29810 = CARTESIAN_POINT ( 'NONE',  ( 2.099999999999950351, 12.50000000000000000, -2.276824562219559311E-15 ) ) ;
#29811 = AXIS2_PLACEMENT_3D ( 'NONE', #89763, #121790, #72076 ) ;
#29812 = DIRECTION ( 'NONE',  ( -0.000000000000000000, 1.000000000000000000, -0.000000000000000000 ) ) ;
#29813 = ORIENTED_EDGE ( 'NONE', *, *, #32810, .T. ) ;
#29814 = EDGE_CURVE ( 'NONE', #34970, #39517, #126340, .T. ) ;
#29815 = ORIENTED_EDGE ( 'NONE', *, *, #85425, .T. ) ;
#29816 = ORIENTED_EDGE ( 'NONE', *, *, #63486, .F. ) ;
#29817 = VERTEX_POINT ( 'NONE', #36651 ) ;
#29818 = ORIENTED_EDGE ( 'NONE', *, *, #10867, .F. ) ;
#29819 = AXIS2_PLACEMENT_3D ( 'NONE', #124971, #5815, #76518 ) ;
#29820 = CARTESIAN_POINT ( 'NONE',  ( 13.39053294304986785, 2.500000000000000888, 7.037281287790724704 ) ) ;
#29821 = DIRECTION ( 'NONE',  ( -0.000000000000000000, 1.000000000000000000, -0.000000000000000000 ) ) ;
#29822 = EDGE_LOOP ( 'NONE', ( #70313, #56686 ) ) ;
#29823 = DIRECTION ( 'NONE',  ( 0.000000000000000000, 0.000000000000000000, 1.000000000000000000 ) ) ;
#29824 = DIRECTION ( 'NONE',  ( 0.000000000000000000, 0.000000000000000000, 1.000000000000000000 ) ) ;
#29825 = CONICAL_SURFACE ( 'NONE', #61122, 0.1000000000000000472, 0.003490658503988666988 ) ;
#29826 = VECTOR ( 'NONE', #11034, 1000.000000000000000 ) ;
#29827 = CIRCLE ( 'NONE', #113443, 0.09999999999999982514 ) ;
#29828 = FACE_OUTER_BOUND ( 'NONE', #108215, .T. ) ;
#29829 = CARTESIAN_POINT ( 'NONE',  ( 185.1927083336747160, 6.551208109652275624, -3.782341765624998686 ) ) ;
#29830 = FACE_OUTER_BOUND ( 'NONE', #43733, .T. ) ;
#29831 = PLANE ( 'NONE',  #86468 ) ;
#29832 = AXIS2_PLACEMENT_3D ( 'NONE', #96778, #16907, #42740 ) ;
#29833 = AXIS2_PLACEMENT_3D ( 'NONE', #41785, #122265, #101974 ) ;
#29834 = DIRECTION ( 'NONE',  ( 0.000000000000000000, 1.000000000000000000, 0.000000000000000000 ) ) ;
#29835 = ORIENTED_EDGE ( 'NONE', *, *, #118396, .T. ) ;
#29836 = DIRECTION ( 'NONE',  ( 0.000000000000000000, 1.000000000000000000, 0.000000000000000000 ) ) ;
#29837 = AXIS2_PLACEMENT_3D ( 'NONE', #79618, #87486, #98590 ) ;
#29838 = EDGE_LOOP ( 'NONE', ( #91463, #23219, #96410, #12105 ) ) ;
#29839 = ORIENTED_EDGE ( 'NONE', *, *, #11476, .F. ) ;
#29840 = DIRECTION ( 'NONE',  ( -4.274815082592931898E-19, -0.9999939076577903929, -0.003490651415223739937 ) ) ;
#29841 = DIRECTION ( 'NONE',  ( 0.000000000000000000, 1.000000000000000000, 0.000000000000000000 ) ) ;
#29842 = DIRECTION ( 'NONE',  ( 0.000000000000000000, 1.000000000000000000, 0.000000000000000000 ) ) ;
#29843 = ORIENTED_EDGE ( 'NONE', *, *, #57091, .F. ) ;
#29844 = ORIENTED_EDGE ( 'NONE', *, *, #109467, .T. ) ;
#29845 = CIRCLE ( 'NONE', #46551, 0.09999999999999982514 ) ;
#29846 = CARTESIAN_POINT ( 'NONE',  ( 1.049999999999954525, 2.500000000000000000, 1.718653347947321386 ) ) ;
#29847 = EDGE_CURVE ( 'NONE', #76431, #64157, #128904, .T. ) ;
#29848 = CARTESIAN_POINT ( 'NONE',  ( -2.100000000000033840, 12.50000000000000000, 5.022947341949748790 ) ) ;
#29849 = DIRECTION ( 'NONE',  ( 0.000000000000000000, 0.000000000000000000, -1.000000000000000000 ) ) ;
#29850 = DIRECTION ( 'NONE',  ( 0.000000000000000000, 1.000000000000000000, 0.000000000000000000 ) ) ;
#29851 = VERTEX_POINT ( 'NONE', #119687 ) ;
#29852 = CARTESIAN_POINT ( 'NONE',  ( -10.65000000000000391, 12.50000000000000000, -2.446380397790836270 ) ) ;
#29854 = EDGE_LOOP ( 'NONE', ( #1737, #1658, #71670, #1663 ) ) ;
#29853 = CONICAL_SURFACE ( 'NONE', #109259, 0.1000000000000002554, 0.003490658503988666988 ) ;
#29855 = DIRECTION ( 'NONE',  ( 0.000000000000000000, 1.000000000000000000, 0.000000000000000000 ) ) ;
#29856 = AXIS2_PLACEMENT_3D ( 'NONE', #53780, #83258, #110761 ) ;
#29857 = VERTEX_POINT ( 'NONE', #120355 ) ;
#29858 = LINE ( 'NONE', #109715, #100573 ) ;
#29859 = DIRECTION ( 'NONE',  ( 0.000000000000000000, -0.000000000000000000, 1.000000000000000000 ) ) ;
#29860 = PLANE ( 'NONE',  #101273 ) ;
#29862 = CIRCLE ( 'NONE', #25734, 0.1000000000000002554 ) ;
#29861 = FACE_OUTER_BOUND ( 'NONE', #94594, .T. ) ;
#29863 = ORIENTED_EDGE ( 'NONE', *, *, #95191, .T. ) ;
#29864 = AXIS2_PLACEMENT_3D ( 'NONE', #25659, #34217, #13900 ) ;
#29865 = CIRCLE ( 'NONE', #11060, 0.09999999999999982514 ) ;
#29866 = CARTESIAN_POINT ( 'NONE',  ( -1.050000000000038680, 2.500000000000000000, 2.511473670974873507 ) ) ;
#29867 = CIRCLE ( 'NONE', #6846, 0.06509327318403745899 ) ;
#29868 = ORIENTED_EDGE ( 'NONE', *, *, #51221, .F. ) ;
#29869 = VERTEX_POINT ( 'NONE', #98756 ) ;
#29870 = CARTESIAN_POINT ( 'NONE',  ( 8.349999999999923261, 2.500000000000000000, -7.188010851410854052 ) ) ;
#29871 = DIRECTION ( 'NONE',  ( -0.000000000000000000, -1.000000000000000000, -0.000000000000000000 ) ) ;
#29872 = PLANE ( 'NONE',  #78344 ) ;
#29873 = SURFACE_STYLE_USAGE ( .BOTH. , #20065 ) ;
#29874 = CIRCLE ( 'NONE', #19391, 0.1000000000000002554 ) ;
#29875 = DIRECTION ( 'NONE',  ( 0.000000000000000000, 0.000000000000000000, 1.000000000000000000 ) ) ;
#29876 = CARTESIAN_POINT ( 'NONE',  ( -1.650000000000035216, 2.500000000000000000, -5.802370205355749988 ) ) ;
#29877 = AXIS2_PLACEMENT_3D ( 'NONE', #102230, #32861, #82595 ) ;
#29878 = DIRECTION ( 'NONE',  ( -0.000000000000000000, -1.000000000000000000, -0.000000000000000000 ) ) ;
#29879 = CIRCLE ( 'NONE', #71832, 0.09999999999999982514 ) ;
#29880 = CARTESIAN_POINT ( 'NONE',  ( -11.84999999999999787, 12.50000000000000000, -6.083687093685485436 ) ) ;
#29881 = CONICAL_SURFACE ( 'NONE', #103023, 0.09999999999999982514, 0.003490658503988666988 ) ;
#29882 = PLANE ( 'NONE',  #63077 ) ;
#29883 = CIRCLE ( 'NONE', #86292, 0.06509327318403745899 ) ;
#29884 = EDGE_CURVE ( 'NONE', #54255, #117981, #58848, .T. ) ;
#29885 = AXIS2_PLACEMENT_3D ( 'NONE', #50908, #52187, #20796 ) ;
#29886 = ORIENTED_EDGE ( 'NONE', *, *, #49034, .T. ) ;
#29887 = FACE_OUTER_BOUND ( 'NONE', #2144, .T. ) ;
#29888 = DIRECTION ( 'NONE',  ( 0.000000000000000000, 0.000000000000000000, 1.000000000000000000 ) ) ;
#29889 = CARTESIAN_POINT ( 'NONE',  ( 1.249999999999954259, 2.500000000000000000, -7.188010851410854052 ) ) ;
#29890 = CARTESIAN_POINT ( 'NONE',  ( 127.5000000000000000, -2.000000000000000000, 5.000000000000001776 ) ) ;
#29891 = CARTESIAN_POINT ( 'NONE',  ( -6.900000000000019007, 12.50000000000000000, 0.3464101615137735735 ) ) ;
#29892 = EDGE_CURVE ( 'NONE', #108388, #8747, #60784, .T. ) ;
#29893 = VERTEX_POINT ( 'NONE', #30697 ) ;
#29894 = CARTESIAN_POINT ( 'NONE',  ( 13.94999999999989626, 12.50000000000000000, 2.511473670974873507 ) ) ;
#29895 = FACE_OUTER_BOUND ( 'NONE', #43198, .T. ) ;
#29897 = ORIENTED_EDGE ( 'NONE', *, *, #60469, .F. ) ;
#29896 = DIRECTION ( 'NONE',  ( 0.000000000000000000, 1.000000000000000000, 0.000000000000000000 ) ) ;
#29898 = EDGE_CURVE ( 'NONE', #116919, #100324, #117921, .T. ) ;
#29899 = EDGE_CURVE ( 'NONE', #122002, #80402, #9269, .T. ) ;
#29900 = AXIS2_PLACEMENT_3D ( 'NONE', #109367, #19708, #121122 ) ;
#29901 = CIRCLE ( 'NONE', #36174, 0.06509327318403745899 ) ;
#29902 = ADVANCED_FACE ( 'NONE', ( #88956 ), #59523, .T. ) ;
#29903 = ADVANCED_FACE ( 'NONE', ( #91532 ), #5048, .T. ) ;
#29904 = EDGE_CURVE ( 'NONE', #18510, #47774, #49049, .T. ) ;
#29905 = ORIENTED_EDGE ( 'NONE', *, *, #1340, .T. ) ;
#29906 = LINE ( 'NONE', #109756, #787 ) ;
#29907 = CIRCLE ( 'NONE', #55235, 0.1000000000000002554 ) ;
#29908 = VERTEX_POINT ( 'NONE', #119060 ) ;
#29909 = EDGE_LOOP ( 'NONE', ( #68621, #95232, #118014, #44781 ) ) ;
#29910 = ORIENTED_EDGE ( 'NONE', *, *, #127498, .F. ) ;
#29911 = DIRECTION ( 'NONE',  ( 0.000000000000000000, 0.000000000000000000, 1.000000000000000000 ) ) ;
#29912 = AXIS2_PLACEMENT_3D ( 'NONE', #12267, #73138, #90840 ) ;
#29913 = AXIS2_PLACEMENT_3D ( 'NONE', #120824, #83493, #122759 ) ;
#29914 = ADVANCED_FACE ( 'NONE', ( #51617 ), #128424, .T. ) ;
#29915 = DIRECTION ( 'NONE',  ( 0.000000000000000000, 0.000000000000000000, 1.000000000000000000 ) ) ;
#29916 = CARTESIAN_POINT ( 'NONE',  ( 9.799999999999913669, 2.500000000000000000, -3.883716857408426648 ) ) ;
#29917 = CARTESIAN_POINT ( 'NONE',  ( 184.5000000000000000, 0.000000000000000000, 0.000000000000000000 ) ) ;
#29920 = VERTEX_POINT ( 'NONE', #109218 ) ;
#29919 = ADVANCED_FACE ( 'NONE', ( #111144 ), #89599, .T. ) ;
#29918 = CIRCLE ( 'NONE', #96795, 0.1000000000000002554 ) ;
#29921 = AXIS2_PLACEMENT_3D ( 'NONE', #37148, #27298, #17473 ) ;
#29922 = CONICAL_SURFACE ( 'NONE', #71777, 0.09999999999999982514, 0.003490658503988666988 ) ;
#29923 = CARTESIAN_POINT ( 'NONE',  ( 2.099999999999948574, 2.500000000000000000, 3.637306695894644726 ) ) ;
#29925 = ORIENTED_EDGE ( 'NONE', *, *, #91255, .F. ) ;
#29924 = AXIS2_PLACEMENT_3D ( 'NONE', #28711, #77783, #68616 ) ;
#29926 = CARTESIAN_POINT ( 'NONE',  ( 11.24999999999994316, 12.50000000000000000, 2.099970236277060032 ) ) ;
#29927 = AXIS2_PLACEMENT_3D ( 'NONE', #38322, #40252, #110271 ) ;
#29928 = FACE_OUTER_BOUND ( 'NONE', #56510, .T. ) ;
#29929 = LINE ( 'NONE', #117625, #124940 ) ;
#29930 = VECTOR ( 'NONE', #73992, 1000.000000000000000 ) ;
#29931 = EDGE_LOOP ( 'NONE', ( #80755, #99152, #117465, #57459 ) ) ;
#29932 = ORIENTED_EDGE ( 'NONE', *, *, #7719, .T. ) ;
#29933 = VERTEX_POINT ( 'NONE', #19566 ) ;
#29934 = VERTEX_POINT ( 'NONE', #50978 ) ;
#29935 = ORIENTED_EDGE ( 'NONE', *, *, #223, .T. ) ;
#29936 = FACE_OUTER_BOUND ( 'NONE', #119854, .T. ) ;
#29937 = DIRECTION ( 'NONE',  ( 0.000000000000000000, -0.9999939076577903929, 0.003490651415223739937 ) ) ;
#29938 = DIRECTION ( 'NONE',  ( 0.000000000000000000, 0.000000000000000000, 1.000000000000000000 ) ) ;
#29939 = FACE_BOUND ( 'NONE', #12342, .T. ) ;
#29940 = DIRECTION ( 'NONE',  ( 0.000000000000000000, -0.9999939076577903929, 0.003490651415223739937 ) ) ;
#29941 = CARTESIAN_POINT ( 'NONE',  ( 186.9062500006828316, -8.891194145520236347, -1.633285867636356693E-15 ) ) ;
#29942 = DIRECTION ( 'NONE',  ( -0.000000000000000000, -1.000000000000000000, -0.000000000000000000 ) ) ;
#29943 = DIRECTION ( 'NONE',  ( -0.000000000000000000, -1.000000000000000000, -0.000000000000000000 ) ) ;
#29944 = AXIS2_PLACEMENT_3D ( 'NONE', #30907, #70808, #30267 ) ;
#29945 = DIRECTION ( 'NONE',  ( 0.000000000000000000, -0.9999939076577903929, 0.003490651415223739937 ) ) ;
#29946 = DIRECTION ( 'NONE',  ( 0.000000000000000000, 0.000000000000000000, 1.000000000000000000 ) ) ;
#29947 = EDGE_CURVE ( 'NONE', #42572, #73565, #13455, .T. ) ;
#29948 = CARTESIAN_POINT ( 'NONE',  ( 3.949999999999938893, 12.50000000000000000, 6.148780366869520009 ) ) ;
#29949 = CIRCLE ( 'NONE', #53026, 0.06509327318403745899 ) ;
#29950 = ADVANCED_FACE ( 'NONE', ( #90883 ), #111676, .T. ) ;
#29951 = AXIS2_PLACEMENT_3D ( 'NONE', #110906, #43486, #90634 ) ;
#29952 = CIRCLE ( 'NONE', #61255, 0.06509327318403745899 ) ;
#29953 = DIRECTION ( 'NONE',  ( 0.000000000000000000, 0.000000000000000000, -1.000000000000000000 ) ) ;
#29954 = EDGE_CURVE ( 'NONE', #98108, #56262, #23853, .T. ) ;
#29955 = ORIENTED_EDGE ( 'NONE', *, *, #43095, .F. ) ;
#29956 = EDGE_LOOP ( 'NONE', ( #11064, #52242, #97116, #56553 ) ) ;
#29957 = VERTEX_POINT ( 'NONE', #11674 ) ;
#29958 = ORIENTED_EDGE ( 'NONE', *, *, #114050, .T. ) ;
#29959 = CARTESIAN_POINT ( 'NONE',  ( -12.89999999999999147, 2.500000000000000000, 3.637306695894644726 ) ) ;
#29960 = FACE_OUTER_BOUND ( 'NONE', #99903, .T. ) ;
#29961 = ADVANCED_FACE ( 'NONE', ( #30044 ), #80380, .T. ) ;
#29962 = FACE_BOUND ( 'NONE', #49907, .T. ) ;
#29963 = AXIS2_PLACEMENT_3D ( 'NONE', #96096, #86259, #96727 ) ;
#29964 = CIRCLE ( 'NONE', #103110, 0.09999999999999982514 ) ;
#29965 = FACE_OUTER_BOUND ( 'NONE', #12159, .T. ) ;
#29966 = ADVANCED_FACE ( 'NONE', ( #109886 ), #78234, .T. ) ;
#29967 = AXIS2_PLACEMENT_3D ( 'NONE', #78943, #107080, #87443 ) ;
#29968 = AXIS2_PLACEMENT_3D ( 'NONE', #43920, #22351, #22985 ) ;
#29969 = ADVANCED_FACE ( 'NONE', ( #90219 ), #11325, .T. ) ;
#29970 = VERTEX_POINT ( 'NONE', #22170 ) ;
#29971 = CARTESIAN_POINT ( 'NONE',  ( 12.89999999999990088, 12.50000000000000000, -4.395220292106239768 ) ) ;
#29972 = DIRECTION ( 'NONE',  ( -0.000000000000000000, -1.000000000000000000, -0.000000000000000000 ) ) ;
#29973 = DIRECTION ( 'NONE',  ( 0.000000000000000000, 0.000000000000000000, 1.000000000000000000 ) ) ;
#29974 = FACE_OUTER_BOUND ( 'NONE', #83763, .T. ) ;
#29975 = ORIENTED_EDGE ( 'NONE', *, *, #92069, .T. ) ;
#29976 = CARTESIAN_POINT ( 'NONE',  ( -12.04999999999999538, 2.500000000000000000, 6.395190528383296602 ) ) ;
#29977 = ADVANCED_FACE ( 'NONE', ( #112471 ), #86619, .T. ) ;
#29978 = AXIS2_PLACEMENT_3D ( 'NONE', #18640, #98479, #8808 ) ;
#29979 = VECTOR ( 'NONE', #16000, 1000.000000000000000 ) ;
#29980 = CIRCLE ( 'NONE', #57052, 0.06509327318403745899 ) ;
#29981 = ORIENTED_EDGE ( 'NONE', *, *, #30997, .F. ) ;
#29982 = EDGE_LOOP ( 'NONE', ( #109511, #47393, #36221, #41974 ) ) ;
#29983 = DIRECTION ( 'NONE',  ( 0.000000000000000000, 0.000000000000000000, 1.000000000000000000 ) ) ;
#29984 = CARTESIAN_POINT ( 'NONE',  ( 1.249999999999988454, 12.50000000000000000, -2.165063509461101710 ) ) ;
#29985 = VECTOR ( 'NONE', #62497, 1000.000000000000000 ) ;
#29986 = ORIENTED_EDGE ( 'NONE', *, *, #17170, .F. ) ;
#29987 = DIRECTION ( 'NONE',  ( 0.000000000000000000, 0.000000000000000000, 1.000000000000000000 ) ) ;
#29988 = LINE ( 'NONE', #15954, #104271 ) ;
#29989 = ORIENTED_EDGE ( 'NONE', *, *, #16324, .T. ) ;
#29990 = FACE_OUTER_BOUND ( 'NONE', #15126, .T. ) ;
#29991 = EDGE_LOOP ( 'NONE', ( #43650, #49783, #64579, #30536 ) ) ;
#29992 = FACE_OUTER_BOUND ( 'NONE', #85439, .T. ) ;
#29993 = EDGE_CURVE ( 'NONE', #92156, #81635, #71976, .T. ) ;
#29994 = ORIENTED_EDGE ( 'NONE', *, *, #14298, .F. ) ;
#29995 = DIRECTION ( 'NONE',  ( -0.000000000000000000, -1.000000000000000000, -0.000000000000000000 ) ) ;
#29996 = ORIENTED_EDGE ( 'NONE', *, *, #98032, .T. ) ;
#29997 = CARTESIAN_POINT ( 'NONE',  ( 111.0564249898064588, 6.601081615736754671, -3.969972484914319200 ) ) ;
#29998 = VERTEX_POINT ( 'NONE', #44354 ) ;
#29999 = DIRECTION ( 'NONE',  ( -0.000000000000000000, -1.000000000000000000, -0.000000000000000000 ) ) ;
#30000 = CARTESIAN_POINT ( 'NONE',  ( 4.599999999999938360, 2.500000000000000000, -0.7928203230275542301 ) ) ;
#30001 = AXIS2_PLACEMENT_3D ( 'NONE', #84418, #26790, #85059 ) ;
#30002 = DIRECTION ( 'NONE',  ( -0.000000000000000000, -1.000000000000000000, -0.000000000000000000 ) ) ;
#30003 = AXIS2_PLACEMENT_3D ( 'NONE', #119483, #108381, #78300 ) ;
#30004 = CARTESIAN_POINT ( 'NONE',  ( 0.1999999999999562961, 2.500000000000000000, 4.576537180435972019 ) ) ;
#30005 = CARTESIAN_POINT ( 'NONE',  ( -4.999999999999986677, 2.500000000000000000, 0.09999999999999772959 ) ) ;
#30006 = ORIENTED_EDGE ( 'NONE', *, *, #73288, .F. ) ;
#30007 = ORIENTED_EDGE ( 'NONE', *, *, #21073, .F. ) ;
#30008 = VERTEX_POINT ( 'NONE', #22811 ) ;
#30009 = PLANE ( 'NONE',  #129101 ) ;
#30010 = VECTOR ( 'NONE', #67511, 1000.000000000000000 ) ;
#30011 = EDGE_CURVE ( 'NONE', #90336, #78915, #43745, .T. ) ;
#30012 = DIRECTION ( 'NONE',  ( 0.000000000000000000, -1.846105847067148022E-16, 1.000000000000000000 ) ) ;
#30013 = CONICAL_SURFACE ( 'NONE', #48894, 0.1000000000000002554, 0.003490658503988666988 ) ;
#30015 = DIRECTION ( 'NONE',  ( 0.000000000000000000, -0.9999939076577903929, 0.003490651415223739937 ) ) ;
#30014 = CONICAL_SURFACE ( 'NONE', #65490, 0.1000000000000002554, 0.003490658503988666988 ) ;
#30017 = ORIENTED_EDGE ( 'NONE', *, *, #35361, .T. ) ;
#30016 = VERTEX_POINT ( 'NONE', #74470 ) ;
#30018 = ORIENTED_EDGE ( 'NONE', *, *, #32447, .F. ) ;
#30019 = LINE ( 'NONE', #58194, #74911 ) ;
#30020 = ORIENTED_EDGE ( 'NONE', *, *, #56646, .T. ) ;
#30021 = CARTESIAN_POINT ( 'NONE',  ( 12.89999999999990088, 2.500000000000000000, -4.330127018922201643 ) ) ;
#30022 = AXIS2_PLACEMENT_3D ( 'NONE', #121274, #21803, #62996 ) ;
#30023 = CIRCLE ( 'NONE', #27949, 0.09999999999999982514 ) ;
#30024 = DIRECTION ( 'NONE',  ( -0.000000000000000000, 1.000000000000000000, -0.000000000000000000 ) ) ;
#30025 = DIRECTION ( 'NONE',  ( 0.000000000000000000, 0.000000000000000000, -1.000000000000000000 ) ) ;
#30026 = LINE ( 'NONE', #38569, #82102 ) ;
#30027 = AXIS2_PLACEMENT_3D ( 'NONE', #37090, #49502, #109697 ) ;
#30028 = DIRECTION ( 'NONE',  ( 0.000000000000000000, 0.000000000000000000, -1.000000000000000000 ) ) ;
#30029 = DIRECTION ( 'NONE',  ( 0.000000000000000000, 1.000000000000000000, 0.000000000000000000 ) ) ;
#30030 = VECTOR ( 'NONE', #49205, 1000.000000000000000 ) ;
#30031 = ADVANCED_FACE ( 'NONE', ( #101999 ), #48993, .T. ) ;
#30032 = CARTESIAN_POINT ( 'NONE',  ( -4.150000000000024336, 2.500000000000000000, -2.165063509461101710 ) ) ;
#30033 = ORIENTED_EDGE ( 'NONE', *, *, #111064, .T. ) ;
#30034 = VERTEX_POINT ( 'NONE', #92165 ) ;
#30035 = FACE_OUTER_BOUND ( 'NONE', #27419, .T. ) ;
#30036 = VERTEX_POINT ( 'NONE', #33898 ) ;
#30037 = VERTEX_POINT ( 'NONE', #122293 ) ;
#30038 = CARTESIAN_POINT ( 'NONE',  ( 185.4010416670080588, -4.367472073101519747, 7.564683531249999149 ) ) ;
#30039 = CARTESIAN_POINT ( 'NONE',  ( 12.49999999999990585, 2.500000000000000000, 3.737306695894644371 ) ) ;
#30040 = PLANE ( 'NONE',  #100112 ) ;
#30041 = AXIS2_PLACEMENT_3D ( 'NONE', #3993, #33483, #83842 ) ;
#30042 = DIRECTION ( 'NONE',  ( -0.000000000000000000, 1.000000000000000000, -0.000000000000000000 ) ) ;
#30043 = FACE_OUTER_BOUND ( 'NONE', #31071, .T. ) ;
#30044 = FACE_OUTER_BOUND ( 'NONE', #57709, .T. ) ;
#30045 = LINE ( 'NONE', #52900, #83271 ) ;
#30046 = VECTOR ( 'NONE', #14115, 1000.000000000000000 ) ;
#30048 = CIRCLE ( 'NONE', #48831, 0.06509327318403745899 ) ;
#30047 = DIRECTION ( 'NONE',  ( -0.000000000000000000, -1.000000000000000000, -0.000000000000000000 ) ) ;
#30049 = AXIS2_PLACEMENT_3D ( 'NONE', #5589, #124742, #56622 ) ;
#30050 = ORIENTED_EDGE ( 'NONE', *, *, #75952, .T. ) ;
#30051 = ADVANCED_FACE ( 'NONE', ( #64004 ), #63658, .T. ) ;
#30052 = ORIENTED_EDGE ( 'NONE', *, *, #127897, .T. ) ;
#30053 = VERTEX_POINT ( 'NONE', #123549 ) ;
#30054 = ORIENTED_EDGE ( 'NONE', *, *, #9936, .T. ) ;
#30055 = AXIS2_PLACEMENT_3D ( 'NONE', #114442, #117005, #94813 ) ;
#30056 = DIRECTION ( 'NONE',  ( 0.000000000000000000, 0.000000000000000000, 1.000000000000000000 ) ) ;
#30057 = DIRECTION ( 'NONE',  ( -0.000000000000000000, 1.000000000000000000, -0.000000000000000000 ) ) ;
#30058 = VECTOR ( 'NONE', #71721, 1000.000000000000000 ) ;
#30060 = EDGE_CURVE ( 'NONE', #100762, #3469, #65693, .T. ) ;
#30059 = CIRCLE ( 'NONE', #103204, 0.1000000000000002554 ) ;
#30061 = ORIENTED_EDGE ( 'NONE', *, *, #28602, .F. ) ;
#30062 = DIRECTION ( 'NONE',  ( -0.000000000000000000, -1.000000000000000000, -0.000000000000000000 ) ) ;
#30063 = CIRCLE ( 'NONE', #53128, 0.1000000000000000472 ) ;
#30064 = CARTESIAN_POINT ( 'NONE',  ( -10.85000000000000142, 12.50000000000000000, -1.407149913249508666 ) ) ;
#30065 = CARTESIAN_POINT ( 'NONE',  ( -4.600000000000024514, 2.500000000000000000, 5.122947341949749323 ) ) ;
#30067 = ORIENTED_EDGE ( 'NONE', *, *, #112844, .F. ) ;
#30066 = CARTESIAN_POINT ( 'NONE',  ( 6.049999999999934097, 12.50000000000000000, 6.083687093685483660 ) ) ;
#30068 = ADVANCED_FACE ( 'NONE', ( #32643 ), #52254, .T. ) ;
#30069 = EDGE_CURVE ( 'NONE', #61997, #15557, #65779, .T. ) ;
#30070 = EDGE_CURVE ( 'NONE', #60798, #17292, #124212, .T. ) ;
#30071 = CARTESIAN_POINT ( 'NONE',  ( -9.600000000000006750, 2.500000000000000000, 5.022947341949748790 ) ) ;
#30073 = EDGE_CURVE ( 'NONE', #7948, #24838, #115966, .T. ) ;
#30072 = CIRCLE ( 'NONE', #78186, 0.09999999999999982514 ) ;
#30074 = DIRECTION ( 'NONE',  ( 0.000000000000000000, 0.000000000000000000, 1.000000000000000000 ) ) ;
#30075 = ORIENTED_EDGE ( 'NONE', *, *, #50637, .T. ) ;
#30077 = EDGE_CURVE ( 'NONE', #74262, #79739, #53288, .T. ) ;
#30076 = CIRCLE ( 'NONE', #4998, 0.06509327318403745899 ) ;
#30078 = CONICAL_SURFACE ( 'NONE', #80244, 0.1000000000000002554, 0.003490658503988666988 ) ;
#30079 = ORIENTED_EDGE ( 'NONE', *, *, #58416, .T. ) ;
#30081 = ORIENTED_EDGE ( 'NONE', *, *, #26089, .T. ) ;
#30080 = ADVANCED_FACE ( 'NONE', ( #124859 ), #24035, .T. ) ;
#30082 = EDGE_LOOP ( 'NONE', ( #16188, #12434 ) ) ;
#30083 = CARTESIAN_POINT ( 'NONE',  ( 10.79999999999991012, 2.500000000000000000, 4.330127018922196314 ) ) ;
#30084 = AXIS2_PLACEMENT_3D ( 'NONE', #27691, #67614, #107561 ) ;
#30085 = EDGE_CURVE ( 'NONE', #51302, #96401, #94106, .T. ) ;
#30086 = FACE_OUTER_BOUND ( 'NONE', #128327, .T. ) ;
#30087 = DIRECTION ( 'NONE',  ( 0.000000000000000000, 0.000000000000000000, 1.000000000000000000 ) ) ;
#30088 = CONICAL_SURFACE ( 'NONE', #78095, 0.1000000000000000472, 0.003490658503988666988 ) ;
#30089 = EDGE_CURVE ( 'NONE', #110807, #57482, #38623, .T. ) ;
#30090 = EDGE_CURVE ( 'NONE', #83674, #35537, #80480, .T. ) ;
#30091 = CARTESIAN_POINT ( 'NONE',  ( -9.800000000000006040, 12.50000000000000000, 4.676537180435972552 ) ) ;
#30092 = ORIENTED_EDGE ( 'NONE', *, *, #46893, .F. ) ;
#30093 = CARTESIAN_POINT ( 'NONE',  ( 11.44999999999990870, 12.50000000000000000, 6.776507416713035248 ) ) ;
#30094 = CARTESIAN_POINT ( 'NONE',  ( 14.34999999999989306, 12.50000000000000000, -1.753560074763288679 ) ) ;
#30095 = CARTESIAN_POINT ( 'NONE',  ( -8.300000000000009592, 2.500000000000000000, 4.330127018922196314 ) ) ;
#30096 = DIRECTION ( 'NONE',  ( 0.000000000000000000, 0.000000000000000000, 1.000000000000000000 ) ) ;
#30097 = ADVANCED_FACE ( 'NONE', ( #12947 ), #52899, .T. ) ;
#30098 = ORIENTED_EDGE ( 'NONE', *, *, #126529, .T. ) ;
#30099 = FACE_OUTER_BOUND ( 'NONE', #125938, .T. ) ;
#30100 = ORIENTED_EDGE ( 'NONE', *, *, #94914, .F. ) ;
#30101 = EDGE_LOOP ( 'NONE', ( #82139, #96495, #50346, #87342 ) ) ;
#30103 = CIRCLE ( 'NONE', #90719, 0.1000000000000000472 ) ;
#30102 = CARTESIAN_POINT ( 'NONE',  ( -11.64999999999999680, 2.500000000000000000, 1.472243186433545459 ) ) ;
#30104 = CONICAL_SURFACE ( 'NONE', #28028, 0.1000000000000000472, 0.003490658503988666988 ) ;
#30105 = CARTESIAN_POINT ( 'NONE',  ( -15.19999999999998330, 2.500000000000000000, 0.3464101615137758494 ) ) ;
#30106 = FACE_BOUND ( 'NONE', #91610, .T. ) ;
#30107 = DIRECTION ( 'NONE',  ( 0.000000000000000000, 0.000000000000000000, 1.000000000000000000 ) ) ;
#30108 = DIRECTION ( 'NONE',  ( -0.000000000000000000, -1.000000000000000000, -0.000000000000000000 ) ) ;
#30109 = DIRECTION ( 'NONE',  ( 0.000000000000000000, -0.9999939076577903929, 0.003490651415223739937 ) ) ;
#30110 = CONICAL_SURFACE ( 'NONE', #48978, 0.1000000000000002554, 0.003490658503988666988 ) ;
#30111 = CONICAL_SURFACE ( 'NONE', #55229, 0.1000000000000002554, 0.003490658503988666988 ) ;
#30112 = AXIS2_PLACEMENT_3D ( 'NONE', #103739, #117227, #104372 ) ;
#30113 = CARTESIAN_POINT ( 'NONE',  ( -1.850000000000033396, 2.500000000000000000, -6.841600689897077814 ) ) ;
#30114 = DIRECTION ( 'NONE',  ( 0.000000000000000000, 1.000000000000000000, 0.000000000000000000 ) ) ;
#30115 = FACE_OUTER_BOUND ( 'NONE', #66438, .T. ) ;
#30116 = DIRECTION ( 'NONE',  ( 0.000000000000000000, 1.000000000000000000, 0.000000000000000000 ) ) ;
#30117 = ORIENTED_EDGE ( 'NONE', *, *, #78204, .T. ) ;
#30119 = DIRECTION ( 'NONE',  ( 0.000000000000000000, 0.000000000000000000, -1.000000000000000000 ) ) ;
#30118 = CIRCLE ( 'NONE', #11317, 0.1000000000000002554 ) ;
#30120 = CIRCLE ( 'NONE', #7089, 0.1000000000000000472 ) ;
#30121 = CARTESIAN_POINT ( 'NONE',  ( 9.199999999999915801, 12.50000000000000000, 4.395220292106234439 ) ) ;
#30122 = ORIENTED_EDGE ( 'NONE', *, *, #35822, .T. ) ;
#30123 = EDGE_LOOP ( 'NONE', ( #101261, #68354, #95075, #115971 ) ) ;
#30124 = DIRECTION ( 'NONE',  ( 0.000000000000000000, -0.9999939076577903929, 0.003490651415223739937 ) ) ;
#30125 = CARTESIAN_POINT ( 'NONE',  ( 4.399999999999940847, 2.500000000000000000, -4.676537180435977881 ) ) ;
#30126 = FACE_BOUND ( 'NONE', #116902, .T. ) ;
#30127 = DIRECTION ( 'NONE',  ( 0.000000000000000000, 0.000000000000000000, 1.000000000000000000 ) ) ;
#30128 = EDGE_CURVE ( 'NONE', #64157, #11947, #55333, .T. ) ;
#30129 = FACE_OUTER_BOUND ( 'NONE', #100080, .T. ) ;
#30130 = ADVANCED_FACE ( 'NONE', ( #65925 ), #97183, .T. ) ;
#30131 = VERTEX_POINT ( 'NONE', #17459 ) ;
#30132 = DIRECTION ( 'NONE',  ( -0.000000000000000000, 1.000000000000000000, -0.000000000000000000 ) ) ;
#30133 = CARTESIAN_POINT ( 'NONE',  ( -14.14999999999998614, 12.50000000000000000, -2.165063509461099489 ) ) ;
#30135 = ORIENTED_EDGE ( 'NONE', *, *, #36103, .F. ) ;
#30134 = VECTOR ( 'NONE', #97959, 1000.000000000000000 ) ;
#30136 = CARTESIAN_POINT ( 'NONE',  ( 10.59999999999991260, 2.500000000000000000, 0.3464101615137735735 ) ) ;
#30137 = LINE ( 'NONE', #38673, #107601 ) ;
#30138 = EDGE_CURVE ( 'NONE', #101406, #123848, #17658, .T. ) ;
#30139 = DIRECTION ( 'NONE',  ( 0.000000000000000000, 1.000000000000000000, 0.000000000000000000 ) ) ;
#30140 = FACE_OUTER_BOUND ( 'NONE', #10098, .T. ) ;
#30141 = CIRCLE ( 'NONE', #80310, 0.06509327318403745899 ) ;
#30142 = AXIS2_PLACEMENT_3D ( 'NONE', #106705, #127017, #7210 ) ;
#30143 = ORIENTED_EDGE ( 'NONE', *, *, #22360, .F. ) ;
#30144 = DIRECTION ( 'NONE',  ( 0.000000000000000000, 0.000000000000000000, 1.000000000000000000 ) ) ;
#30145 = DIRECTION ( 'NONE',  ( -4.274815082592931898E-19, -0.9999939076577903929, -0.003490651415223739937 ) ) ;
#30146 = CARTESIAN_POINT ( 'NONE',  ( -11.89999999999999680, 12.50000000000000000, -3.983716857408423628 ) ) ;
#30147 = DIRECTION ( 'NONE',  ( 0.000000000000000000, 1.000000000000000000, 0.000000000000000000 ) ) ;
#30148 = ORIENTED_EDGE ( 'NONE', *, *, #7883, .T. ) ;
#30149 = ORIENTED_EDGE ( 'NONE', *, *, #53412, .T. ) ;
#30150 = CIRCLE ( 'NONE', #69848, 0.1000000000000000472 ) ;
#30151 = CARTESIAN_POINT ( 'NONE',  ( 4.599999999999935696, 12.50000000000000000, 4.957854068765711553 ) ) ;
#30152 = EDGE_LOOP ( 'NONE', ( #19336, #90316, #97575, #40216 ) ) ;
#30153 = DIRECTION ( 'NONE',  ( 0.000000000000000000, 1.000000000000000000, 0.000000000000000000 ) ) ;
#30154 = DIRECTION ( 'NONE',  ( -0.000000000000000000, 1.000000000000000000, -0.000000000000000000 ) ) ;
#30155 = DIRECTION ( 'NONE',  ( 0.000000000000000000, 1.000000000000000000, 0.000000000000000000 ) ) ;
#30156 = ORIENTED_EDGE ( 'NONE', *, *, #82059, .T. ) ;
#30157 = DIRECTION ( 'NONE',  ( 0.000000000000000000, 0.000000000000000000, 1.000000000000000000 ) ) ;
#30158 = DIRECTION ( 'NONE',  ( -0.000000000000000000, -1.000000000000000000, -0.000000000000000000 ) ) ;
#30159 = DIRECTION ( 'NONE',  ( -0.000000000000000000, -1.000000000000000000, -0.000000000000000000 ) ) ;
#30160 = LINE ( 'NONE', #41273, #101960 ) ;
#30161 = CARTESIAN_POINT ( 'NONE',  ( 4.399999999999937295, 12.50000000000000000, 4.741630453620009789 ) ) ;
#30162 = CARTESIAN_POINT ( 'NONE',  ( -1.050000000000037348, 12.50000000000000000, -2.511473670974877948 ) ) ;
#30163 = EDGE_LOOP ( 'NONE', ( #83607, #39768, #120313, #25812 ) ) ;
#30164 = EDGE_LOOP ( 'NONE', ( #91439, #96464 ) ) ;
#30165 = DIRECTION ( 'NONE',  ( 0.000000000000000000, 0.000000000000000000, 1.000000000000000000 ) ) ;
#30167 = ORIENTED_EDGE ( 'NONE', *, *, #75454, .T. ) ;
#30166 = AXIS2_PLACEMENT_3D ( 'NONE', #53754, #123765, #64214 ) ;
#30168 = AXIS2_PLACEMENT_3D ( 'NONE', #93553, #111909, #123637 ) ;
#30169 = CIRCLE ( 'NONE', #36431, 0.1000000000000002554 ) ;
#30170 = LINE ( 'NONE', #28878, #32592 ) ;
#30172 = ORIENTED_EDGE ( 'NONE', *, *, #117636, .T. ) ;
#30171 = ORIENTED_EDGE ( 'NONE', *, *, #98939, .F. ) ;
#30173 = ORIENTED_EDGE ( 'NONE', *, *, #82868, .T. ) ;
#30174 = VECTOR ( 'NONE', #91781, 1000.000000000000000 ) ;
#30175 = CARTESIAN_POINT ( 'NONE',  ( -2.900000000000029665, 2.500000000000000000, 3.537306695894645081 ) ) ;
#30176 = AXIS2_PLACEMENT_3D ( 'NONE', #9649, #98656, #8349 ) ;
#30177 = CARTESIAN_POINT ( 'NONE',  ( -13.74999999999995381, 2.500000000000000000, -2.065063509461099844 ) ) ;
#30178 = CARTESIAN_POINT ( 'NONE',  ( -2.900000000000029665, 2.500000000000000000, 3.737306695894644371 ) ) ;
#30179 = SHAPE_REPRESENTATION_RELATIONSHIP ( 'NONE' , 'NONE' ,  #89551, #108597 ) ;
#30180 = DIRECTION ( 'NONE',  ( -0.000000000000000000, 1.000000000000000000, -0.000000000000000000 ) ) ;
#30181 = CARTESIAN_POINT ( 'NONE',  ( 4.799999999999939426, 2.500000000000000000, -4.676537180435977881 ) ) ;
#30182 = CARTESIAN_POINT ( 'NONE',  ( 186.0000000000000000, 0.000000000000000000, 7.700000000000000178 ) ) ;
#30183 = EDGE_CURVE ( 'NONE', #32860, #105669, #126444, .T. ) ;
#30184 = DIRECTION ( 'NONE',  ( 0.000000000000000000, 0.000000000000000000, 1.000000000000000000 ) ) ;
#30185 = FACE_OUTER_BOUND ( 'NONE', #122213, .T. ) ;
#30186 = ADVANCED_FACE ( 'NONE', ( #105209 ), #126141, .T. ) ;
#30187 = DIRECTION ( 'NONE',  ( -4.274815082592931898E-19, -0.9999939076577903929, -0.003490651415223739937 ) ) ;
#30188 = ORIENTED_EDGE ( 'NONE', *, *, #11308, .T. ) ;
#30189 = ORIENTED_EDGE ( 'NONE', *, *, #26079, .F. ) ;
#30190 = AXIS2_PLACEMENT_3D ( 'NONE', #85079, #62870, #102771 ) ;
#30191 = AXIS2_PLACEMENT_3D ( 'NONE', #93459, #122928, #103925 ) ;
#30192 = FACE_OUTER_BOUND ( 'NONE', #79337, .T. ) ;
#30193 = CIRCLE ( 'NONE', #105391, 0.06509327318403745899 ) ;
#30194 = CIRCLE ( 'NONE', #103345, 0.1000000000000002554 ) ;
#30195 = ORIENTED_EDGE ( 'NONE', *, *, #115017, .F. ) ;
#30196 = ADVANCED_FACE ( 'NONE', ( #128083 ), #74121, .T. ) ;
#30197 = EDGE_LOOP ( 'NONE', ( #93434, #76114, #29290, #121534 ) ) ;
#30198 = DIRECTION ( 'NONE',  ( -4.274815082592931898E-19, -0.9999939076577903929, -0.003490651415223739937 ) ) ;
#30199 = CARTESIAN_POINT ( 'NONE',  ( 8.099999999999923261, 12.50000000000000000, 4.611443907251934426 ) ) ;
#30200 = AXIS2_PLACEMENT_3D ( 'NONE', #127168, #8013, #6071 ) ;
#30201 = CIRCLE ( 'NONE', #92978, 0.06509327318403745899 ) ;
#30202 = DIRECTION ( 'NONE',  ( 0.000000000000000000, 0.000000000000000000, -1.000000000000000000 ) ) ;
#30204 = DIRECTION ( 'NONE',  ( 0.000000000000000000, -0.000000000000000000, 1.000000000000000000 ) ) ;
#30203 = CIRCLE ( 'NONE', #67829, 0.06509327318403741736 ) ;
#30205 = CARTESIAN_POINT ( 'NONE',  ( 8.949999999999917577, 2.500000000000000000, 6.248780366869520542 ) ) ;
#30206 = DIRECTION ( 'NONE',  ( 0.000000000000000000, -0.000000000000000000, 1.000000000000000000 ) ) ;
#30207 = ORIENTED_EDGE ( 'NONE', *, *, #40786, .F. ) ;
#30208 = CONICAL_SURFACE ( 'NONE', #119783, 0.09999999999999999167, 0.003490658503988666988 ) ;
#30210 = VERTEX_POINT ( 'NONE', #67185 ) ;
#30209 = CIRCLE ( 'NONE', #46932, 0.1000000000000002554 ) ;
#30211 = CARTESIAN_POINT ( 'NONE',  ( 11.64999999999990798, 12.50000000000000000, -2.922977105672691422 ) ) ;
#30212 = AXIS2_PLACEMENT_3D ( 'NONE', #4487, #54900, #66015 ) ;
#30213 = ORIENTED_EDGE ( 'NONE', *, *, #99226, .T. ) ;
#30215 = EDGE_CURVE ( 'NONE', #72305, #110447, #37132, .T. ) ;
#30214 = DIRECTION ( 'NONE',  ( 0.000000000000000000, -0.000000000000000000, 1.000000000000000000 ) ) ;
#30216 = EDGE_LOOP ( 'NONE', ( #46683, #105900 ) ) ;
#30217 = AXIS2_PLACEMENT_3D ( 'NONE', #53547, #24085, #72550 ) ;
#30218 = ORIENTED_EDGE ( 'NONE', *, *, #94480, .T. ) ;
#30219 = CARTESIAN_POINT ( 'NONE',  ( 8.149999999999920419, 2.500000000000000000, -2.411473670974877859 ) ) ;
#30220 = CARTESIAN_POINT ( 'NONE',  ( -8.950000000000009948, 2.500000000000000000, -1.818653347947326138 ) ) ;
#30221 = EDGE_CURVE ( 'NONE', #119823, #63624, #90828, .T. ) ;
#30222 = DIRECTION ( 'NONE',  ( 0.000000000000000000, 1.000000000000000000, 0.000000000000000000 ) ) ;
#30223 = FACE_OUTER_BOUND ( 'NONE', #14345, .T. ) ;
#30224 = DIRECTION ( 'NONE',  ( -0.000000000000000000, -1.000000000000000000, -0.000000000000000000 ) ) ;
#30225 = VERTEX_POINT ( 'NONE', #117581 ) ;
#30226 = DIRECTION ( 'NONE',  ( 0.000000000000000000, 0.000000000000000000, -1.000000000000000000 ) ) ;
#30227 = CARTESIAN_POINT ( 'NONE',  ( -7.950000000000016165, 12.50000000000000000, -6.495190528383297135 ) ) ;
#30228 = EDGE_CURVE ( 'NONE', #96489, #39393, #103453, .T. ) ;
#30229 = EDGE_CURVE ( 'NONE', #67757, #21708, #107560, .T. ) ;
#30230 = FACE_OUTER_BOUND ( 'NONE', #28745, .T. ) ;
#30231 = EDGE_CURVE ( 'NONE', #119121, #124307, #51141, .T. ) ;
#30232 = PLANE ( 'NONE',  #36812 ) ;
#30233 = ADVANCED_FACE ( 'NONE', ( #56726 ), #88781, .T. ) ;
#30234 = AXIS2_PLACEMENT_3D ( 'NONE', #88790, #21331, #389 ) ;
#30235 = FACE_OUTER_BOUND ( 'NONE', #54012, .T. ) ;
#30236 = ORIENTED_EDGE ( 'NONE', *, *, #128872, .F. ) ;
#30237 = VERTEX_POINT ( 'NONE', #56101 ) ;
#30238 = EDGE_CURVE ( 'NONE', #7578, #53869, #8290, .T. ) ;
#30239 = DIRECTION ( 'NONE',  ( 0.000000000000000000, 1.000000000000000000, 0.000000000000000000 ) ) ;
#30240 = EDGE_CURVE ( 'NONE', #120360, #96594, #45662, .T. ) ;
#30241 = VERTEX_POINT ( 'NONE', #85572 ) ;
#30242 = AXIS2_PLACEMENT_3D ( 'NONE', #61362, #13528, #53477 ) ;
#30243 = CARTESIAN_POINT ( 'NONE',  ( 1.449999999999952216, 12.50000000000000000, 1.753560074763284016 ) ) ;
#30244 = DIRECTION ( 'NONE',  ( -0.000000000000000000, 1.000000000000000000, -0.000000000000000000 ) ) ;
#30245 = AXIS2_PLACEMENT_3D ( 'NONE', #8499, #30116, #28818 ) ;
#30246 = ADVANCED_FACE ( 'NONE', ( #96039 ), #125493, .T. ) ;
#30247 = B_SPLINE_CURVE_WITH_KNOTS ( 'NONE', 3,
 ( #45517, #85422, #97179, #25866, #126648, #46142, #65775, #38269 ),
 .UNSPECIFIED., .F., .F.,
 ( 4, 2, 2, 4 ),
 ( 0.000000000000000000, 0.01659299152883686457, 0.03318598305767372914, 0.06637196611534749990 ),
 .UNSPECIFIED. ) ;
#30248 = ORIENTED_EDGE ( 'NONE', *, *, #46428, .F. ) ;
#30249 = DIRECTION ( 'NONE',  ( 0.000000000000000000, 1.000000000000000000, 0.000000000000000000 ) ) ;
#30250 = DIRECTION ( 'NONE',  ( -0.000000000000000000, 1.000000000000000000, -0.000000000000000000 ) ) ;
#30251 = EDGE_CURVE ( 'NONE', #103678, #41488, #111765, .T. ) ;
#30252 = DIRECTION ( 'NONE',  ( 1.000000000000000000, 0.000000000000000000, 0.000000000000000000 ) ) ;
#30253 = CARTESIAN_POINT ( 'NONE',  ( 1.249999999999952482, 12.50000000000000000, -5.802370205355749988 ) ) ;
#30254 = EDGE_CURVE ( 'NONE', #40749, #50291, #15601, .T. ) ;
#30255 = CONICAL_SURFACE ( 'NONE', #103395, 0.1000000000000000472, 0.003490658503988666988 ) ;
#30256 = FACE_OUTER_BOUND ( 'NONE', #91066, .T. ) ;
#30257 = CIRCLE ( 'NONE', #67875, 0.06509327318403745899 ) ;
#30258 = EDGE_LOOP ( 'NONE', ( #93867, #102590 ) ) ;
#30259 = CARTESIAN_POINT ( 'NONE',  ( 6.649999999999929301, 12.50000000000000000, 6.495190528383297135 ) ) ;
#30260 = CARTESIAN_POINT ( 'NONE',  ( 9.149999999999916866, 2.500000000000000000, 7.288010851410849256 ) ) ;
#30261 = CARTESIAN_POINT ( 'NONE',  ( 13.34999999999989662, 12.50000000000000000, -1.472243186433550122 ) ) ;
#30262 = ORIENTED_EDGE ( 'NONE', *, *, #9782, .F. ) ;
#30263 = AXIS2_PLACEMENT_3D ( 'NONE', #20640, #47519, #7567 ) ;
#30265 = VERTEX_POINT ( 'NONE', #21338 ) ;
#30264 = AXIS2_PLACEMENT_3D ( 'NONE', #71489, #111402, #21762 ) ;
#30266 = DIRECTION ( 'NONE',  ( 0.000000000000000000, -0.9999939076577903929, 0.003490651415223739937 ) ) ;
#30267 = DIRECTION ( 'NONE',  ( 0.000000000000000000, 0.000000000000000000, 1.000000000000000000 ) ) ;
#30268 = DIRECTION ( 'NONE',  ( -0.000000000000000000, -1.000000000000000000, -0.000000000000000000 ) ) ;
#30269 = AXIS2_PLACEMENT_3D ( 'NONE', #105765, #76305, #4307 ) ;
#30270 = ORIENTED_EDGE ( 'NONE', *, *, #4668, .T. ) ;
#30271 = DIRECTION ( 'NONE',  ( -0.000000000000000000, 1.000000000000000000, -0.000000000000000000 ) ) ;
#30272 = CARTESIAN_POINT ( 'NONE',  ( -7.700000000000012612, 12.50000000000000000, 4.676537180435972552 ) ) ;
#30273 = ORIENTED_EDGE ( 'NONE', *, *, #34631, .F. ) ;
#30274 = DIRECTION ( 'NONE',  ( 0.000000000000000000, 0.000000000000000000, 1.000000000000000000 ) ) ;
#30275 = VERTEX_POINT ( 'NONE', #70450 ) ;
#30276 = DIRECTION ( 'NONE',  ( 0.000000000000000000, 0.000000000000000000, 1.000000000000000000 ) ) ;
#30277 = EDGE_CURVE ( 'NONE', #73222, #65306, #118254, .T. ) ;
#30278 = CIRCLE ( 'NONE', #65941, 0.06509327318403741736 ) ;
#30279 = ORIENTED_EDGE ( 'NONE', *, *, #83709, .F. ) ;
#30280 = DIRECTION ( 'NONE',  ( 0.000000000000000000, 0.000000000000000000, -1.000000000000000000 ) ) ;
#30281 = CARTESIAN_POINT ( 'NONE',  ( 13.92826131978669046, 2.499999999999999112, -6.790916465128549184 ) ) ;
#30282 = AXIS2_PLACEMENT_3D ( 'NONE', #72393, #21335, #80913 ) ;
#30283 = EDGE_CURVE ( 'NONE', #117070, #55871, #20070, .T. ) ;
#30284 = AXIS2_PLACEMENT_3D ( 'NONE', #124690, #35036, #25839 ) ;
#30285 = AXIS2_PLACEMENT_3D ( 'NONE', #88063, #7592, #116891 ) ;
#30286 = ORIENTED_EDGE ( 'NONE', *, *, #25110, .T. ) ;
#30287 = EDGE_LOOP ( 'NONE', ( #93962, #97155, #93527, #41101 ) ) ;
#30288 = DIRECTION ( 'NONE',  ( 0.000000000000000000, 0.000000000000000000, 1.000000000000000000 ) ) ;
#30289 = DIRECTION ( 'NONE',  ( 0.000000000000000000, -0.9999939076577903929, 0.003490651415223739937 ) ) ;
#30290 = ORIENTED_EDGE ( 'NONE', *, *, #16879, .T. ) ;
#30291 = PLANE ( 'NONE',  #40596 ) ;
#30292 = CARTESIAN_POINT ( 'NONE',  ( 186.5677083336747160, -4.367472073101514418, -7.564683531250002702 ) ) ;
#30293 = CIRCLE ( 'NONE', #55406, 0.06509327318403745899 ) ;
#30294 = AXIS2_PLACEMENT_3D ( 'NONE', #68973, #119356, #116776 ) ;
#30295 = PLANE ( 'NONE',  #22340 ) ;
#30296 = CARTESIAN_POINT ( 'NONE',  ( 105.7603592657142144, 7.458072953931099036, -4.482094334535867475 ) ) ;
#30297 = CARTESIAN_POINT ( 'NONE',  ( 11.44999999999991047, 2.500000000000000000, 6.248780366869520542 ) ) ;
#30298 = AXIS2_PLACEMENT_3D ( 'NONE', #8947, #120214, #111684 ) ;
#30299 = CARTESIAN_POINT ( 'NONE',  ( 11.24999999999991118, 2.500000000000000000, 5.902370205355745192 ) ) ;
#30300 = DIRECTION ( 'NONE',  ( -0.000000000000000000, -1.000000000000000000, -0.000000000000000000 ) ) ;
#30301 = AXIS2_PLACEMENT_3D ( 'NONE', #26012, #94099, #55467 ) ;
#30302 = AXIS2_PLACEMENT_3D ( 'NONE', #84368, #26105, #104640 ) ;
#30303 = ORIENTED_EDGE ( 'NONE', *, *, #128158, .T. ) ;
#30304 = ORIENTED_EDGE ( 'NONE', *, *, #38584, .T. ) ;
#30305 = VERTEX_POINT ( 'NONE', #30547 ) ;
#30306 = DIRECTION ( 'NONE',  ( 0.000000000000000000, -0.9999939076577903929, 0.003490651415223739937 ) ) ;
#30307 = DIRECTION ( 'NONE',  ( 0.000000000000000000, 1.000000000000000000, 0.000000000000000000 ) ) ;
#30308 = AXIS2_PLACEMENT_3D ( 'NONE', #57409, #86857, #26660 ) ;
#30309 = DIRECTION ( 'NONE',  ( 0.000000000000000000, 0.000000000000000000, -1.000000000000000000 ) ) ;
#30311 = ORIENTED_EDGE ( 'NONE', *, *, #113227, .T. ) ;
#30310 = ORIENTED_EDGE ( 'NONE', *, *, #119539, .F. ) ;
#30312 = FACE_BOUND ( 'NONE', #100347, .T. ) ;
#30313 = ORIENTED_EDGE ( 'NONE', *, *, #15548, .T. ) ;
#30314 = DIRECTION ( 'NONE',  ( 0.000000000000000000, 0.000000000000000000, -1.000000000000000000 ) ) ;
#30315 = DIRECTION ( 'NONE',  ( -0.000000000000000000, 1.000000000000000000, -0.000000000000000000 ) ) ;
#30316 = CARTESIAN_POINT ( 'NONE',  ( -11.04999999999999893, 2.500000000000000000, 1.918653347947321564 ) ) ;
#30317 = FACE_OUTER_BOUND ( 'NONE', #43174, .T. ) ;
#30318 = DIRECTION ( 'NONE',  ( 0.000000000000000000, 0.000000000000000000, -1.000000000000000000 ) ) ;
#30319 = FACE_OUTER_BOUND ( 'NONE', #58346, .T. ) ;
#30320 = PLANE ( 'NONE',  #127881 ) ;
#30321 = LINE ( 'NONE', #67631, #114287 ) ;
#30322 = CONICAL_SURFACE ( 'NONE', #49200, 0.1000000000000000472, 0.003490658503988666988 ) ;
#30323 = DIRECTION ( 'NONE',  ( -0.000000000000000000, -1.000000000000000000, -0.000000000000000000 ) ) ;
#30324 = ADVANCED_FACE ( 'NONE', ( #79620 ), #69142, .T. ) ;
#30325 = EDGE_LOOP ( 'NONE', ( #77414, #45887, #65344, #115571 ) ) ;
#30326 = ORIENTED_EDGE ( 'NONE', *, *, #62660, .F. ) ;
#30327 = ORIENTED_EDGE ( 'NONE', *, *, #118802, .F. ) ;
#30328 = ORIENTED_EDGE ( 'NONE', *, *, #49578, .F. ) ;
#30329 = CARTESIAN_POINT ( 'NONE',  ( -2.900000000000029221, 2.500000000000000000, -5.022947341949754119 ) ) ;
#30330 = DIRECTION ( 'NONE',  ( 0.000000000000000000, 0.000000000000000000, -1.000000000000000000 ) ) ;
#30332 = VERTEX_POINT ( 'NONE', #8927 ) ;
#30331 = ORIENTED_EDGE ( 'NONE', *, *, #73035, .F. ) ;
#30333 = ORIENTED_EDGE ( 'NONE', *, *, #110564, .F. ) ;
#30334 = DIRECTION ( 'NONE',  ( 0.000000000000000000, 1.000000000000000000, 0.000000000000000000 ) ) ;
#30335 = CONICAL_SURFACE ( 'NONE', #3128, 0.1000000000000002554, 0.003490658503988666988 ) ;
#30336 = EDGE_CURVE ( 'NONE', #22266, #79729, #19829, .T. ) ;
#30337 = CIRCLE ( 'NONE', #101420, 0.06509327318403745899 ) ;
#30338 = DIRECTION ( 'NONE',  ( 0.000000000000000000, 0.000000000000000000, 1.000000000000000000 ) ) ;
#30339 = DIRECTION ( 'NONE',  ( 0.000000000000000000, 1.000000000000000000, 0.000000000000000000 ) ) ;
#30340 = CARTESIAN_POINT ( 'NONE',  ( -5.650000000000023448, 12.50000000000000000, -6.841600689897078702 ) ) ;
#30341 = DIRECTION ( 'NONE',  ( 0.000000000000000000, 0.000000000000000000, -1.000000000000000000 ) ) ;
#30342 = DIRECTION ( 'NONE',  ( 0.000000000000000000, 1.000000000000000000, 0.000000000000000000 ) ) ;
#30343 = EDGE_CURVE ( 'NONE', #53599, #72890, #82533, .T. ) ;
#30344 = CARTESIAN_POINT ( 'NONE',  ( -12.09999999999999609, 2.500000000000000000, 0.1000000000000017403 ) ) ;
#30345 = ADVANCED_FACE ( 'NONE', ( #100541 ), #99915, .T. ) ;
#30346 = ORIENTED_EDGE ( 'NONE', *, *, #18974, .T. ) ;
#30347 = CARTESIAN_POINT ( 'NONE',  ( -0.4000000000000331624, 2.500000000000000000, 0.000000000000000000 ) ) ;
#30348 = ORIENTED_EDGE ( 'NONE', *, *, #75302, .F. ) ;
#30349 = CIRCLE ( 'NONE', #122276, 0.06509327318403745899 ) ;
#30350 = ORIENTED_EDGE ( 'NONE', *, *, #33319, .T. ) ;
#30351 = VERTEX_POINT ( 'NONE', #29880 ) ;
#30352 = AXIS2_PLACEMENT_3D ( 'NONE', #47681, #87581, #8375 ) ;
#30353 = CARTESIAN_POINT ( 'NONE',  ( 11.44999999999990692, 2.500000000000000000, 1.918653347947321564 ) ) ;
#30354 = ORIENTED_EDGE ( 'NONE', *, *, #63590, .F. ) ;
#30355 = EDGE_CURVE ( 'NONE', #15089, #52919, #99259, .T. ) ;
#30356 = ORIENTED_EDGE ( 'NONE', *, *, #55131, .T. ) ;
#30357 = CARTESIAN_POINT ( 'NONE',  ( -8.550000000000011369, 2.500000000000000000, 1.918653347947321564 ) ) ;
#30358 = DIRECTION ( 'NONE',  ( 0.000000000000000000, 0.000000000000000000, 1.000000000000000000 ) ) ;
#30359 = LINE ( 'NONE', #101005, #116796 ) ;
#30360 = CIRCLE ( 'NONE', #26138, 0.06509327318403745899 ) ;
#30361 = FACE_OUTER_BOUND ( 'NONE', #88206, .T. ) ;
#30362 = DIRECTION ( 'NONE',  ( -0.000000000000000000, -1.000000000000000000, -0.000000000000000000 ) ) ;
#30363 = VERTEX_POINT ( 'NONE', #119533 ) ;
#30364 = CARTESIAN_POINT ( 'NONE',  ( -14.14999999999998792, 2.500000000000000000, 2.857883832488652853 ) ) ;
#30365 = ORIENTED_EDGE ( 'NONE', *, *, #16884, .F. ) ;
#30366 = DIRECTION ( 'NONE',  ( 0.000000000000000000, 1.000000000000000000, 0.000000000000000000 ) ) ;
#30367 = EDGE_LOOP ( 'NONE', ( #105560, #53504 ) ) ;
#30368 = CARTESIAN_POINT ( 'NONE',  ( 2.949999999999946887, 2.500000000000000000, -6.495190528383302464 ) ) ;
#30369 = DIRECTION ( 'NONE',  ( 0.000000000000000000, 1.000000000000000000, 0.000000000000000000 ) ) ;
#30370 = ORIENTED_EDGE ( 'NONE', *, *, #79852, .F. ) ;
#30371 = DIRECTION ( 'NONE',  ( -0.000000000000000000, -1.000000000000000000, -0.000000000000000000 ) ) ;
#30372 = DIRECTION ( 'NONE',  ( 0.000000000000000000, 0.000000000000000000, 1.000000000000000000 ) ) ;
#30373 = VERTEX_POINT ( 'NONE', #80275 ) ;
#30374 = EDGE_CURVE ( 'NONE', #56130, #93025, #108428, .T. ) ;
#30375 = VECTOR ( 'NONE', #60577, 1000.000000000000000 ) ;
#30377 = PLANE ( 'NONE',  #32073 ) ;
#30376 = AXIS2_PLACEMENT_3D ( 'NONE', #52098, #92015, #63201 ) ;
#30378 = ORIENTED_EDGE ( 'NONE', *, *, #39680, .T. ) ;
#30379 = AXIS2_PLACEMENT_3D ( 'NONE', #125135, #35472, #75370 ) ;
#30380 = EDGE_LOOP ( 'NONE', ( #54694, #14576 ) ) ;
#30381 = CARTESIAN_POINT ( 'NONE',  ( 1.049999999999954969, 12.50000000000000000, -6.776507416713039689 ) ) ;
#30382 = DIRECTION ( 'NONE',  ( 0.000000000000000000, 0.000000000000000000, -1.000000000000000000 ) ) ;
#30383 = ADVANCED_FACE ( 'NONE', ( #50181 ), #3106, .T. ) ;
#30384 = CARTESIAN_POINT ( 'NONE',  ( 184.8802083336747444, 4.367472073101515306, 7.564683531250000925 ) ) ;
#30385 = CARTESIAN_POINT ( 'NONE',  ( -11.25000000000000000, 2.500000000000000000, -7.288010851410851032 ) ) ;
#30386 = EDGE_CURVE ( 'NONE', #116756, #37559, #44878, .T. ) ;
#30387 = CIRCLE ( 'NONE', #15770, 0.1000000000000000472 ) ;
#30388 = CARTESIAN_POINT ( 'NONE',  ( 9.399999999999918643, 2.500000000000000000, -0.4464101615137782142 ) ) ;
#30389 = AXIS2_PLACEMENT_3D ( 'NONE', #22121, #42388, #82317 ) ;
#30390 = ORIENTED_EDGE ( 'NONE', *, *, #118706, .F. ) ;
#30391 = VECTOR ( 'NONE', #108094, 1000.000000000000000 ) ;
#30392 = FACE_OUTER_BOUND ( 'NONE', #98259, .T. ) ;
#30393 = EDGE_CURVE ( 'NONE', #51160, #81889, #21993, .T. ) ;
#30394 = CIRCLE ( 'NONE', #47113, 0.1000000000000000472 ) ;
#30395 = ADVANCED_FACE ( 'NONE', ( #48892 ), #128609, .T. ) ;
#30396 = EDGE_CURVE ( 'NONE', #73228, #59490, #38730, .T. ) ;
#30397 = ADVANCED_FACE ( 'NONE', ( #39080 ), #78996, .T. ) ;
#30398 = ORIENTED_EDGE ( 'NONE', *, *, #13330, .T. ) ;
#30399 = CONICAL_SURFACE ( 'NONE', #1119, 0.1000000000000002554, 0.003490658503988666988 ) ;
#30400 = DIRECTION ( 'NONE',  ( 0.000000000000000000, 0.000000000000000000, 1.000000000000000000 ) ) ;
#30402 = AXIS2_PLACEMENT_3D ( 'NONE', #14009, #4185, #83426 ) ;
#30401 = CARTESIAN_POINT ( 'NONE',  ( -4.550000000000026468, 2.500000000000000000, -6.495190528383302464 ) ) ;
#30403 = EDGE_CURVE ( 'NONE', #28942, #125792, #99275, .T. ) ;
#30404 = AXIS2_PLACEMENT_3D ( 'NONE', #6655, #39408, #109400 ) ;
#30405 = CARTESIAN_POINT ( 'NONE',  ( 186.3802083336747444, 4.367472073101515306, 7.564683531250000925 ) ) ;
#30406 = LINE ( 'NONE', #2848, #69896 ) ;
#30407 = FACE_OUTER_BOUND ( 'NONE', #91566, .T. ) ;
#30408 = DIRECTION ( 'NONE',  ( -0.000000000000000000, -1.000000000000000000, -0.000000000000000000 ) ) ;
#30409 = CARTESIAN_POINT ( 'NONE',  ( -0.8500000000000382805, 12.50000000000000000, -5.802370205355749988 ) ) ;
#30410 = ORIENTED_EDGE ( 'NONE', *, *, #65949, .F. ) ;
#30411 = EDGE_CURVE ( 'NONE', #112989, #25435, #89442, .T. ) ;
#30412 = DIRECTION ( 'NONE',  ( 0.000000000000000000, 1.000000000000000000, 0.000000000000000000 ) ) ;
#30413 = CARTESIAN_POINT ( 'NONE',  ( -5.850000000000021849, 2.500000000000000000, -7.288010851410854585 ) ) ;
#30414 = DIRECTION ( 'NONE',  ( -0.000000000000000000, 1.000000000000000000, -0.000000000000000000 ) ) ;
#30415 = AXIS2_PLACEMENT_3D ( 'NONE', #72792, #112718, #123799 ) ;
#30416 = ORIENTED_EDGE ( 'NONE', *, *, #80193, .T. ) ;
#30417 = DIRECTION ( 'NONE',  ( 0.000000000000000000, 0.000000000000000000, 1.000000000000000000 ) ) ;
#30418 = ORIENTED_EDGE ( 'NONE', *, *, #52848, .F. ) ;
#30419 = EDGE_LOOP ( 'NONE', ( #109081, #125694 ) ) ;
#30420 = DIRECTION ( 'NONE',  ( -0.000000000000000000, 1.000000000000000000, -0.000000000000000000 ) ) ;
#30421 = VECTOR ( 'NONE', #15130, 1000.000000000000000 ) ;
#30422 = ORIENTED_EDGE ( 'NONE', *, *, #104583, .F. ) ;
#30423 = B_SPLINE_CURVE_WITH_KNOTS ( 'NONE', 3,
 ( #87083, #117171, #17022, #56972, #7882, #96908, #27508, #47835, #67420, #107381, #17698, #122370 ),
 .UNSPECIFIED., .F., .F.,
 ( 4, 2, 2, 2, 2, 4 ),
 ( 4.337147489887063328E-18, 0.0006571239767409316418, 0.001314247953481858947, 0.002628495906963720496, 0.003942743860445582262, 0.005256991813927443594 ),
 .UNSPECIFIED. ) ;
#30424 = CARTESIAN_POINT ( 'NONE',  ( 11.69999999999990870, 2.500000000000000000, -4.330127018922201643 ) ) ;
#30425 = CARTESIAN_POINT ( 'NONE',  ( -10.00000000000000533, 2.500000000000000000, 0.6928203230275494784 ) ) ;
#30426 = CONICAL_SURFACE ( 'NONE', #34725, 0.1000000000000002554, 0.003490658503988666988 ) ;
#30427 = AXIS2_PLACEMENT_3D ( 'NONE', #69059, #67771, #28505 ) ;
#30428 = ORIENTED_EDGE ( 'NONE', *, *, #115736, .T. ) ;
#30429 = CARTESIAN_POINT ( 'NONE',  ( 4.999999999999936939, 2.500000000000000000, -0.6928203230275541413 ) ) ;
#30430 = DIRECTION ( 'NONE',  ( -0.000000000000000000, -1.000000000000000000, -0.000000000000000000 ) ) ;
#30431 = CARTESIAN_POINT ( 'NONE',  ( 16.32360635137687410, -2.500000000000000000, -4.874197684290930255 ) ) ;
#30432 = EDGE_CURVE ( 'NONE', #86599, #28690, #57484, .T. ) ;
#30433 = ORIENTED_EDGE ( 'NONE', *, *, #35685, .T. ) ;
#30434 = VECTOR ( 'NONE', #24283, 1000.000000000000000 ) ;
#30436 = ORIENTED_EDGE ( 'NONE', *, *, #31185, .T. ) ;
#30435 = EDGE_CURVE ( 'NONE', #84709, #103499, #14568, .T. ) ;
#30437 = CIRCLE ( 'NONE', #105640, 0.06509327318403745899 ) ;
#30438 = ORIENTED_EDGE ( 'NONE', *, *, #55722, .F. ) ;
#30439 = DIRECTION ( 'NONE',  ( 0.000000000000000000, 0.000000000000000000, 1.000000000000000000 ) ) ;
#30440 = PLANE ( 'NONE',  #66684 ) ;
#30441 = CARTESIAN_POINT ( 'NONE',  ( -11.64999999999999858, 2.500000000000000000, -1.472243186433546125 ) ) ;
#30442 = FACE_BOUND ( 'NONE', #76001, .T. ) ;
#30443 = EDGE_LOOP ( 'NONE', ( #44008, #5348 ) ) ;
#30444 = DIRECTION ( 'NONE',  ( -0.000000000000000000, 1.000000000000000000, -0.000000000000000000 ) ) ;
#30445 = DIRECTION ( 'NONE',  ( 0.000000000000000000, 0.000000000000000000, 1.000000000000000000 ) ) ;
#30446 = ORIENTED_EDGE ( 'NONE', *, *, #42899, .T. ) ;
#30447 = EDGE_CURVE ( 'NONE', #51458, #30363, #109803, .T. ) ;
#30448 = DIRECTION ( 'NONE',  ( -0.7336674352945157240, 0.000000000000000000, 0.6795087154616692438 ) ) ;
#30450 = CARTESIAN_POINT ( 'NONE',  ( -11.69999999999999929, 2.500000000000000000, -0.09999999999999827083 ) ) ;
#30449 = AXIS2_PLACEMENT_3D ( 'NONE', #13185, #105459, #125714 ) ;
#30451 = AXIS2_PLACEMENT_3D ( 'NONE', #27077, #58488, #78112 ) ;
#30452 = CARTESIAN_POINT ( 'NONE',  ( 5.849999999999934808, 2.500000000000000000, -5.902370205355750521 ) ) ;
#30453 = DIRECTION ( 'NONE',  ( 0.000000000000000000, 1.000000000000000000, 0.000000000000000000 ) ) ;
#30454 = CARTESIAN_POINT ( 'NONE',  ( -9.350000000000008527, 12.50000000000000000, -6.148780366869520897 ) ) ;
#30455 = CARTESIAN_POINT ( 'NONE',  ( -14.59999999999998366, 12.50000000000000000, -0.7579135962115894909 ) ) ;
#30456 = DIRECTION ( 'NONE',  ( 0.000000000000000000, 0.000000000000000000, 1.000000000000000000 ) ) ;
#30457 = ORIENTED_EDGE ( 'NONE', *, *, #50107, .F. ) ;
#30458 = ORIENTED_EDGE ( 'NONE', *, *, #51941, .F. ) ;
#30459 = AXIS2_PLACEMENT_3D ( 'NONE', #103886, #112424, #22768 ) ;
#30460 = EDGE_LOOP ( 'NONE', ( #16023, #45980, #111157, #33765 ) ) ;
#30461 = ORIENTED_EDGE ( 'NONE', *, *, #112660, .F. ) ;
#30462 = FACE_OUTER_BOUND ( 'NONE', #21897, .T. ) ;
#30463 = DIRECTION ( 'NONE',  ( 0.000000000000000000, 1.000000000000000000, 0.000000000000000000 ) ) ;
#30464 = EDGE_LOOP ( 'NONE', ( #559, #123221 ) ) ;
#30465 = FACE_BOUND ( 'NONE', #52281, .T. ) ;
#30466 = CIRCLE ( 'NONE', #65935, 0.06509327318403745899 ) ;
#30467 = DIRECTION ( 'NONE',  ( 0.000000000000000000, -0.000000000000000000, 1.000000000000000000 ) ) ;
#30468 = CARTESIAN_POINT ( 'NONE',  ( 5.849999999999931255, 2.500000000000000000, 2.757883832488649656 ) ) ;
#30469 = VECTOR ( 'NONE', #52661, 1000.000000000000000 ) ;
#30470 = DIRECTION ( 'NONE',  ( 0.000000000000000000, 1.000000000000000000, 0.000000000000000000 ) ) ;
#30471 = CIRCLE ( 'NONE', #49248, 0.1000000000000002554 ) ;
#30472 = DIRECTION ( 'NONE',  ( 0.000000000000000000, 0.000000000000000000, 1.000000000000000000 ) ) ;
#30473 = DIRECTION ( 'NONE',  ( 0.000000000000000000, 1.000000000000000000, 0.000000000000000000 ) ) ;
#30474 = DIRECTION ( 'NONE',  ( -4.274815082592931898E-19, -0.9999939076577903929, -0.003490651415223739937 ) ) ;
#30475 = CARTESIAN_POINT ( 'NONE',  ( -9.350000000000006750, 2.500000000000000000, -1.818653347947325916 ) ) ;
#30476 = DIRECTION ( 'NONE',  ( -0.000000000000000000, -1.000000000000000000, -0.000000000000000000 ) ) ;
#30477 = VERTEX_POINT ( 'NONE', #35526 ) ;
#30478 = CONICAL_SURFACE ( 'NONE', #24199, 0.09999999999999982514, 0.003490658503988666988 ) ;
#30479 = ORIENTED_EDGE ( 'NONE', *, *, #110647, .F. ) ;
#30480 = EDGE_CURVE ( 'NONE', #70719, #62448, #75424, .T. ) ;
#30481 = ORIENTED_EDGE ( 'NONE', *, *, #28178, .T. ) ;
#30482 = ORIENTED_EDGE ( 'NONE', *, *, #35063, .T. ) ;
#30483 = ORIENTED_EDGE ( 'NONE', *, *, #120664, .F. ) ;
#30484 = EDGE_LOOP ( 'NONE', ( #15835, #85447 ) ) ;
#30485 = CONICAL_SURFACE ( 'NONE', #63911, 0.1000000000000002554, 0.003490658503988666988 ) ;
#30486 = LINE ( 'NONE', #112894, #19149 ) ;
#30487 = CARTESIAN_POINT ( 'NONE',  ( 7.299999999999924327, 12.50000000000000000, 0.3464101615137735735 ) ) ;
#30488 = EDGE_LOOP ( 'NONE', ( #44519, #25932, #66090, #75890 ) ) ;
#30489 = CARTESIAN_POINT ( 'NONE',  ( 15.39999999999989022, 12.50000000000000000, -2.385244779468109755E-15 ) ) ;
#30490 = CIRCLE ( 'NONE', #45147, 0.06509327318403745899 ) ;
#30492 = EDGE_CURVE ( 'NONE', #25624, #120397, #95134, .T. ) ;
#30491 = VECTOR ( 'NONE', #40118, 1000.000000000000000 ) ;
#30493 = AXIS2_PLACEMENT_3D ( 'NONE', #49340, #19863, #31615 ) ;
#30494 = CARTESIAN_POINT ( 'NONE',  ( 20.37757664703730853, 0.6627606010239018852, 4.188167776336779724 ) ) ;
#30495 = CARTESIAN_POINT ( 'NONE',  ( 184.3177083336747160, 4.367472073101515306, 7.564683531250000925 ) ) ;
#30496 = CARTESIAN_POINT ( 'NONE',  ( -6.900000000000019007, 2.500000000000000000, -0.3464101615137783474 ) ) ;
#30498 = VECTOR ( 'NONE', #2653, 1000.000000000000000 ) ;
#30497 = DIRECTION ( 'NONE',  ( 0.000000000000000000, 1.000000000000000000, 0.000000000000000000 ) ) ;
#30499 = EDGE_CURVE ( 'NONE', #51256, #72103, #6036, .T. ) ;
#30500 = ADVANCED_FACE ( 'NONE', ( #31817 ), #107656, .T. ) ;
#30501 = VERTEX_POINT ( 'NONE', #81559 ) ;
#30502 = DIRECTION ( 'NONE',  ( -0.000000000000000000, 1.000000000000000000, -0.000000000000000000 ) ) ;
#30503 = EDGE_LOOP ( 'NONE', ( #16636, #70052 ) ) ;
#30504 = ORIENTED_EDGE ( 'NONE', *, *, #71243, .T. ) ;
#30505 = DIRECTION ( 'NONE',  ( -4.274815082592931898E-19, -0.9999939076577903929, -0.003490651415223739937 ) ) ;
#30506 = EDGE_CURVE ( 'NONE', #121812, #121834, #59662, .T. ) ;
#30507 = CARTESIAN_POINT ( 'NONE',  ( 11.04999999999991189, 12.50000000000000000, -2.576566944158915184 ) ) ;
#30508 = FACE_OUTER_BOUND ( 'NONE', #122318, .T. ) ;
#30509 = EDGE_CURVE ( 'NONE', #82230, #115626, #94419, .T. ) ;
#30510 = CONICAL_SURFACE ( 'NONE', #24227, 0.1000000000000002554, 0.003490658503988666988 ) ;
#30511 = ORIENTED_EDGE ( 'NONE', *, *, #37959, .T. ) ;
#30512 = ORIENTED_EDGE ( 'NONE', *, *, #96139, .T. ) ;
#30513 = FACE_OUTER_BOUND ( 'NONE', #116532, .T. ) ;
#30514 = CARTESIAN_POINT ( 'NONE',  ( -10.45000000000000107, 2.500000000000000000, 6.495190528383297135 ) ) ;
#30515 = CARTESIAN_POINT ( 'NONE',  ( 0.5999999999999560130, 2.500000000000000000, -3.883716857408426648 ) ) ;
#30516 = PLANE ( 'NONE',  #110908 ) ;
#30517 = EDGE_LOOP ( 'NONE', ( #66036, #43 ) ) ;
#30518 = DIRECTION ( 'NONE',  ( 0.000000000000000000, 0.000000000000000000, 1.000000000000000000 ) ) ;
#30519 = CONICAL_SURFACE ( 'NONE', #99462, 0.1000000000000002554, 0.003490658503988666988 ) ;
#30520 = AXIS2_PLACEMENT_3D ( 'NONE', #78088, #109480, #80014 ) ;
#30521 = ORIENTED_EDGE ( 'NONE', *, *, #116070, .T. ) ;
#30523 = CIRCLE ( 'NONE', #124588, 0.09999999999999982514 ) ;
#30522 = FACE_OUTER_BOUND ( 'NONE', #1583, .T. ) ;
#30524 = VERTEX_POINT ( 'NONE', #16496 ) ;
#30525 = CIRCLE ( 'NONE', #28454, 0.06509327318403745899 ) ;
#30526 = CARTESIAN_POINT ( 'NONE',  ( -10.20000000000000639, 12.50000000000000000, -3.983716857408421852 ) ) ;
#30527 = DIRECTION ( 'NONE',  ( 0.000000000000000000, 0.000000000000000000, 1.000000000000000000 ) ) ;
#30528 = LINE ( 'NONE', #20689, #36456 ) ;
#30529 = DIRECTION ( 'NONE',  ( -0.000000000000000000, -1.000000000000000000, -0.000000000000000000 ) ) ;
#30530 = VERTEX_POINT ( 'NONE', #115333 ) ;
#30531 = CIRCLE ( 'NONE', #11626, 0.06509327318403745899 ) ;
#30532 = FACE_OUTER_BOUND ( 'NONE', #32126, .T. ) ;
#30533 = AXIS2_PLACEMENT_3D ( 'NONE', #82630, #102885, #103556 ) ;
#30534 = CARTESIAN_POINT ( 'NONE',  ( -14.99999999999998401, 12.50000000000000000, 0.6928203230275518099 ) ) ;
#30535 = EDGE_LOOP ( 'NONE', ( #98104, #47737 ) ) ;
#30536 = ORIENTED_EDGE ( 'NONE', *, *, #98939, .T. ) ;
#30537 = ORIENTED_EDGE ( 'NONE', *, *, #3513, .T. ) ;
#30538 = DIRECTION ( 'NONE',  ( 0.000000000000000000, 0.000000000000000000, 1.000000000000000000 ) ) ;
#30539 = DIRECTION ( 'NONE',  ( 0.000000000000000000, 1.000000000000000000, 0.000000000000000000 ) ) ;
#30540 = DIRECTION ( 'NONE',  ( 0.000000000000000000, 0.000000000000000000, -1.000000000000000000 ) ) ;
#30541 = DIRECTION ( 'NONE',  ( -1.000000000000000000, -0.000000000000000000, -0.000000000000000000 ) ) ;
#30542 = DIRECTION ( 'NONE',  ( 0.000000000000000000, 0.000000000000000000, 1.000000000000000000 ) ) ;
#30543 = CARTESIAN_POINT ( 'NONE',  ( -8.350000000000013856, 12.50000000000000000, -5.802370205355744659 ) ) ;
#30544 = CIRCLE ( 'NONE', #90871, 0.1000000000000002554 ) ;
#30545 = AXIS2_PLACEMENT_3D ( 'NONE', #2761, #81338, #13215 ) ;
#30546 = DIRECTION ( 'NONE',  ( 0.000000000000000000, -0.000000000000000000, 1.000000000000000000 ) ) ;
#30547 = CARTESIAN_POINT ( 'NONE',  ( -6.250000000000019540, 12.50000000000000000, -2.792790559304616504 ) ) ;
#30548 = CARTESIAN_POINT ( 'NONE',  ( 6.049999999999934097, 2.500000000000000000, -6.248780366869526759 ) ) ;
#30549 = EDGE_CURVE ( 'NONE', #114181, #21644, #25683, .T. ) ;
#30550 = EDGE_CURVE ( 'NONE', #118813, #79023, #51236, .T. ) ;
#30551 = EDGE_CURVE ( 'NONE', #91650, #60027, #124383, .T. ) ;
#30552 = ADVANCED_FACE ( 'NONE', ( #64959 ), #82621, .T. ) ;
#30553 = ORIENTED_EDGE ( 'NONE', *, *, #18952, .F. ) ;
#30554 = EDGE_CURVE ( 'NONE', #34203, #80417, #88868, .T. ) ;
#30555 = DIRECTION ( 'NONE',  ( 0.000000000000000000, 0.000000000000000000, 1.000000000000000000 ) ) ;
#30556 = DIRECTION ( 'NONE',  ( 0.000000000000000000, 1.000000000000000000, 0.000000000000000000 ) ) ;
#30557 = CARTESIAN_POINT ( 'NONE',  ( -4.350000000000023626, 12.50000000000000000, -2.446380397790840266 ) ) ;
#30558 = DIRECTION ( 'NONE',  ( -0.000000000000000000, 1.000000000000000000, -0.000000000000000000 ) ) ;
#30559 = ORIENTED_EDGE ( 'NONE', *, *, #113168, .T. ) ;
#30560 = EDGE_CURVE ( 'NONE', #43603, #53182, #1040, .T. ) ;
#30561 = DIRECTION ( 'NONE',  ( 0.000000000000000000, 0.000000000000000000, 1.000000000000000000 ) ) ;
#30562 = EDGE_CURVE ( 'NONE', #46924, #96072, #53375, .T. ) ;
#30563 = AXIS2_PLACEMENT_3D ( 'NONE', #60431, #72813, #11941 ) ;
#30564 = AXIS2_PLACEMENT_3D ( 'NONE', #45834, #16338, #96197 ) ;
#30565 = CARTESIAN_POINT ( 'NONE',  ( -6.505213034913026604E-15, 2.500000000000000000, 4.330127018922196314 ) ) ;
#30567 = VERTEX_POINT ( 'NONE', #41658 ) ;
#30566 = CARTESIAN_POINT ( 'NONE',  ( -3.300000000000027800, 2.500000000000000000, 0.09999999999999772959 ) ) ;
#30568 = ORIENTED_EDGE ( 'NONE', *, *, #80383, .T. ) ;
#30569 = CONICAL_SURFACE ( 'NONE', #24286, 0.09999999999999982514, 0.003490658503988666988 ) ;
#30570 = FACE_OUTER_BOUND ( 'NONE', #36137, .T. ) ;
#30571 = ORIENTED_EDGE ( 'NONE', *, *, #35687, .T. ) ;
#30572 = VERTEX_POINT ( 'NONE', #85881 ) ;
#30573 = DIRECTION ( 'NONE',  ( 0.000000000000000000, -0.000000000000000000, 1.000000000000000000 ) ) ;
#30574 = CARTESIAN_POINT ( 'NONE',  ( 18.87984495337804347, 0.5408627091912223683, -4.542689527608963829 ) ) ;
#30575 = FACE_OUTER_BOUND ( 'NONE', #80956, .T. ) ;
#30576 = CIRCLE ( 'NONE', #39000, 0.1000000000000002554 ) ;
#30577 = DIRECTION ( 'NONE',  ( 0.000000000000000000, 0.000000000000000000, 1.000000000000000000 ) ) ;
#30578 = ORIENTED_EDGE ( 'NONE', *, *, #46470, .F. ) ;
#30579 = CIRCLE ( 'NONE', #126708, 0.06509327318403745899 ) ;
#30580 = PLANE ( 'NONE',  #23138 ) ;
#30581 = VERTEX_POINT ( 'NONE', #125807 ) ;
#30582 = CARTESIAN_POINT ( 'NONE',  ( 8.349999999999923261, 2.500000000000000000, -7.088010851410853519 ) ) ;
#30583 = DIRECTION ( 'NONE',  ( -0.000000000000000000, -1.000000000000000000, -0.000000000000000000 ) ) ;
#30584 = EDGE_CURVE ( 'NONE', #36319, #41518, #64326, .T. ) ;
#30585 = CARTESIAN_POINT ( 'NONE',  ( 17.10613367507967553, -2.036230694789212592, 5.376205058613408028 ) ) ;
#30586 = ORIENTED_EDGE ( 'NONE', *, *, #17167, .T. ) ;
#30587 = ORIENTED_EDGE ( 'NONE', *, *, #84611, .T. ) ;
#30588 = ORIENTED_EDGE ( 'NONE', *, *, #120786, .T. ) ;
#30589 = ORIENTED_EDGE ( 'NONE', *, *, #84984, .T. ) ;
#30590 = EDGE_LOOP ( 'NONE', ( #92254, #89348 ) ) ;
#30591 = LINE ( 'NONE', #61969, #62867 ) ;
#30592 = DIRECTION ( 'NONE',  ( -4.274815082592931898E-19, -0.9999939076577903929, -0.003490651415223739937 ) ) ;
#30593 = DIRECTION ( 'NONE',  ( -0.000000000000000000, -1.000000000000000000, -0.000000000000000000 ) ) ;
#30594 = FACE_BOUND ( 'NONE', #9947, .T. ) ;
#30595 = FACE_OUTER_BOUND ( 'NONE', #119200, .T. ) ;
#30596 = CONICAL_SURFACE ( 'NONE', #26469, 0.1000000000000000472, 0.003490658503988666988 ) ;
#30597 = FACE_OUTER_BOUND ( 'NONE', #120146, .T. ) ;
#30598 = FACE_OUTER_BOUND ( 'NONE', #44238, .T. ) ;
#30599 = DIRECTION ( 'NONE',  ( -0.000000000000000000, 1.000000000000000000, -0.000000000000000000 ) ) ;
#30600 = EDGE_CURVE ( 'NONE', #89491, #56415, #85257, .T. ) ;
#30601 = CIRCLE ( 'NONE', #118592, 0.1000000000000002554 ) ;
#30602 = LINE ( 'NONE', #89502, #25498 ) ;
#30603 = AXIS2_PLACEMENT_3D ( 'NONE', #45763, #35930, #22903 ) ;
#30604 = DIRECTION ( 'NONE',  ( 0.000000000000000000, 0.000000000000000000, 1.000000000000000000 ) ) ;
#30605 = DIRECTION ( 'NONE',  ( 0.000000000000000000, 0.000000000000000000, 1.000000000000000000 ) ) ;
#30606 = AXIS2_PLACEMENT_3D ( 'NONE', #109144, #119616, #99996 ) ;
#30607 = CIRCLE ( 'NONE', #120472, 0.06509327318403745899 ) ;
#30608 = CARTESIAN_POINT ( 'NONE',  ( 11.89999999999990798, 12.50000000000000000, -4.048810130592463530 ) ) ;
#30609 = CIRCLE ( 'NONE', #120475, 0.1000000000000002554 ) ;
#30610 = ORIENTED_EDGE ( 'NONE', *, *, #118435, .F. ) ;
#30611 = VERTEX_POINT ( 'NONE', #76726 ) ;
#30612 = ORIENTED_EDGE ( 'NONE', *, *, #58291, .T. ) ;
#30613 = ORIENTED_EDGE ( 'NONE', *, *, #27340, .T. ) ;
#30614 = CARTESIAN_POINT ( 'NONE',  ( -0.4000000000000401013, 12.50000000000000000, -3.637306695894650055 ) ) ;
#30615 = DIRECTION ( 'NONE',  ( 0.000000000000000000, 0.000000000000000000, -1.000000000000000000 ) ) ;
#30616 = FACE_BOUND ( 'NONE', #99031, .T. ) ;
#30618 = DIRECTION ( 'NONE',  ( 0.000000000000000000, 0.000000000000000000, 1.000000000000000000 ) ) ;
#30617 = AXIS2_PLACEMENT_3D ( 'NONE', #59418, #109784, #20113 ) ;
#30620 = CONICAL_SURFACE ( 'NONE', #103767, 0.1000000000000000472, 0.003490658503988666988 ) ;
#30619 = CONICAL_SURFACE ( 'NONE', #82850, 0.1000000000000002554, 0.003490658503988666988 ) ;
#30621 = EDGE_LOOP ( 'NONE', ( #7468, #65999, #21886, #73625 ) ) ;
#30622 = FACE_OUTER_BOUND ( 'NONE', #18504, .T. ) ;
#30623 = DIRECTION ( 'NONE',  ( 0.000000000000000000, 1.000000000000000000, 0.000000000000000000 ) ) ;
#30624 = DIRECTION ( 'NONE',  ( 0.000000000000000000, 0.000000000000000000, -1.000000000000000000 ) ) ;
#30625 = DIRECTION ( 'NONE',  ( 0.000000000000000000, 0.000000000000000000, -1.000000000000000000 ) ) ;
#30626 = ORIENTED_EDGE ( 'NONE', *, *, #17973, .T. ) ;
#30627 = CARTESIAN_POINT ( 'NONE',  ( -12.49999999999999289, 2.500000000000000000, -5.122947341949751987 ) ) ;
#30628 = ORIENTED_EDGE ( 'NONE', *, *, #44258, .F. ) ;
#30629 = EDGE_LOOP ( 'NONE', ( #116806, #35857 ) ) ;
#30630 = CARTESIAN_POINT ( 'NONE',  ( 12.89999999999990088, 2.500000000000000000, 4.330127018922196314 ) ) ;
#30631 = CARTESIAN_POINT ( 'NONE',  ( -1.250000000000001110, 12.50000000000000000, -2.099970236277064473 ) ) ;
#30632 = EDGE_LOOP ( 'NONE', ( #30683, #45576, #115214, #81854 ) ) ;
#30633 = DIRECTION ( 'NONE',  ( 0.000000000000000000, 1.000000000000000000, 0.000000000000000000 ) ) ;
#30634 = EDGE_CURVE ( 'NONE', #46379, #67379, #32471, .T. ) ;
#30635 = DIRECTION ( 'NONE',  ( -0.000000000000000000, -1.000000000000000000, -0.000000000000000000 ) ) ;
#30636 = FACE_OUTER_BOUND ( 'NONE', #69536, .T. ) ;
#30637 = DIRECTION ( 'NONE',  ( 0.000000000000000000, 0.000000000000000000, 1.000000000000000000 ) ) ;
#30638 = VERTEX_POINT ( 'NONE', #78010 ) ;
#30639 = EDGE_CURVE ( 'NONE', #7770, #120491, #57744, .T. ) ;
#30640 = DIRECTION ( 'NONE',  ( -0.000000000000000000, -1.000000000000000000, -0.000000000000000000 ) ) ;
#30641 = EDGE_CURVE ( 'NONE', #41537, #29412, #99343, .T. ) ;
#30642 = ORIENTED_EDGE ( 'NONE', *, *, #114868, .T. ) ;
#30643 = CARTESIAN_POINT ( 'NONE',  ( -1.900000000000034550, 2.500000000000000000, 4.676537180435972552 ) ) ;
#30644 = VERTEX_POINT ( 'NONE', #86540 ) ;
#30645 = VECTOR ( 'NONE', #98140, 1000.000000000000000 ) ;
#30646 = FACE_OUTER_BOUND ( 'NONE', #64338, .T. ) ;
#30647 = ORIENTED_EDGE ( 'NONE', *, *, #32747, .T. ) ;
#30648 = DIRECTION ( 'NONE',  ( 0.000000000000000000, 0.000000000000000000, -1.000000000000000000 ) ) ;
#30649 = CARTESIAN_POINT ( 'NONE',  ( -0.6000000000000323963, 2.500000000000000000, 0.4464101615137759382 ) ) ;
#30650 = EDGE_CURVE ( 'NONE', #109098, #112569, #89123, .T. ) ;
#30651 = ADVANCED_FACE ( 'NONE', ( #26992 ), #19923, .T. ) ;
#30652 = DIRECTION ( 'NONE',  ( -0.000000000000000000, -1.000000000000000000, -0.000000000000000000 ) ) ;
#30653 = EDGE_CURVE ( 'NONE', #79005, #95802, #44966, .T. ) ;
#30654 = DIRECTION ( 'NONE',  ( -4.274815082592931898E-19, -0.9999939076577903929, -0.003490651415223739937 ) ) ;
#30655 = EDGE_CURVE ( 'NONE', #5036, #115994, #93085, .T. ) ;
#30656 = EDGE_CURVE ( 'NONE', #119339, #111925, #19069, .T. ) ;
#30657 = DIRECTION ( 'NONE',  ( 0.000000000000000000, -0.000000000000000000, 1.000000000000000000 ) ) ;
#30658 = VERTEX_POINT ( 'NONE', #29557 ) ;
#30661 = ORIENTED_EDGE ( 'NONE', *, *, #97923, .F. ) ;
#30660 = AXIS2_PLACEMENT_3D ( 'NONE', #56010, #78751, #146 ) ;
#30659 = CIRCLE ( 'NONE', #68280, 0.06509327318403745899 ) ;
#30662 = ORIENTED_EDGE ( 'NONE', *, *, #1546, .T. ) ;
#30663 = CARTESIAN_POINT ( 'NONE',  ( -2.700000000000030820, 2.500000000000000000, 0.4464101615137735513 ) ) ;
#30664 = DIRECTION ( 'NONE',  ( -0.000000000000000000, 1.000000000000000000, -0.000000000000000000 ) ) ;
#30665 = CARTESIAN_POINT ( 'NONE',  ( 108.0000000000000142, 5.855766388782936538, -5.000000000000004441 ) ) ;
#30667 = ORIENTED_EDGE ( 'NONE', *, *, #78717, .F. ) ;
#30666 = EDGE_LOOP ( 'NONE', ( #96628, #34839, #19452, #126456 ) ) ;
#30668 = VERTEX_POINT ( 'NONE', #36814 ) ;
#30669 = ADVANCED_FACE ( 'NONE', ( #27603 ), #5235, .T. ) ;
#30670 = CARTESIAN_POINT ( 'NONE',  ( -6.850000000000017408, 12.50000000000000000, -2.446380397790840266 ) ) ;
#30672 = AXIS2_PLACEMENT_3D ( 'NONE', #111366, #1425, #92382 ) ;
#30671 = CIRCLE ( 'NONE', #122676, 0.06509327318403745899 ) ;
#30673 = ORIENTED_EDGE ( 'NONE', *, *, #87344, .T. ) ;
#30674 = CARTESIAN_POINT ( 'NONE',  ( -7.700000000000016165, 2.500000000000000000, -3.983716857408426293 ) ) ;
#30675 = AXIS2_PLACEMENT_3D ( 'NONE', #126282, #37891, #97459 ) ;
#30676 = DIRECTION ( 'NONE',  ( 0.000000000000000000, 0.000000000000000000, 1.000000000000000000 ) ) ;
#30677 = DIRECTION ( 'NONE',  ( -0.000000000000000000, 1.000000000000000000, -0.000000000000000000 ) ) ;
#30678 = CARTESIAN_POINT ( 'NONE',  ( -3.750000000000025757, 2.500000000000000000, -2.857883832488653741 ) ) ;
#30679 = LINE ( 'NONE', #10996, #57637 ) ;
#30680 = DIRECTION ( 'NONE',  ( -0.000000000000000000, 1.000000000000000000, -0.000000000000000000 ) ) ;
#30681 = DIRECTION ( 'NONE',  ( -0.000000000000000000, -1.000000000000000000, -0.000000000000000000 ) ) ;
#30682 = VERTEX_POINT ( 'NONE', #119226 ) ;
#30683 = ORIENTED_EDGE ( 'NONE', *, *, #9016, .T. ) ;
#30684 = CARTESIAN_POINT ( 'NONE',  ( 0.1999999999999562961, 12.50000000000000000, 4.611443907251934426 ) ) ;
#30685 = CARTESIAN_POINT ( 'NONE',  ( 4.399999999999940847, 12.50000000000000000, -4.676537180435977881 ) ) ;
#30686 = EDGE_LOOP ( 'NONE', ( #63549, #119398, #71516, #120626 ) ) ;
#30687 = ORIENTED_EDGE ( 'NONE', *, *, #103374, .F. ) ;
#30688 = CARTESIAN_POINT ( 'NONE',  ( 185.4843750003414300, -8.734944146203032389, -1.604583208406768146E-15 ) ) ;
#30689 = CARTESIAN_POINT ( 'NONE',  ( 14.39999999999989555, 2.500000000000000000, 0.3464101615137736845 ) ) ;
#30690 = VECTOR ( 'NONE', #125443, 1000.000000000000000 ) ;
#30691 = FACE_OUTER_BOUND ( 'NONE', #82948, .T. ) ;
#30693 = CIRCLE ( 'NONE', #26471, 0.1000000000000002554 ) ;
#30692 = DIRECTION ( 'NONE',  ( 0.000000000000000000, 1.000000000000000000, 0.000000000000000000 ) ) ;
#30694 = CARTESIAN_POINT ( 'NONE',  ( -1.250000000000037526, 12.50000000000000000, -1.537336459617587581 ) ) ;
#30695 = FACE_OUTER_BOUND ( 'NONE', #43984, .T. ) ;
#30696 = AXIS2_PLACEMENT_3D ( 'NONE', #111543, #90605, #946 ) ;
#30697 = CARTESIAN_POINT ( 'NONE',  ( 7.099999999999927702, 12.50000000000000000, -3.572213422710612374 ) ) ;
#30698 = DIRECTION ( 'NONE',  ( 0.000000000000000000, 1.000000000000000000, 0.000000000000000000 ) ) ;
#30699 = ADVANCED_FACE ( 'NONE', ( #107476 ), #97007, .T. ) ;
#30700 = AXIS2_PLACEMENT_3D ( 'NONE', #38349, #128003, #66494 ) ;
#30701 = ADVANCED_FACE ( 'NONE', ( #47278 ), #7375, .T. ) ;
#30702 = AXIS2_PLACEMENT_3D ( 'NONE', #58144, #88202, #18841 ) ;
#30703 = LINE ( 'NONE', #11677, #83509 ) ;
#30704 = ORIENTED_EDGE ( 'NONE', *, *, #50894, .F. ) ;
#30705 = ORIENTED_EDGE ( 'NONE', *, *, #123478, .F. ) ;
#30706 = AXIS2_PLACEMENT_3D ( 'NONE', #91722, #91074, #89786 ) ;
#30707 = ADVANCED_FACE ( 'NONE', ( #98286 ), #47199, .T. ) ;
#30708 = EDGE_LOOP ( 'NONE', ( #38069, #108944 ) ) ;
#30709 = ORIENTED_EDGE ( 'NONE', *, *, #86204, .F. ) ;
#30710 = CIRCLE ( 'NONE', #7683, 0.09999999999999999167 ) ;
#30711 = EDGE_CURVE ( 'NONE', #40465, #25579, #8602, .T. ) ;
#30712 = EDGE_LOOP ( 'NONE', ( #129094, #8180 ) ) ;
#30713 = FACE_OUTER_BOUND ( 'NONE', #111699, .T. ) ;
#30714 = DIRECTION ( 'NONE',  ( 0.000000000000000000, 1.000000000000000000, 0.000000000000000000 ) ) ;
#30715 = CIRCLE ( 'NONE', #41088, 0.06509327318403745899 ) ;
#30716 = EDGE_CURVE ( 'NONE', #127948, #48914, #48562, .T. ) ;
#30717 = ORIENTED_EDGE ( 'NONE', *, *, #52066, .F. ) ;
#30718 = EDGE_CURVE ( 'NONE', #62072, #11437, #128431, .T. ) ;
#30719 = FACE_OUTER_BOUND ( 'NONE', #64753, .T. ) ;
#30720 = DIRECTION ( 'NONE',  ( -0.000000000000000000, -1.000000000000000000, -0.000000000000000000 ) ) ;
#30723 = EDGE_CURVE ( 'NONE', #67433, #52089, #28274, .T. ) ;
#30722 = VECTOR ( 'NONE', #93571, 1000.000000000000000 ) ;
#30721 = CIRCLE ( 'NONE', #26498, 0.1000000000000000056 ) ;
#30724 = DIRECTION ( 'NONE',  ( 0.000000000000000000, -0.9999939076577903929, 0.003490651415223739937 ) ) ;
#30726 = EDGE_LOOP ( 'NONE', ( #39797, #104361 ) ) ;
#30725 = CARTESIAN_POINT ( 'NONE',  ( -8.350000000000013856, 2.500000000000000000, 2.265063509461097357 ) ) ;
#30727 = CARTESIAN_POINT ( 'NONE',  ( 5.199999999999931788, 2.500000000000000000, 4.676537180435972552 ) ) ;
#30728 = ADVANCED_FACE ( 'NONE', ( #69469 ), #72253, .T. ) ;
#30729 = CARTESIAN_POINT ( 'NONE',  ( -3.550000000000027800, 2.500000000000000000, 6.248780366869520542 ) ) ;
#30730 = EDGE_LOOP ( 'NONE', ( #14069, #28254 ) ) ;
#30731 = ORIENTED_EDGE ( 'NONE', *, *, #40337, .T. ) ;
#30732 = EDGE_LOOP ( 'NONE', ( #45937, #111915, #128542, #5804 ) ) ;
#30733 = ORIENTED_EDGE ( 'NONE', *, *, #104925, .T. ) ;
#30734 = CARTESIAN_POINT ( 'NONE',  ( -10.65000000000000391, 2.500000000000000000, -6.148780366869522673 ) ) ;
#30735 = CIRCLE ( 'NONE', #13966, 0.06509327318403741736 ) ;
#30736 = DIRECTION ( 'NONE',  ( -4.274815082592931898E-19, -0.9999939076577903929, -0.003490651415223739937 ) ) ;
#30737 = CARTESIAN_POINT ( 'NONE',  ( 7.499999999999960032, 2.500000000000000000, -2.276824562219559311E-15 ) ) ;
#30738 = CARTESIAN_POINT ( 'NONE',  ( -8.350000000000013856, 2.500000000000000000, -2.065063509461102065 ) ) ;
#30739 = ORIENTED_EDGE ( 'NONE', *, *, #27456, .T. ) ;
#30740 = CARTESIAN_POINT ( 'NONE',  ( -1.700000000000034817, 12.50000000000000000, 0.06509327318403504425 ) ) ;
#30741 = CARTESIAN_POINT ( 'NONE',  ( 18.29531403502781828, -0.5011766475904796403, -4.780851392375756070 ) ) ;
#30742 = LINE ( 'NONE', #70639, #94378 ) ;
#30743 = CARTESIAN_POINT ( 'NONE',  ( -11.44999999999999751, 2.500000000000000000, 1.918653347947321564 ) ) ;
#30744 = ADVANCED_FACE ( 'NONE', ( #100238 ), #55516, .T. ) ;
#30745 = VERTEX_POINT ( 'NONE', #80601 ) ;
#30746 = CIRCLE ( 'NONE', #124816, 4.500000000000003553 ) ;
#30747 = CARTESIAN_POINT ( 'NONE',  ( 6.049999999999935874, 12.50000000000000000, -6.841600689897077814 ) ) ;
#30748 = CONICAL_SURFACE ( 'NONE', #106032, 0.1000000000000000472, 0.003490658503988666988 ) ;
#30749 = ORIENTED_EDGE ( 'NONE', *, *, #92853, .T. ) ;
#30750 = VERTEX_POINT ( 'NONE', #102169 ) ;
#30751 = CARTESIAN_POINT ( 'NONE',  ( 6.699999999999930012, 12.50000000000000000, 4.265033745738159077 ) ) ;
#30752 = DIRECTION ( 'NONE',  ( 0.000000000000000000, 0.000000000000000000, -1.000000000000000000 ) ) ;
#30753 = FACE_BOUND ( 'NONE', #7270, .T. ) ;
#30754 = CARTESIAN_POINT ( 'NONE',  ( -10.80000000000000071, 2.500000000000000000, 4.230127018922196669 ) ) ;
#30755 = DIRECTION ( 'NONE',  ( 0.000000000000000000, 0.000000000000000000, -1.000000000000000000 ) ) ;
#30756 = CIRCLE ( 'NONE', #93428, 0.06509327318403745899 ) ;
#30757 = CARTESIAN_POINT ( 'NONE',  ( 13.29999999999989946, 2.500000000000000000, -0.1000000000000023925 ) ) ;
#30758 = EDGE_CURVE ( 'NONE', #110183, #99983, #100862, .T. ) ;
#30759 = DIRECTION ( 'NONE',  ( -0.000000000000000000, -1.000000000000000000, -0.000000000000000000 ) ) ;
#30760 = DIRECTION ( 'NONE',  ( 0.000000000000000000, 1.000000000000000000, 0.000000000000000000 ) ) ;
#30761 = CARTESIAN_POINT ( 'NONE',  ( -6.450000000000017941, 2.500000000000000000, -2.511473670974877948 ) ) ;
#30762 = ORIENTED_EDGE ( 'NONE', *, *, #30509, .F. ) ;
#30764 = CONICAL_SURFACE ( 'NONE', #103903, 0.09999999999999982514, 0.003490658503988666988 ) ;
#30763 = AXIS2_PLACEMENT_3D ( 'NONE', #90740, #12161, #111677 ) ;
#30765 = CARTESIAN_POINT ( 'NONE',  ( 5.649999999999932854, 2.500000000000000000, 1.718653347947321386 ) ) ;
#30766 = VECTOR ( 'NONE', #22576, 1000.000000000000000 ) ;
#30767 = DIRECTION ( 'NONE',  ( -4.274815082592931898E-19, -0.9999939076577903929, -0.003490651415223739937 ) ) ;
#30768 = ORIENTED_EDGE ( 'NONE', *, *, #9231, .F. ) ;
#30769 = ORIENTED_EDGE ( 'NONE', *, *, #28645, .F. ) ;
#30770 = CARTESIAN_POINT ( 'NONE',  ( -4.150000000000025224, 2.500000000000000000, -1.472243186433550122 ) ) ;
#30771 = EDGE_CURVE ( 'NONE', #37867, #81193, #126628, .T. ) ;
#30772 = FACE_OUTER_BOUND ( 'NONE', #76910, .T. ) ;
#30773 = FACE_BOUND ( 'NONE', #7015, .T. ) ;
#30774 = DIRECTION ( 'NONE',  ( 0.000000000000000000, 0.000000000000000000, 1.000000000000000000 ) ) ;
#30775 = DIRECTION ( 'NONE',  ( 0.000000000000000000, 1.000000000000000000, 0.000000000000000000 ) ) ;
#30776 = EDGE_LOOP ( 'NONE', ( #26143, #26240, #4321, #117650 ) ) ;
#30777 = DIRECTION ( 'NONE',  ( 0.000000000000000000, 1.000000000000000000, 0.000000000000000000 ) ) ;
#30778 = CARTESIAN_POINT ( 'NONE',  ( 184.1250000000000284, -8.891194145520236347, -1.633285867636356693E-15 ) ) ;
#30779 = CIRCLE ( 'NONE', #93457, 0.09999999999999999167 ) ;
#30780 = ORIENTED_EDGE ( 'NONE', *, *, #108452, .T. ) ;
#30781 = DIRECTION ( 'NONE',  ( 0.000000000000000000, -0.000000000000000000, 1.000000000000000000 ) ) ;
#30782 = AXIS2_PLACEMENT_3D ( 'NONE', #125742, #24353, #95665 ) ;
#30783 = LINE ( 'NONE', #70686, #7326 ) ;
#30784 = AXIS2_PLACEMENT_3D ( 'NONE', #86584, #95133, #96397 ) ;
#30785 = LINE ( 'NONE', #61530, #69488 ) ;
#30786 = FACE_OUTER_BOUND ( 'NONE', #18603, .T. ) ;
#30787 = AXIS2_PLACEMENT_3D ( 'NONE', #48816, #89998, #58635 ) ;
#30788 = AXIS2_PLACEMENT_3D ( 'NONE', #126722, #36424, #75666 ) ;
#30789 = VERTEX_POINT ( 'NONE', #91703 ) ;
#30790 = EDGE_CURVE ( 'NONE', #53425, #77768, #111961, .T. ) ;
#30791 = DIRECTION ( 'NONE',  ( -0.000000000000000000, 1.000000000000000000, -0.000000000000000000 ) ) ;
#30792 = DIRECTION ( 'NONE',  ( 0.000000000000000000, -0.000000000000000000, 1.000000000000000000 ) ) ;
#30793 = DIRECTION ( 'NONE',  ( 0.000000000000000000, 0.000000000000000000, 1.000000000000000000 ) ) ;
#30794 = ORIENTED_EDGE ( 'NONE', *, *, #122112, .T. ) ;
#30795 = EDGE_LOOP ( 'NONE', ( #111399, #16255, #125117, #78612 ) ) ;
#30796 = AXIS2_PLACEMENT_3D ( 'NONE', #128205, #78476, #1812 ) ;
#30797 = DIRECTION ( 'NONE',  ( 0.000000000000000000, -0.000000000000000000, 1.000000000000000000 ) ) ;
#30798 = ADVANCED_FACE ( 'NONE', ( #70139 ), #12488, .T. ) ;
#30799 = ORIENTED_EDGE ( 'NONE', *, *, #20561, .T. ) ;
#30800 = CARTESIAN_POINT ( 'NONE',  ( 11.04999999999991012, 2.500000000000000000, -1.818653347947326138 ) ) ;
#30801 = CARTESIAN_POINT ( 'NONE',  ( 17.50000000000000000, -2.499999999999999556, 1.666666666666671404 ) ) ;
#30803 = AXIS2_PLACEMENT_3D ( 'NONE', #24027, #83595, #93407 ) ;
#30802 = CONICAL_SURFACE ( 'NONE', #45473, 0.09999999999999982514, 0.003490658503988666988 ) ;
#30804 = FACE_OUTER_BOUND ( 'NONE', #72370, .T. ) ;
#30805 = ORIENTED_EDGE ( 'NONE', *, *, #59949, .T. ) ;
#30806 = CARTESIAN_POINT ( 'NONE',  ( 6.249999999999932498, 2.500000000000000000, -5.802370205355749988 ) ) ;
#30807 = DIRECTION ( 'NONE',  ( 0.000000000000000000, -0.000000000000000000, 1.000000000000000000 ) ) ;
#30808 = DIRECTION ( 'NONE',  ( 0.000000000000000000, 0.000000000000000000, 1.000000000000000000 ) ) ;
#30809 = EDGE_CURVE ( 'NONE', #84669, #83875, #32155, .T. ) ;
#30810 = EDGE_CURVE ( 'NONE', #109919, #125301, #31494, .T. ) ;
#30811 = CARTESIAN_POINT ( 'NONE',  ( 14.14999999999989733, 2.500000000000000000, 1.572243186433545548 ) ) ;
#30812 = FACE_OUTER_BOUND ( 'NONE', #44043, .T. ) ;
#30813 = ADVANCED_FACE ( 'NONE', ( #40033 ), #88965, .T. ) ;
#30814 = ADVANCED_FACE ( 'NONE', ( #60944 ), #11192, .T. ) ;
#30815 = CARTESIAN_POINT ( 'NONE',  ( 9.399999999999918643, 12.50000000000000000, 0.3464101615137736845 ) ) ;
#30816 = VERTEX_POINT ( 'NONE', #30868 ) ;
#30817 = ORIENTED_EDGE ( 'NONE', *, *, #18722, .T. ) ;
#30818 = DIRECTION ( 'NONE',  ( 0.000000000000000000, 0.000000000000000000, -1.000000000000000000 ) ) ;
#30819 = EDGE_LOOP ( 'NONE', ( #77201, #43194 ) ) ;
#30820 = CARTESIAN_POINT ( 'NONE',  ( 103.7759110461913821, 7.219941590808979015, 2.680022258956899162 ) ) ;
#30822 = ORIENTED_EDGE ( 'NONE', *, *, #102735, .F. ) ;
#30821 = ORIENTED_EDGE ( 'NONE', *, *, #42569, .F. ) ;
#30823 = EDGE_LOOP ( 'NONE', ( #79565, #9419 ) ) ;
#30825 = ADVANCED_FACE ( 'NONE', ( #72077 ), #101492, .T. ) ;
#30824 = AXIS2_PLACEMENT_3D ( 'NONE', #69750, #59965, #109685 ) ;
#30826 = CARTESIAN_POINT ( 'NONE',  ( 17.50000000000000000, -2.083333333333331705, -3.999999999999998224 ) ) ;
#30827 = ADVANCED_FACE ( 'NONE', ( #101525 ), #7475, .T. ) ;
#30828 = DIRECTION ( 'NONE',  ( 0.000000000000000000, 1.846105847067148022E-16, -1.000000000000000000 ) ) ;
#30829 = ADVANCED_FACE ( 'NONE', ( #41964 ), #40887, .T. ) ;
#30830 = DIRECTION ( 'NONE',  ( -0.000000000000000000, -1.000000000000000000, -0.000000000000000000 ) ) ;
#30831 = CARTESIAN_POINT ( 'NONE',  ( 14.14999999999989733, 2.500000000000000000, 1.372243186433545370 ) ) ;
#30832 = DIRECTION ( 'NONE',  ( 0.000000000000000000, -0.000000000000000000, 1.000000000000000000 ) ) ;
#30833 = CARTESIAN_POINT ( 'NONE',  ( -10.40000000000000391, 12.50000000000000000, -3.637306695894645614 ) ) ;
#30834 = CARTESIAN_POINT ( 'NONE',  ( -1.450000000000035927, 2.500000000000000000, -1.918653347947326004 ) ) ;
#30835 = DIRECTION ( 'NONE',  ( -0.000000000000000000, -1.000000000000000000, -0.000000000000000000 ) ) ;
#30836 = CARTESIAN_POINT ( 'NONE',  ( 5.649999999999934630, 12.50000000000000000, -1.818653347947325916 ) ) ;
#30838 = ORIENTED_EDGE ( 'NONE', *, *, #112833, .T. ) ;
#30837 = CIRCLE ( 'NONE', #114425, 0.1000000000000000056 ) ;
#30839 = DIRECTION ( 'NONE',  ( 0.000000000000000000, 1.000000000000000000, 0.000000000000000000 ) ) ;
#30840 = ORIENTED_EDGE ( 'NONE', *, *, #86199, .T. ) ;
#30841 = VERTEX_POINT ( 'NONE', #36011 ) ;
#30842 = DIRECTION ( 'NONE',  ( 0.000000000000000000, 0.000000000000000000, -1.000000000000000000 ) ) ;
#30843 = CARTESIAN_POINT ( 'NONE',  ( -2.050000000000032685, 2.500000000000000000, -2.265063509461101798 ) ) ;
#30845 = CIRCLE ( 'NONE', #35052, 0.06509327318403745899 ) ;
#30844 = VECTOR ( 'NONE', #56141, 1000.000000000000000 ) ;
#30846 = VECTOR ( 'NONE', #50595, 1000.000000000000000 ) ;
#30847 = DIRECTION ( 'NONE',  ( 0.000000000000000000, 1.000000000000000000, 0.000000000000000000 ) ) ;
#30848 = DIRECTION ( 'NONE',  ( 0.000000000000000000, -0.9999939076577903929, 0.003490651415223739937 ) ) ;
#30849 = DIRECTION ( 'NONE',  ( 0.000000000000000000, -0.9999939076577903929, 0.003490651415223739937 ) ) ;
#30850 = EDGE_LOOP ( 'NONE', ( #54743, #44688 ) ) ;
#30851 = CIRCLE ( 'NONE', #107905, 0.09999999999999982514 ) ;
#30852 = VERTEX_POINT ( 'NONE', #115174 ) ;
#30853 = CARTESIAN_POINT ( 'NONE',  ( 16.56576425165006228, 1.499999999999999556, -6.084390597445811011 ) ) ;
#30854 = CONICAL_SURFACE ( 'NONE', #14092, 0.1000000000000002554, 0.003490658503988666988 ) ;
#30855 = ORIENTED_EDGE ( 'NONE', *, *, #117507, .T. ) ;
#30856 = CARTESIAN_POINT ( 'NONE',  ( 186.2916666666666288, 4.445597072760091528, -7.700000000000049916 ) ) ;
#30857 = ORIENTED_EDGE ( 'NONE', *, *, #14444, .T. ) ;
#30858 = EDGE_CURVE ( 'NONE', #121003, #126895, #91023, .T. ) ;
#30859 = EDGE_LOOP ( 'NONE', ( #34789, #90128, #57327, #60338 ) ) ;
#30860 = CARTESIAN_POINT ( 'NONE',  ( 13.09999999999989839, 12.50000000000000000, -0.4115034346978157509 ) ) ;
#30861 = DIRECTION ( 'NONE',  ( 0.000000000000000000, 0.000000000000000000, 1.000000000000000000 ) ) ;
#30862 = ADVANCED_FACE ( 'NONE', ( #44530 ), #83182, .T. ) ;
#30863 = AXIS2_PLACEMENT_3D ( 'NONE', #94516, #116096, #46078 ) ;
#30864 = FACE_OUTER_BOUND ( 'NONE', #125415, .T. ) ;
#30865 = DIRECTION ( 'NONE',  ( 0.000000000000000000, -0.9999939076577903929, 0.003490651415223739937 ) ) ;
#30866 = EDGE_CURVE ( 'NONE', #116963, #43630, #102792, .T. ) ;
#30867 = AXIS2_PLACEMENT_3D ( 'NONE', #16610, #76201, #65062 ) ;
#30868 = CARTESIAN_POINT ( 'NONE',  ( 3.749999999999942268, 2.500000000000000000, 1.572243186433545548 ) ) ;
#30869 = ORIENTED_EDGE ( 'NONE', *, *, #123626, .F. ) ;
#30870 = FACE_OUTER_BOUND ( 'NONE', #85760, .T. ) ;
#30871 = DIRECTION ( 'NONE',  ( 0.000000000000000000, 0.000000000000000000, 1.000000000000000000 ) ) ;
#30872 = CARTESIAN_POINT ( 'NONE',  ( 17.49862860983167323, 2.500000000000000000, -4.081131818001370704 ) ) ;
#30873 = CARTESIAN_POINT ( 'NONE',  ( -14.79999999999998295, 2.500000000000000000, -0.4464101615137760493 ) ) ;
#30874 = AXIS2_PLACEMENT_3D ( 'NONE', #114491, #24832, #64747 ) ;
#30875 = AXIS2_PLACEMENT_3D ( 'NONE', #98006, #118941, #29286 ) ;
#30876 = EDGE_CURVE ( 'NONE', #94676, #56167, #83805, .T. ) ;
#30877 = DIRECTION ( 'NONE',  ( 0.000000000000000000, 0.000000000000000000, 1.000000000000000000 ) ) ;
#30878 = ORIENTED_EDGE ( 'NONE', *, *, #55924, .F. ) ;
#30879 = CIRCLE ( 'NONE', #16159, 0.06509327318403745899 ) ;
#30880 = VERTEX_POINT ( 'NONE', #113926 ) ;
#30881 = CARTESIAN_POINT ( 'NONE',  ( -7.100000000000017408, 2.500000000000000000, 0.6928203230275494784 ) ) ;
#30882 = CIRCLE ( 'NONE', #7860, 0.1000000000000002554 ) ;
#30883 = EDGE_CURVE ( 'NONE', #118717, #9579, #3285, .T. ) ;
#30884 = ORIENTED_EDGE ( 'NONE', *, *, #8713, .F. ) ;
#30885 = CIRCLE ( 'NONE', #76844, 0.06509327318403745899 ) ;
#30886 = CARTESIAN_POINT ( 'NONE',  ( -14.59999999999998366, 2.500000000000000000, -0.5928203230275519431 ) ) ;
#30887 = CARTESIAN_POINT ( 'NONE',  ( -6.650000000000014566, 2.500000000000000000, 2.165063509461097713 ) ) ;
#30888 = CIRCLE ( 'NONE', #70574, 0.1000000000000002554 ) ;
#30889 = ORIENTED_EDGE ( 'NONE', *, *, #40005, .F. ) ;
#30890 = CARTESIAN_POINT ( 'NONE',  ( -3.750000000000025757, 2.500000000000000000, 1.572243186433545548 ) ) ;
#30892 = CONICAL_SURFACE ( 'NONE', #87295, 0.09999999999999982514, 0.003490658503988666988 ) ;
#30891 = DIRECTION ( 'NONE',  ( -0.000000000000000000, -1.000000000000000000, -0.000000000000000000 ) ) ;
#30893 = CARTESIAN_POINT ( 'NONE',  ( 11.84999999999990372, 2.500000000000000000, -6.941600689897078347 ) ) ;
#30894 = EDGE_CURVE ( 'NONE', #6638, #74055, #118207, .T. ) ;
#30895 = DIRECTION ( 'NONE',  ( 0.000000000000000000, 0.000000000000000000, -1.000000000000000000 ) ) ;
#30896 = AXIS2_PLACEMENT_3D ( 'NONE', #30489, #40295, #48172 ) ;
#30897 = DIRECTION ( 'NONE',  ( -0.000000000000000000, 1.000000000000000000, -0.000000000000000000 ) ) ;
#30898 = ORIENTED_EDGE ( 'NONE', *, *, #31523, .F. ) ;
#30899 = CARTESIAN_POINT ( 'NONE',  ( 8.749999999999921840, 2.500000000000000000, -5.702370205355749455 ) ) ;
#30900 = CARTESIAN_POINT ( 'NONE',  ( -3.150000000000029665, 2.500000000000000000, 6.741600689897071952 ) ) ;
#30901 = DIRECTION ( 'NONE',  ( -4.274815082592931898E-19, -0.9999939076577903929, -0.003490651415223739937 ) ) ;
#30902 = DIRECTION ( 'NONE',  ( -4.274815082592931898E-19, -0.9999939076577903929, -0.003490651415223739937 ) ) ;
#30903 = ORIENTED_EDGE ( 'NONE', *, *, #89775, .F. ) ;
#30904 = ADVANCED_FACE ( 'NONE', ( #64811 ), #51330, .T. ) ;
#30905 = ORIENTED_EDGE ( 'NONE', *, *, #56407, .F. ) ;
#30906 = DIRECTION ( 'NONE',  ( -1.000000000000000000, 0.000000000000000000, 0.000000000000000000 ) ) ;
#30907 = CARTESIAN_POINT ( 'NONE',  ( 5.599999999999934808, 12.50000000000000000, -3.983716857408426293 ) ) ;
#30908 = CIRCLE ( 'NONE', #37164, 0.06509327318403745899 ) ;
#30909 = CARTESIAN_POINT ( 'NONE',  ( -2.050000000000032685, 2.500000000000000000, -6.495190528383302464 ) ) ;
#30910 = ORIENTED_EDGE ( 'NONE', *, *, #117199, .T. ) ;
#30911 = CARTESIAN_POINT ( 'NONE',  ( -8.550000000000011369, 2.500000000000000000, 1.718653347947321386 ) ) ;
#30912 = CARTESIAN_POINT ( 'NONE',  ( 14.59999999999989484, 2.500000000000000000, -0.6928203230275541413 ) ) ;
#30913 = EDGE_LOOP ( 'NONE', ( #43756, #37884 ) ) ;
#30914 = CARTESIAN_POINT ( 'NONE',  ( -8.950000000000008171, 2.500000000000000000, 1.818653347947321475 ) ) ;
#30915 = EDGE_CURVE ( 'NONE', #72308, #37406, #13731, .T. ) ;
#30916 = VERTEX_POINT ( 'NONE', #115844 ) ;
#30917 = DIRECTION ( 'NONE',  ( 0.000000000000000000, 1.000000000000000000, 0.000000000000000000 ) ) ;
#30918 = VECTOR ( 'NONE', #125768, 1000.000000000000000 ) ;
#30919 = CONICAL_SURFACE ( 'NONE', #85279, 0.1000000000000000472, 0.003490658503988666988 ) ;
#30920 = VERTEX_POINT ( 'NONE', #5875 ) ;
#30921 = LINE ( 'NONE', #72126, #121710 ) ;
#30922 = FACE_OUTER_BOUND ( 'NONE', #33910, .T. ) ;
#30923 = VERTEX_POINT ( 'NONE', #43267 ) ;
#30924 = ADVANCED_FACE ( 'NONE', ( #63536 ), #45832, .T. ) ;
#30925 = ORIENTED_EDGE ( 'NONE', *, *, #34103, .F. ) ;
#30926 = DIRECTION ( 'NONE',  ( -4.274815082592931898E-19, -0.9999939076577903929, -0.003490651415223739937 ) ) ;
#30927 = CARTESIAN_POINT ( 'NONE',  ( 2.699999999999944666, 12.50000000000000000, 4.676537180435972552 ) ) ;
#30928 = EDGE_LOOP ( 'NONE', ( #10578, #33107, #84946, #9584 ) ) ;
#30929 = VECTOR ( 'NONE', #36311, 1000.000000000000000 ) ;
#30930 = LINE ( 'NONE', #72134, #74015 ) ;
#30931 = CARTESIAN_POINT ( 'NONE',  ( 185.3177083336747160, 4.367472073101515306, 7.564683531250000925 ) ) ;
#30932 = VECTOR ( 'NONE', #52383, 1000.000000000000000 ) ;
#30933 = CONICAL_SURFACE ( 'NONE', #53904, 0.09999999999999982514, 0.003490658503988666988 ) ;
#30934 = CARTESIAN_POINT ( 'NONE',  ( -9.350000000000004974, 2.500000000000000000, 6.148780366869520897 ) ) ;
#30935 = CARTESIAN_POINT ( 'NONE',  ( 106.6782762233207507, 7.234168045436613070, -4.833551603070167069 ) ) ;
#30936 = PLANE ( 'NONE',  #57221 ) ;
#30937 = CARTESIAN_POINT ( 'NONE',  ( -2.900000000000030553, 2.500000000000000000, 4.922947341949748257 ) ) ;
#30938 = CARTESIAN_POINT ( 'NONE',  ( 6.649999999999929301, 2.500000000000000000, 6.595190528383296780 ) ) ;
#30939 = CIRCLE ( 'NONE', #47659, 0.06509327318403743123 ) ;
#30940 = ORIENTED_EDGE ( 'NONE', *, *, #32285, .F. ) ;
#30942 = ORIENTED_EDGE ( 'NONE', *, *, #85848, .T. ) ;
#30941 = EDGE_CURVE ( 'NONE', #91444, #19888, #85095, .T. ) ;
#30943 = FACE_OUTER_BOUND ( 'NONE', #115139, .T. ) ;
#30944 = ORIENTED_EDGE ( 'NONE', *, *, #119268, .F. ) ;
#30945 = CARTESIAN_POINT ( 'NONE',  ( -7.700000000000014388, 2.500000000000000000, -4.676537180435977881 ) ) ;
#30946 = CARTESIAN_POINT ( 'NONE',  ( 9.149999999999916866, 12.50000000000000000, -2.857883832488653741 ) ) ;
#30947 = DIRECTION ( 'NONE',  ( 0.000000000000000000, -0.000000000000000000, 1.000000000000000000 ) ) ;
#30949 = ORIENTED_EDGE ( 'NONE', *, *, #119262, .F. ) ;
#30948 = ORIENTED_EDGE ( 'NONE', *, *, #7981, .F. ) ;
#30950 = FACE_BOUND ( 'NONE', #30380, .T. ) ;
#30951 = VERTEX_POINT ( 'NONE', #4572 ) ;
#30952 = DIRECTION ( 'NONE',  ( -0.000000000000000000, 1.000000000000000000, -0.000000000000000000 ) ) ;
#30953 = DIRECTION ( 'NONE',  ( 0.000000000000000000, 1.000000000000000000, 0.000000000000000000 ) ) ;
#30954 = ADVANCED_FACE ( 'NONE', ( #85735 ), #122424, .T. ) ;
#30956 = ADVANCED_FACE ( 'NONE', ( #53705 ), #49268, .T. ) ;
#30955 = DIRECTION ( 'NONE',  ( 0.000000000000000000, -0.9999939076577903929, 0.003490651415223739937 ) ) ;
#30957 = AXIS2_PLACEMENT_3D ( 'NONE', #119259, #20428, #72114 ) ;
#30958 = DIRECTION ( 'NONE',  ( -4.274815082592931898E-19, -0.9999939076577903929, -0.003490651415223739937 ) ) ;
#30959 = CARTESIAN_POINT ( 'NONE',  ( 10.19999999999991047, 2.500000000000000000, -4.083716857408426826 ) ) ;
#30960 = LINE ( 'NONE', #19840, #63216 ) ;
#30961 = PLANE ( 'NONE',  #33031 ) ;
#30962 = DIRECTION ( 'NONE',  ( 0.000000000000000000, 0.000000000000000000, 1.000000000000000000 ) ) ;
#30963 = EDGE_CURVE ( 'NONE', #95802, #79005, #28327, .T. ) ;
#30964 = EDGE_CURVE ( 'NONE', #114240, #98256, #5243, .T. ) ;
#30965 = DIRECTION ( 'NONE',  ( 0.000000000000000000, 0.000000000000000000, -1.000000000000000000 ) ) ;
#30966 = DIRECTION ( 'NONE',  ( 0.000000000000000000, 0.000000000000000000, -1.000000000000000000 ) ) ;
#30967 = ADVANCED_FACE ( 'NONE', ( #53068 ), #5320, .T. ) ;
#30968 = AXIS2_PLACEMENT_3D ( 'NONE', #87925, #95841, #38219 ) ;
#30969 = EDGE_CURVE ( 'NONE', #5452, #40796, #125024, .T. ) ;
#30970 = CIRCLE ( 'NONE', #106249, 0.1000000000000000472 ) ;
#30971 = DIRECTION ( 'NONE',  ( 0.000000000000000000, 0.000000000000000000, 1.000000000000000000 ) ) ;
#30972 = ORIENTED_EDGE ( 'NONE', *, *, #115253, .F. ) ;
#30974 = ORIENTED_EDGE ( 'NONE', *, *, #84146, .T. ) ;
#30973 = CONICAL_SURFACE ( 'NONE', #99913, 0.1000000000000002554, 0.003490658503988666988 ) ;
#30975 = ORIENTED_EDGE ( 'NONE', *, *, #119183, .T. ) ;
#30976 = EDGE_LOOP ( 'NONE', ( #101935, #40281 ) ) ;
#30977 = LINE ( 'NONE', #90503, #95947 ) ;
#30978 = EDGE_CURVE ( 'NONE', #23241, #17761, #116142, .T. ) ;
#30979 = FACE_OUTER_BOUND ( 'NONE', #85509, .T. ) ;
#30982 = VERTEX_POINT ( 'NONE', #39257 ) ;
#30981 = ORIENTED_EDGE ( 'NONE', *, *, #129498, .T. ) ;
#30980 = EDGE_CURVE ( 'NONE', #86732, #113115, #80653, .T. ) ;
#30984 = VERTEX_POINT ( 'NONE', #7172 ) ;
#30983 = VECTOR ( 'NONE', #93731, 1000.000000000000000 ) ;
#30985 = FACE_OUTER_BOUND ( 'NONE', #25353, .T. ) ;
#30986 = EDGE_CURVE ( 'NONE', #47855, #6356, #97363, .T. ) ;
#30987 = ADVANCED_FACE ( 'NONE', ( #6501 ), #18923, .T. ) ;
#30988 = DIRECTION ( 'NONE',  ( 0.000000000000000000, 0.000000000000000000, 1.000000000000000000 ) ) ;
#30989 =( LENGTH_UNIT ( ) NAMED_UNIT ( * ) SI_UNIT ( .MILLI., .METRE. ) );
#30990 = DIRECTION ( 'NONE',  ( 0.000000000000000000, 0.000000000000000000, 1.000000000000000000 ) ) ;
#30991 = DIRECTION ( 'NONE',  ( -4.274815082592931898E-19, -0.9999939076577903929, -0.003490651415223739937 ) ) ;
#30992 = CARTESIAN_POINT ( 'NONE',  ( 2.500000000000001332, 2.392226903609812716, 9.521986658763283984 ) ) ;
#30993 = CARTESIAN_POINT ( 'NONE',  ( -3.550000000000028244, 2.500000000000000000, 2.511473670974873507 ) ) ;
#30994 = AXIS2_PLACEMENT_3D ( 'NONE', #51850, #77123, #29317 ) ;
#30995 = EDGE_CURVE ( 'NONE', #97440, #70184, #107968, .T. ) ;
#30996 = ORIENTED_EDGE ( 'NONE', *, *, #111837, .T. ) ;
#30997 = EDGE_CURVE ( 'NONE', #43893, #113036, #122228, .T. ) ;
#30998 = ADVANCED_FACE ( 'NONE', ( #16336 ), #15592, .T. ) ;
#30999 = CARTESIAN_POINT ( 'NONE',  ( -7.500000000000011546, 2.500000000000000000, 3.637306695894644726 ) ) ;
#31000 = ORIENTED_EDGE ( 'NONE', *, *, #45383, .F. ) ;
#31002 = VECTOR ( 'NONE', #79351, 1000.000000000000000 ) ;
#31001 = AXIS2_PLACEMENT_3D ( 'NONE', #23407, #113746, #122279 ) ;
#31003 = EDGE_LOOP ( 'NONE', ( #10142, #112066, #25083, #61723 ) ) ;
#31004 = ORIENTED_EDGE ( 'NONE', *, *, #122758, .T. ) ;
#31005 = LINE ( 'NONE', #41463, #81905 ) ;
#31006 = ORIENTED_EDGE ( 'NONE', *, *, #108825, .T. ) ;
#31007 = ORIENTED_EDGE ( 'NONE', *, *, #69193, .F. ) ;
#31008 = EDGE_LOOP ( 'NONE', ( #69600, #31732 ) ) ;
#31009 = CARTESIAN_POINT ( 'NONE',  ( -3.300000000000027800, 2.500000000000000000, -4.330127018922201643 ) ) ;
#31010 = CARTESIAN_POINT ( 'NONE',  ( 4.549999999999937650, 12.50000000000000000, 2.165063509461097713 ) ) ;
#31011 = DIRECTION ( 'NONE',  ( -0.000000000000000000, 1.000000000000000000, -0.000000000000000000 ) ) ;
#31012 = DIRECTION ( 'NONE',  ( 0.000000000000000000, 0.000000000000000000, -1.000000000000000000 ) ) ;
#31013 = DIRECTION ( 'NONE',  ( 0.000000000000000000, 1.000000000000000000, 0.000000000000000000 ) ) ;
#31014 = CARTESIAN_POINT ( 'NONE',  ( 15.19999999999989271, 2.500000000000000000, -0.4464101615137783252 ) ) ;
#31015 = DIRECTION ( 'NONE',  ( 0.000000000000000000, 1.000000000000000000, 0.000000000000000000 ) ) ;
#31016 = VERTEX_POINT ( 'NONE', #26832 ) ;
#31017 = CARTESIAN_POINT ( 'NONE',  ( 18.46077493895528931, 0.2575262203714444031, 4.048716073879469413 ) ) ;
#31018 = VERTEX_POINT ( 'NONE', #77221 ) ;
#31019 = CARTESIAN_POINT ( 'NONE',  ( 108.6701129985725487, 7.143859034846247624, 4.966056649218576702 ) ) ;
#31020 = CARTESIAN_POINT ( 'NONE',  ( 1.649999999999951950, 12.50000000000000000, -7.188010851410854052 ) ) ;
#31021 = CIRCLE ( 'NONE', #83228, 0.1000000000000000472 ) ;
#31022 = CIRCLE ( 'NONE', #47727, 0.1000000000000002554 ) ;
#31023 = VERTEX_POINT ( 'NONE', #46455 ) ;
#31025 = AXIS2_PLACEMENT_3D ( 'NONE', #29984, #109819, #7735 ) ;
#31024 = DIRECTION ( 'NONE',  ( 0.000000000000000000, 1.000000000000000000, 0.000000000000000000 ) ) ;
#31026 = CARTESIAN_POINT ( 'NONE',  ( -12.69999999999999396, 2.500000000000000000, -3.983716857408423628 ) ) ;
#31027 = VERTEX_POINT ( 'NONE', #8454 ) ;
#31028 = AXIS2_PLACEMENT_3D ( 'NONE', #66859, #17087, #57034 ) ;
#31029 = EDGE_CURVE ( 'NONE', #16823, #116336, #122506, .T. ) ;
#31030 = DIRECTION ( 'NONE',  ( -4.274815082592931898E-19, -0.9999939076577903929, -0.003490651415223739937 ) ) ;
#31031 = EDGE_CURVE ( 'NONE', #30530, #94029, #11684, .T. ) ;
#31032 = ORIENTED_EDGE ( 'NONE', *, *, #113563, .F. ) ;
#31033 = ORIENTED_EDGE ( 'NONE', *, *, #67994, .F. ) ;
#31034 = CARTESIAN_POINT ( 'NONE',  ( -13.34999999999999076, 12.50000000000000000, -2.099970236277062252 ) ) ;
#31035 = DIRECTION ( 'NONE',  ( -0.000000000000000000, -1.000000000000000000, -0.000000000000000000 ) ) ;
#31036 = CARTESIAN_POINT ( 'NONE',  ( 185.1302083336747160, -4.367472073101514418, -7.564683531250002702 ) ) ;
#31037 = PLANE ( 'NONE',  #128684 ) ;
#31038 = CIRCLE ( 'NONE', #116676, 0.06509327318403745899 ) ;
#31039 = ADVANCED_FACE ( 'NONE', ( #28121 ), #15881, .T. ) ;
#31040 = DIRECTION ( 'NONE',  ( 0.000000000000000000, 0.000000000000000000, -1.000000000000000000 ) ) ;
#31041 = VECTOR ( 'NONE', #92330, 1000.000000000000000 ) ;
#31042 = ORIENTED_EDGE ( 'NONE', *, *, #92840, .F. ) ;
#31043 = CARTESIAN_POINT ( 'NONE',  ( 1.649999999999950617, 2.500000000000000000, 2.265063509461097357 ) ) ;
#31044 = ORIENTED_EDGE ( 'NONE', *, *, #111008, .F. ) ;
#31045 = CARTESIAN_POINT ( 'NONE',  ( -14.79999999999998472, 2.500000000000000000, 0.3464101615137758494 ) ) ;
#31047 = CONICAL_SURFACE ( 'NONE', #18488, 0.09999999999999982514, 0.003490658503988666988 ) ;
#31046 = DIRECTION ( 'NONE',  ( 0.000000000000000000, 0.000000000000000000, -1.000000000000000000 ) ) ;
#31048 = CIRCLE ( 'NONE', #85401, 0.06509327318403745899 ) ;
#31049 = CARTESIAN_POINT ( 'NONE',  ( 186.1718750003414016, 9.264065473108010111E-16, -7.564683531250000925 ) ) ;
#31050 = DIRECTION ( 'NONE',  ( -4.274815082592931898E-19, -0.9999939076577903929, -0.003490651415223739937 ) ) ;
#31051 = CARTESIAN_POINT ( 'NONE',  ( -5.850000000000021849, 12.50000000000000000, -2.792790559304616504 ) ) ;
#31052 = CARTESIAN_POINT ( 'NONE',  ( 2.299999999999949640, 2.500000000000000000, -0.2464101615137782308 ) ) ;
#31053 = CARTESIAN_POINT ( 'NONE',  ( -4.350000000000023626, 2.500000000000000000, 6.841600689897072485 ) ) ;
#31054 = VERTEX_POINT ( 'NONE', #18289 ) ;
#31055 = AXIS2_PLACEMENT_3D ( 'NONE', #102000, #40521, #62086 ) ;
#31056 = DIRECTION ( 'NONE',  ( 0.000000000000000000, 0.000000000000000000, 1.000000000000000000 ) ) ;
#31057 = FACE_OUTER_BOUND ( 'NONE', #9316, .T. ) ;
#31058 = CARTESIAN_POINT ( 'NONE',  ( 3.749999999999940492, 2.500000000000000000, 2.857883832488649301 ) ) ;
#31059 = ORIENTED_EDGE ( 'NONE', *, *, #14386, .T. ) ;
#31060 = AXIS2_PLACEMENT_3D ( 'NONE', #101168, #81527, #47722 ) ;
#31061 = PLANE ( 'NONE',  #111705 ) ;
#31062 = EDGE_CURVE ( 'NONE', #30982, #23344, #68108, .T. ) ;
#31063 = AXIS2_PLACEMENT_3D ( 'NONE', #33467, #104744, #44563 ) ;
#31064 = ORIENTED_EDGE ( 'NONE', *, *, #102143, .T. ) ;
#31065 = ORIENTED_EDGE ( 'NONE', *, *, #115704, .T. ) ;
#31066 = CARTESIAN_POINT ( 'NONE',  ( -9.200000000000009948, 2.500000000000000000, -4.330127018922197202 ) ) ;
#31067 = ORIENTED_EDGE ( 'NONE', *, *, #12754, .T. ) ;
#31068 = AXIS2_PLACEMENT_3D ( 'NONE', #7250, #95017, #45273 ) ;
#31069 = CARTESIAN_POINT ( 'NONE',  ( 4.399999999999937295, 2.500000000000000000, 3.983716857408420964 ) ) ;
#31070 = CARTESIAN_POINT ( 'NONE',  ( 6.249999999999968914, 2.500000000000000000, -6.495190528383302464 ) ) ;
#31071 = EDGE_LOOP ( 'NONE', ( #105960, #18062, #53511, #125518 ) ) ;
#31072 = CARTESIAN_POINT ( 'NONE',  ( 4.399999999999940847, 2.500000000000000000, -3.983716857408426293 ) ) ;
#31073 = DIRECTION ( 'NONE',  ( -4.274815082592931898E-19, -0.9999939076577903929, -0.003490651415223739937 ) ) ;
#31074 = ADVANCED_FACE ( 'NONE', ( #106668 ), #51425, .T. ) ;
#31075 = CARTESIAN_POINT ( 'NONE',  ( 16.56576425165007294, -1.499999999999999778, -6.084390597445819893 ) ) ;
#31076 = VECTOR ( 'NONE', #4985, 1000.000000000000000 ) ;
#31077 = ORIENTED_EDGE ( 'NONE', *, *, #24178, .F. ) ;
#31079 = CONICAL_SURFACE ( 'NONE', #104218, 0.1000000000000002554, 0.003490658503988666988 ) ;
#31078 = CIRCLE ( 'NONE', #37334, 0.06509327318403745899 ) ;
#31080 = ORIENTED_EDGE ( 'NONE', *, *, #59327, .F. ) ;
#31081 = ORIENTED_EDGE ( 'NONE', *, *, #120757, .T. ) ;
#31082 = DIRECTION ( 'NONE',  ( 0.000000000000000000, -0.000000000000000000, 1.000000000000000000 ) ) ;
#31083 = CARTESIAN_POINT ( 'NONE',  ( 12.89999999999990266, 12.50000000000000000, 3.637306695894644726 ) ) ;
#31084 =( BOUNDED_CURVE ( )  B_SPLINE_CURVE ( 2, ( #68944, #128544, #39518, #78789, #88587, #100984, #9389 ),
 .UNSPECIFIED., .F., .F. ) 
 B_SPLINE_CURVE_WITH_KNOTS ( ( 3, 2, 2, 3 ),
 ( 0.6428571428571433488, 0.6666666666666670737, 0.6904761904761910207, 0.7142857142857148567 ),
 .UNSPECIFIED. ) 
 CURVE ( )  GEOMETRIC_REPRESENTATION_ITEM ( )  RATIONAL_B_SPLINE_CURVE ( ( 0.9999999999999974465, 0.8660254037844412611, 1.000000000000000000, 0.8660254037844387076, 1.000000000000000000, 0.8660254037844355990, 1.000000000000003109 ) ) 
 REPRESENTATION_ITEM ( '' )  );
#31085 = DIRECTION ( 'NONE',  ( 0.000000000000000000, 1.000000000000000000, 0.000000000000000000 ) ) ;
#31086 = ADVANCED_FACE ( 'NONE', ( #27451 ), #84840, .T. ) ;
#31087 = FACE_BOUND ( 'NONE', #96453, .T. ) ;
#31088 = EDGE_LOOP ( 'NONE', ( #47608, #86328, #112867, #32781 ) ) ;
#31089 = DIRECTION ( 'NONE',  ( 0.000000000000000000, 0.000000000000000000, -1.000000000000000000 ) ) ;
#31090 = DIRECTION ( 'NONE',  ( 0.000000000000000000, -0.9999939076577903929, 0.003490651415223739937 ) ) ;
#31091 = ORIENTED_EDGE ( 'NONE', *, *, #26783, .F. ) ;
#31092 = DIRECTION ( 'NONE',  ( 0.000000000000000000, 0.000000000000000000, 1.000000000000000000 ) ) ;
#31093 = CARTESIAN_POINT ( 'NONE',  ( -2.100000000000033840, 12.50000000000000000, 5.022947341949748790 ) ) ;
#31094 = PLANE ( 'NONE',  #23545 ) ;
#31095 = DIRECTION ( 'NONE',  ( 0.000000000000000000, -0.000000000000000000, 1.000000000000000000 ) ) ;
#31096 = AXIS2_PLACEMENT_3D ( 'NONE', #100152, #90300, #10464 ) ;
#31097 = CARTESIAN_POINT ( 'NONE',  ( 10.84999999999991260, 12.50000000000000000, -1.472243186433550122 ) ) ;
#31098 = CARTESIAN_POINT ( 'NONE',  ( -8.150000000000012790, 2.500000000000000000, 2.511473670974873507 ) ) ;
#31099 = CARTESIAN_POINT ( 'NONE',  ( 5.399999999999931966, 12.50000000000000000, 4.330127018922196314 ) ) ;
#31100 = ORIENTED_EDGE ( 'NONE', *, *, #5205, .F. ) ;
#31101 = VERTEX_POINT ( 'NONE', #56908 ) ;
#31102 = AXIS2_PLACEMENT_3D ( 'NONE', #46257, #14210, #65896 ) ;
#31103 = ORIENTED_EDGE ( 'NONE', *, *, #54810, .T. ) ;
#31104 = EDGE_LOOP ( 'NONE', ( #38616, #15951 ) ) ;
#31105 = LINE ( 'NONE', #71016, #47468 ) ;
#31106 = DIRECTION ( 'NONE',  ( 0.000000000000000000, 0.000000000000000000, -1.000000000000000000 ) ) ;
#31107 = VERTEX_POINT ( 'NONE', #88304 ) ;
#31108 = FACE_BOUND ( 'NONE', #86519, .T. ) ;
#31109 = FACE_OUTER_BOUND ( 'NONE', #7661, .T. ) ;
#31111 = EDGE_CURVE ( 'NONE', #21032, #47772, #43115, .T. ) ;
#31110 = DIRECTION ( 'NONE',  ( 0.000000000000000000, 0.000000000000000000, -1.000000000000000000 ) ) ;
#31112 = CONICAL_SURFACE ( 'NONE', #35307, 0.1000000000000000056, 0.003490658503988666988 ) ;
#31113 = CIRCLE ( 'NONE', #110511, 0.1000000000000000472 ) ;
#31114 = DIRECTION ( 'NONE',  ( 0.000000000000000000, -0.9999939076577903929, 0.003490651415223739937 ) ) ;
#31115 = CARTESIAN_POINT ( 'NONE',  ( 10.19999999999991047, 12.50000000000000000, -3.983716857408426293 ) ) ;
#31116 = DIRECTION ( 'NONE',  ( -0.000000000000000000, -1.000000000000000000, -0.000000000000000000 ) ) ;
#31117 = DIRECTION ( 'NONE',  ( 0.000000000000000000, -0.9999939076577903929, 0.003490651415223739937 ) ) ;
#31118 = DIRECTION ( 'NONE',  ( -0.000000000000000000, 1.000000000000000000, -0.000000000000000000 ) ) ;
#31119 = EDGE_CURVE ( 'NONE', #108711, #124173, #105779, .T. ) ;
#31120 = LINE ( 'NONE', #3568, #97763 ) ;
#31121 = ORIENTED_EDGE ( 'NONE', *, *, #98864, .T. ) ;
#31123 = EDGE_CURVE ( 'NONE', #97390, #49498, #49065, .T. ) ;
#31122 = CONICAL_SURFACE ( 'NONE', #79227, 0.1000000000000002554, 0.003490658503988666988 ) ;
#31124 = VERTEX_POINT ( 'NONE', #19588 ) ;
#31125 = ORIENTED_EDGE ( 'NONE', *, *, #114133, .F. ) ;
#31126 = ORIENTED_EDGE ( 'NONE', *, *, #3610, .T. ) ;
#31127 = EDGE_LOOP ( 'NONE', ( #82751, #26042 ) ) ;
#31128 = ORIENTED_EDGE ( 'NONE', *, *, #5622, .F. ) ;
#31129 = ADVANCED_FACE ( 'NONE', ( #70618 ), #88771, .T. ) ;
#31131 = EDGE_CURVE ( 'NONE', #82531, #89806, #32367, .T. ) ;
#31130 = DIRECTION ( 'NONE',  ( 0.000000000000000000, 0.000000000000000000, 1.000000000000000000 ) ) ;
#31133 = VERTEX_POINT ( 'NONE', #51637 ) ;
#31132 = EDGE_CURVE ( 'NONE', #94750, #41903, #39890, .T. ) ;
#31134 = AXIS2_PLACEMENT_3D ( 'NONE', #119628, #50265, #40460 ) ;
#31136 = ADVANCED_FACE ( 'NONE', ( #32000 ), #111841, .T. ) ;
#31135 = CARTESIAN_POINT ( 'NONE',  ( 18.29531403502778986, 0.5011766475904848583, 4.780851392375770281 ) ) ;
#31137 = CARTESIAN_POINT ( 'NONE',  ( 11.04999999999991189, 12.50000000000000000, -2.446380397790840266 ) ) ;
#31138 = CARTESIAN_POINT ( 'NONE',  ( 3.749999999999942268, 2.500000000000000000, 1.372243186433545370 ) ) ;
#31139 = FACE_OUTER_BOUND ( 'NONE', #26359, .T. ) ;
#31140 = EDGE_LOOP ( 'NONE', ( #7211, #2626 ) ) ;
#31141 = DIRECTION ( 'NONE',  ( 0.000000000000000000, 0.000000000000000000, 1.000000000000000000 ) ) ;
#31142 = EDGE_CURVE ( 'NONE', #60850, #92191, #49080, .T. ) ;
#31143 = ORIENTED_EDGE ( 'NONE', *, *, #108672, .T. ) ;
#31144 = ORIENTED_EDGE ( 'NONE', *, *, #110924, .F. ) ;
#31145 = VECTOR ( 'NONE', #128074, 1000.000000000000000 ) ;
#31146 = DIRECTION ( 'NONE',  ( 0.000000000000000000, 0.000000000000000000, 1.000000000000000000 ) ) ;
#31147 = CARTESIAN_POINT ( 'NONE',  ( 3.349999999999944578, 12.50000000000000000, -1.472243186433550122 ) ) ;
#31148 = CARTESIAN_POINT ( 'NONE',  ( 12.69999999999990159, 2.500000000000000000, 4.676537180435972552 ) ) ;
#31149 = EDGE_LOOP ( 'NONE', ( #126369, #68400, #105117, #16830 ) ) ;
#31150 = AXIS2_PLACEMENT_3D ( 'NONE', #46108, #78160, #116772 ) ;
#31151 = ORIENTED_EDGE ( 'NONE', *, *, #89792, .T. ) ;
#31152 = FACE_OUTER_BOUND ( 'NONE', #34972, .T. ) ;
#31153 = AXIS2_PLACEMENT_3D ( 'NONE', #79818, #49736, #120398 ) ;
#31154 = CARTESIAN_POINT ( 'NONE',  ( -11.64999999999999680, 2.500000000000000000, 5.702370205355745014 ) ) ;
#31155 = DIRECTION ( 'NONE',  ( 0.000000000000000000, 1.000000000000000000, 0.000000000000000000 ) ) ;
#31156 = CARTESIAN_POINT ( 'NONE',  ( 9.149999999999915090, 2.500000000000000000, 6.395190528383296602 ) ) ;
#31157 = VERTEX_POINT ( 'NONE', #11692 ) ;
#31158 = DIRECTION ( 'NONE',  ( 0.000000000000000000, 0.000000000000000000, 1.000000000000000000 ) ) ;
#31159 = CIRCLE ( 'NONE', #8137, 0.09999999999999982514 ) ;
#31160 = ORIENTED_EDGE ( 'NONE', *, *, #95593, .F. ) ;
#31161 = CARTESIAN_POINT ( 'NONE',  ( 10.63722763359394463, -2.500000000000000000, 8.014330155125172439 ) ) ;
#31162 = EDGE_LOOP ( 'NONE', ( #17067, #50558, #58249, #1793 ) ) ;
#31163 = DIRECTION ( 'NONE',  ( -0.000000000000000000, 1.000000000000000000, -0.000000000000000000 ) ) ;
#31165 = VECTOR ( 'NONE', #80496, 1000.000000000000000 ) ;
#31164 = CONICAL_SURFACE ( 'NONE', #49944, 0.09999999999999999167, 0.003490658503988666988 ) ;
#31166 = CARTESIAN_POINT ( 'NONE',  ( -9.150000000000009237, 2.500000000000000000, 2.165063509461097713 ) ) ;
#31167 = DIRECTION ( 'NONE',  ( 0.000000000000000000, 1.000000000000000000, 0.000000000000000000 ) ) ;
#31168 = AXIS2_PLACEMENT_3D ( 'NONE', #37695, #47516, #87416 ) ;
#31169 = DIRECTION ( 'NONE',  ( 0.000000000000000000, 0.000000000000000000, -1.000000000000000000 ) ) ;
#31170 = ORIENTED_EDGE ( 'NONE', *, *, #100776, .T. ) ;
#31171 = LINE ( 'NONE', #33108, #2853 ) ;
#31173 = AXIS2_PLACEMENT_3D ( 'NONE', #42984, #102514, #103810 ) ;
#31172 = CIRCLE ( 'NONE', #20694, 0.1000000000000000056 ) ;
#31174 = EDGE_CURVE ( 'NONE', #16787, #57219, #2498, .T. ) ;
#31175 = CARTESIAN_POINT ( 'NONE',  ( 2.049999999999950084, 2.500000000000000000, -2.165063509461101710 ) ) ;
#31176 = ORIENTED_EDGE ( 'NONE', *, *, #103814, .T. ) ;
#31177 = VERTEX_POINT ( 'NONE', #120372 ) ;
#31178 = VERTEX_POINT ( 'NONE', #30065 ) ;
#31179 = DIRECTION ( 'NONE',  ( -0.000000000000000000, 1.000000000000000000, -0.000000000000000000 ) ) ;
#31180 = CARTESIAN_POINT ( 'NONE',  ( -10.85000000000000142, 12.50000000000000000, -5.802370205355746435 ) ) ;
#31181 = CARTESIAN_POINT ( 'NONE',  ( -8.350000000000013856, 2.500000000000000000, -5.802370205355744659 ) ) ;
#31182 = CARTESIAN_POINT ( 'NONE',  ( -2.300000000000032685, 2.500000000000000000, -0.2464101615137783419 ) ) ;
#31183 = FACE_OUTER_BOUND ( 'NONE', #109577, .T. ) ;
#31184 = CARTESIAN_POINT ( 'NONE',  ( 187.5000000000000000, -1.065442715258197248E-15, 8.699999999999999289 ) ) ;
#31185 = EDGE_CURVE ( 'NONE', #62826, #57879, #21885, .T. ) ;
#31186 = CARTESIAN_POINT ( 'NONE',  ( -10.65000000000000391, 12.50000000000000000, -6.148780366869522673 ) ) ;
#31187 = DIRECTION ( 'NONE',  ( -0.000000000000000000, 1.000000000000000000, -0.000000000000000000 ) ) ;
#31188 = CARTESIAN_POINT ( 'NONE',  ( 11.64999999999990443, 2.500000000000000000, -7.188010851410854052 ) ) ;
#31189 = CIRCLE ( 'NONE', #112647, 0.06509327318403745899 ) ;
#31190 = AXIS2_PLACEMENT_3D ( 'NONE', #45198, #55648, #94272 ) ;
#31191 = AXIS2_PLACEMENT_3D ( 'NONE', #117103, #129555, #96827 ) ;
#31192 = ORIENTED_EDGE ( 'NONE', *, *, #77282, .F. ) ;
#31193 = CARTESIAN_POINT ( 'NONE',  ( 3.749999999999942268, 2.500000000000000000, -5.802370205355749988 ) ) ;
#31194 = CARTESIAN_POINT ( 'NONE',  ( 108.0000000000000142, 9.000000000000001776, 0.000000000000000000 ) ) ;
#31195 = CARTESIAN_POINT ( 'NONE',  ( -1.250000000000037526, 2.500000000000000000, -1.372243186433550033 ) ) ;
#31196 = CARTESIAN_POINT ( 'NONE',  ( -10.80000000000000249, 2.500000000000000000, -4.330127018922197202 ) ) ;
#31197 = CONICAL_SURFACE ( 'NONE', #91822, 0.09999999999999982514, 0.003490658503988666988 ) ;
#31198 = ORIENTED_EDGE ( 'NONE', *, *, #116091, .F. ) ;
#31199 = CIRCLE ( 'NONE', #33355, 0.1000000000000002554 ) ;
#31200 = CARTESIAN_POINT ( 'NONE',  ( -12.94999999999999218, 2.500000000000000000, 2.065063509461101621 ) ) ;
#31201 = AXIS2_PLACEMENT_3D ( 'NONE', #106141, #86492, #25001 ) ;
#31202 = DIRECTION ( 'NONE',  ( 0.000000000000000000, 0.000000000000000000, 1.000000000000000000 ) ) ;
#31204 = EDGE_LOOP ( 'NONE', ( #22952, #120389 ) ) ;
#31203 = CARTESIAN_POINT ( 'NONE',  ( 10.39999999999990976, 2.500000000000000000, -4.430127018922202176 ) ) ;
#31205 = AXIS2_PLACEMENT_3D ( 'NONE', #26553, #57304, #48131 ) ;
#31206 = ORIENTED_EDGE ( 'NONE', *, *, #1694, .T. ) ;
#31207 = LINE ( 'NONE', #416, #38477 ) ;
#31209 = ADVANCED_FACE ( 'NONE', ( #111161 ), #22185, .T. ) ;
#31208 = AXIS2_PLACEMENT_3D ( 'NONE', #100079, #57586, #19581 ) ;
#31210 = ORIENTED_EDGE ( 'NONE', *, *, #73494, .T. ) ;
#31211 = ORIENTED_EDGE ( 'NONE', *, *, #113168, .F. ) ;
#31212 = CARTESIAN_POINT ( 'NONE',  ( -12.29999999999999538, 2.500000000000000000, -4.576537180435975571 ) ) ;
#31213 = CARTESIAN_POINT ( 'NONE',  ( 2.299999999999947864, 2.500000000000000000, 3.983716857408420964 ) ) ;
#31214 = DIRECTION ( 'NONE',  ( 0.000000000000000000, 0.000000000000000000, 1.000000000000000000 ) ) ;
#31215 = CARTESIAN_POINT ( 'NONE',  ( -2.950000000000029932, 2.500000000000000000, 2.265063509461097357 ) ) ;
#31216 = ADVANCED_FACE ( 'NONE', ( #90901 ), #17948, .T. ) ;
#31217 = ORIENTED_EDGE ( 'NONE', *, *, #7831, .T. ) ;
#31218 = CARTESIAN_POINT ( 'NONE',  ( 1.899999999999951283, 12.50000000000000000, 0.4115034346978110880 ) ) ;
#31219 = ORIENTED_EDGE ( 'NONE', *, *, #73652, .F. ) ;
#31220 = CIRCLE ( 'NONE', #29168, 0.06509327318403745899 ) ;
#31221 = EDGE_CURVE ( 'NONE', #39963, #13385, #21522, .T. ) ;
#31222 = CARTESIAN_POINT ( 'NONE',  ( 12.69999999999990159, 12.50000000000000000, 4.676537180435972552 ) ) ;
#31223 = CARTESIAN_POINT ( 'NONE',  ( 186.4062500006828031, -8.891194145520236347, -1.633285867636356299E-15 ) ) ;
#31224 = ADVANCED_FACE ( 'NONE', ( #81716 ), #109910, .T. ) ;
#31225 = ORIENTED_EDGE ( 'NONE', *, *, #65682, .F. ) ;
#31226 = VERTEX_POINT ( 'NONE', #80450 ) ;
#31227 = EDGE_CURVE ( 'NONE', #48633, #3662, #82527, .T. ) ;
#31228 = ORIENTED_EDGE ( 'NONE', *, *, #20768, .T. ) ;
#31229 = ORIENTED_EDGE ( 'NONE', *, *, #120359, .F. ) ;
#31230 = DIRECTION ( 'NONE',  ( 0.000000000000000000, 0.000000000000000000, -1.000000000000000000 ) ) ;
#31231 = CARTESIAN_POINT ( 'NONE',  ( 14.18215599412867967, 2.500000000000000000, 6.639800459772074781 ) ) ;
#31232 = CARTESIAN_POINT ( 'NONE',  ( -9.600000000000008527, 12.50000000000000000, -3.637306695894645614 ) ) ;
#31233 = EDGE_CURVE ( 'NONE', #16047, #21053, #45156, .T. ) ;
#31234 = FACE_BOUND ( 'NONE', #8899, .T. ) ;
#31235 = DIRECTION ( 'NONE',  ( -0.000000000000000000, 1.000000000000000000, -0.000000000000000000 ) ) ;
#31236 = CARTESIAN_POINT ( 'NONE',  ( 183.8645833340161175, -6.668395609140180369, 3.849999999999994760 ) ) ;
#31237 = AXIS2_PLACEMENT_3D ( 'NONE', #72843, #63676, #83931 ) ;
#31238 = CARTESIAN_POINT ( 'NONE',  ( 12.89999999999990266, 2.500000000000000000, -5.022947341949754119 ) ) ;
#31239 = DIRECTION ( 'NONE',  ( 0.000000000000000000, 0.000000000000000000, 1.000000000000000000 ) ) ;
#31240 = DIRECTION ( 'NONE',  ( 0.000000000000000000, 1.000000000000000000, 0.000000000000000000 ) ) ;
#31241 = FACE_OUTER_BOUND ( 'NONE', #100622, .T. ) ;
#31242 = VECTOR ( 'NONE', #8089, 1000.000000000000000 ) ;
#31243 = DIRECTION ( 'NONE',  ( 0.000000000000000000, 0.000000000000000000, 1.000000000000000000 ) ) ;
#31244 = CARTESIAN_POINT ( 'NONE',  ( 13.34999999999989662, 12.50000000000000000, -2.792790559304616504 ) ) ;
#31246 = AXIS2_PLACEMENT_3D ( 'NONE', #88178, #66625, #105923 ) ;
#31245 = CIRCLE ( 'NONE', #93933, 0.06509327318403745899 ) ;
#31247 = ORIENTED_EDGE ( 'NONE', *, *, #12805, .T. ) ;
#31248 = ORIENTED_EDGE ( 'NONE', *, *, #60668, .T. ) ;
#31249 = ORIENTED_EDGE ( 'NONE', *, *, #97287, .F. ) ;
#31250 = ORIENTED_EDGE ( 'NONE', *, *, #69688, .T. ) ;
#31251 = VERTEX_POINT ( 'NONE', #89616 ) ;
#31252 = DIRECTION ( 'NONE',  ( 0.000000000000000000, -0.9999939076577903929, 0.003490651415223739937 ) ) ;
#31253 = AXIS2_PLACEMENT_3D ( 'NONE', #103705, #84040, #123968 ) ;
#31254 = CARTESIAN_POINT ( 'NONE',  ( 4.349999999999941025, 12.50000000000000000, -1.883746621131363597 ) ) ;
#31255 = ORIENTED_EDGE ( 'NONE', *, *, #103635, .T. ) ;
#31256 = FACE_BOUND ( 'NONE', #120777, .T. ) ;
#31257 = DIRECTION ( 'NONE',  ( -4.274815082592931898E-19, -0.9999939076577903929, -0.003490651415223739937 ) ) ;
#31259 = AXIS2_PLACEMENT_3D ( 'NONE', #108309, #22372, #42661 ) ;
#31258 = VECTOR ( 'NONE', #120831, 1000.000000000000000 ) ;
#31260 = EDGE_CURVE ( 'NONE', #94355, #79874, #59545, .T. ) ;
#31261 = ORIENTED_EDGE ( 'NONE', *, *, #74403, .F. ) ;
#31262 = DIRECTION ( 'NONE',  ( -0.000000000000000000, -1.000000000000000000, -0.000000000000000000 ) ) ;
#31263 = DIRECTION ( 'NONE',  ( -0.000000000000000000, 1.000000000000000000, -0.000000000000000000 ) ) ;
#31264 = CARTESIAN_POINT ( 'NONE',  ( -8.950000000000009948, 12.50000000000000000, 2.511473670974873507 ) ) ;
#31265 = DIRECTION ( 'NONE',  ( 0.000000000000000000, 1.000000000000000000, 0.000000000000000000 ) ) ;
#31266 = ORIENTED_EDGE ( 'NONE', *, *, #39790, .T. ) ;
#31267 = LINE ( 'NONE', #62658, #109837 ) ;
#31268 = EDGE_CURVE ( 'NONE', #109722, #69263, #129572, .T. ) ;
#31269 = ORIENTED_EDGE ( 'NONE', *, *, #31896, .F. ) ;
#31270 = EDGE_LOOP ( 'NONE', ( #107533, #16762 ) ) ;
#31271 = AXIS2_PLACEMENT_3D ( 'NONE', #108513, #33670, #19486 ) ;
#31272 = EDGE_CURVE ( 'NONE', #72904, #70366, #115957, .T. ) ;
#31273 = PLANE ( 'NONE',  #25675 ) ;
#31274 = CARTESIAN_POINT ( 'NONE',  ( 0.3999999999999563904, 12.50000000000000000, 5.022947341949748790 ) ) ;
#31276 = ORIENTED_EDGE ( 'NONE', *, *, #117567, .F. ) ;
#31275 = ADVANCED_FACE ( 'NONE', ( #60801 ), #34701, .T. ) ;
#31277 = DIRECTION ( 'NONE',  ( -0.000000000000000000, -1.000000000000000000, -0.000000000000000000 ) ) ;
#31278 = ADVANCED_FACE ( 'NONE', ( #64660 ), #33915, .T. ) ;
#31279 = CIRCLE ( 'NONE', #41661, 0.1000000000000002554 ) ;
#31280 = DIRECTION ( 'NONE',  ( 0.000000000000000000, 1.000000000000000000, 0.000000000000000000 ) ) ;
#31281 = CARTESIAN_POINT ( 'NONE',  ( 11.24999999999990585, 12.50000000000000000, 2.922977105672686982 ) ) ;
#31283 = ADVANCED_FACE ( 'NONE', ( #12961 ), #22179, .T. ) ;
#31282 = FACE_OUTER_BOUND ( 'NONE', #112034, .T. ) ;
#31284 = CARTESIAN_POINT ( 'NONE',  ( 7.099999999999928590, 2.500000000000000000, 3.737306695894644371 ) ) ;
#31285 = ORIENTED_EDGE ( 'NONE', *, *, #111498, .F. ) ;
#31287 = ORIENTED_EDGE ( 'NONE', *, *, #110865, .T. ) ;
#31286 = CONICAL_SURFACE ( 'NONE', #25011, 0.1000000000000000472, 0.003490658503988666988 ) ;
#31288 = CARTESIAN_POINT ( 'NONE',  ( 3.749999999999938716, 12.50000000000000000, 7.188010851410848723 ) ) ;
#31291 = EDGE_CURVE ( 'NONE', #9874, #7088, #78606, .T. ) ;
#31290 = AXIS2_PLACEMENT_3D ( 'NONE', #47885, #106776, #64920 ) ;
#31289 = AXIS2_PLACEMENT_3D ( 'NONE', #105839, #26638, #88782 ) ;
#31292 = CONICAL_SURFACE ( 'NONE', #41759, 0.09999999999999982514, 0.003490658503988666988 ) ;
#31293 = EDGE_CURVE ( 'NONE', #71602, #10983, #112040, .T. ) ;
#31294 = ORIENTED_EDGE ( 'NONE', *, *, #67463, .T. ) ;
#31295 = DIRECTION ( 'NONE',  ( 0.000000000000000000, 0.000000000000000000, -1.000000000000000000 ) ) ;
#31296 = ORIENTED_EDGE ( 'NONE', *, *, #78722, .F. ) ;
#31297 = CARTESIAN_POINT ( 'NONE',  ( 8.949999999999921130, 12.50000000000000000, -6.841600689897078702 ) ) ;
#31298 = DIRECTION ( 'NONE',  ( -0.000000000000000000, 1.000000000000000000, -0.000000000000000000 ) ) ;
#31299 = DIRECTION ( 'NONE',  ( -0.000000000000000000, 1.000000000000000000, -0.000000000000000000 ) ) ;
#31300 = CARTESIAN_POINT ( 'NONE',  ( 7.299999999999927880, 12.50000000000000000, 3.983716857408420964 ) ) ;
#31301 = CARTESIAN_POINT ( 'NONE',  ( -2.900000000000029221, 2.500000000000000000, -0.6928203230275541413 ) ) ;
#31302 = AXIS2_PLACEMENT_3D ( 'NONE', #116058, #108804, #95779 ) ;
#31303 = VERTEX_POINT ( 'NONE', #34583 ) ;
#31304 = ORIENTED_EDGE ( 'NONE', *, *, #89150, .T. ) ;
#31306 = EDGE_LOOP ( 'NONE', ( #123909, #26273, #58901, #67012 ) ) ;
#31305 = VECTOR ( 'NONE', #107652, 1000.000000000000000 ) ;
#31307 = DIRECTION ( 'NONE',  ( -4.274815082592931898E-19, -0.9999939076577903929, -0.003490651415223739937 ) ) ;
#31308 = AXIS2_PLACEMENT_3D ( 'NONE', #35565, #56466, #4779 ) ;
#31309 = CARTESIAN_POINT ( 'NONE',  ( -8.350000000000012079, 12.50000000000000000, 2.857883832488649301 ) ) ;
#31310 = DIRECTION ( 'NONE',  ( -0.000000000000000000, 1.000000000000000000, -0.000000000000000000 ) ) ;
#31312 = ORIENTED_EDGE ( 'NONE', *, *, #70349, .T. ) ;
#31311 = EDGE_LOOP ( 'NONE', ( #56189, #42871, #62316, #4818 ) ) ;
#31313 = EDGE_LOOP ( 'NONE', ( #71876, #98117, #36453, #108310 ) ) ;
#31314 = FACE_OUTER_BOUND ( 'NONE', #52595, .T. ) ;
#31315 = ORIENTED_EDGE ( 'NONE', *, *, #34949, .F. ) ;
#31316 = DIRECTION ( 'NONE',  ( -0.000000000000000000, 1.000000000000000000, -0.000000000000000000 ) ) ;
#31317 = DIRECTION ( 'NONE',  ( 0.000000000000000000, -0.9999939076577903929, 0.003490651415223739937 ) ) ;
#31318 = CARTESIAN_POINT ( 'NONE',  ( -1.450000000000035927, 12.50000000000000000, -6.148780366869526226 ) ) ;
#31319 = DIRECTION ( 'NONE',  ( 0.000000000000000000, 0.000000000000000000, 1.000000000000000000 ) ) ;
#31320 = DIRECTION ( 'NONE',  ( -1.000000000000000000, -0.000000000000000000, 1.445602896647339656E-16 ) ) ;
#31321 = LINE ( 'NONE', #19544, #73416 ) ;
#31322 = AXIS2_PLACEMENT_3D ( 'NONE', #90512, #108224, #59142 ) ;
#31323 = CARTESIAN_POINT ( 'NONE',  ( 10.44999999999991402, 12.50000000000000000, 6.495190528383297135 ) ) ;
#31324 = DIRECTION ( 'NONE',  ( 0.000000000000000000, -0.000000000000000000, 1.000000000000000000 ) ) ;
#31325 = EDGE_LOOP ( 'NONE', ( #59669, #22631, #97937, #108847 ) ) ;
#31326 = DIRECTION ( 'NONE',  ( 0.000000000000000000, 1.000000000000000000, 0.000000000000000000 ) ) ;
#31327 = DIRECTION ( 'NONE',  ( 0.000000000000000000, 0.000000000000000000, 1.000000000000000000 ) ) ;
#31328 = ORIENTED_EDGE ( 'NONE', *, *, #56724, .T. ) ;
#31329 = ORIENTED_EDGE ( 'NONE', *, *, #81856, .F. ) ;
#31330 = APPLICATION_CONTEXT ( 'automotive_design' ) ;
#31331 = CARTESIAN_POINT ( 'NONE',  ( 186.5468750003414300, -8.734944146203032389, -1.604583208406768146E-15 ) ) ;
#31332 = LINE ( 'NONE', #62721, #126338 ) ;
#31333 = DIRECTION ( 'NONE',  ( 0.000000000000000000, -0.9999939076577903929, 0.003490651415223739937 ) ) ;
#31334 = CARTESIAN_POINT ( 'NONE',  ( -11.05000000000000071, 2.500000000000000000, 6.841600689897072485 ) ) ;
#31335 = CARTESIAN_POINT ( 'NONE',  ( 13.14999999999990088, 12.50000000000000000, 1.753560074763284016 ) ) ;
#31336 = EDGE_CURVE ( 'NONE', #47870, #126052, #126430, .T. ) ;
#31337 = DIRECTION ( 'NONE',  ( 0.000000000000000000, 0.000000000000000000, -1.000000000000000000 ) ) ;
#31338 = DIRECTION ( 'NONE',  ( 0.000000000000000000, 0.000000000000000000, 1.000000000000000000 ) ) ;
#31339 = DIRECTION ( 'NONE',  ( -4.274815082592931898E-19, -0.9999939076577903929, -0.003490651415223739937 ) ) ;
#31340 = CIRCLE ( 'NONE', #71115, 0.06509327318403741736 ) ;
#31341 = CARTESIAN_POINT ( 'NONE',  ( 12.89999999999990088, 12.50000000000000000, 4.395220292106234439 ) ) ;
#31342 = VERTEX_POINT ( 'NONE', #65290 ) ;
#31343 = ORIENTED_EDGE ( 'NONE', *, *, #86361, .F. ) ;
#31344 = VECTOR ( 'NONE', #36357, 1000.000000000000000 ) ;
#31345 = ORIENTED_EDGE ( 'NONE', *, *, #9637, .T. ) ;
#31346 = CIRCLE ( 'NONE', #39482, 0.1000000000000002554 ) ;
#31347 = EDGE_LOOP ( 'NONE', ( #4518, #30794, #107578, #46100 ) ) ;
#31348 = ORIENTED_EDGE ( 'NONE', *, *, #94664, .F. ) ;
#31349 = CARTESIAN_POINT ( 'NONE',  ( -10.40000000000000213, 2.500000000000000000, 3.537306695894645081 ) ) ;
#31350 = DIRECTION ( 'NONE',  ( 0.000000000000000000, 0.000000000000000000, 1.000000000000000000 ) ) ;
#31353 = ORIENTED_EDGE ( 'NONE', *, *, #10766, .T. ) ;
#31352 = AXIS2_PLACEMENT_3D ( 'NONE', #57621, #37344, #79203 ) ;
#31351 = CIRCLE ( 'NONE', #58543, 0.1000000000000002554 ) ;
#31354 = CARTESIAN_POINT ( 'NONE',  ( 11.04999999999991189, 2.500000000000000000, -2.611473670974877592 ) ) ;
#31355 = CARTESIAN_POINT ( 'NONE',  ( 9.199999999999915801, 2.500000000000000000, -4.330127018922201643 ) ) ;
#31356 = DIRECTION ( 'NONE',  ( 0.000000000000000000, 0.000000000000000000, -1.000000000000000000 ) ) ;
#31358 = ORIENTED_EDGE ( 'NONE', *, *, #5389, .T. ) ;
#31357 = DIRECTION ( 'NONE',  ( 0.000000000000000000, 0.000000000000000000, 1.000000000000000000 ) ) ;
#31359 = DIRECTION ( 'NONE',  ( 0.000000000000000000, 0.000000000000000000, -1.000000000000000000 ) ) ;
#31360 = DIRECTION ( 'NONE',  ( 0.000000000000000000, 0.000000000000000000, 1.000000000000000000 ) ) ;
#31361 = VERTEX_POINT ( 'NONE', #123567 ) ;
#31362 = ORIENTED_EDGE ( 'NONE', *, *, #46216, .T. ) ;
#31363 = ORIENTED_EDGE ( 'NONE', *, *, #65789, .F. ) ;
#31364 = VERTEX_POINT ( 'NONE', #94765 ) ;
#31365 = DIRECTION ( 'NONE',  ( 0.000000000000000000, -0.000000000000000000, 1.000000000000000000 ) ) ;
#31366 = CARTESIAN_POINT ( 'NONE',  ( 5.399999999999934630, 2.500000000000000000, -0.7928203230275543412 ) ) ;
#31367 = DIRECTION ( 'NONE',  ( -0.000000000000000000, 1.000000000000000000, -0.000000000000000000 ) ) ;
#31368 = AXIS2_PLACEMENT_3D ( 'NONE', #123912, #119191, #1338 ) ;
#31369 = ADVANCED_FACE ( 'NONE', ( #73840 ), #74486, .T. ) ;
#31370 = EDGE_LOOP ( 'NONE', ( #31065, #40153 ) ) ;
#31371 = LINE ( 'NONE', #112504, #56477 ) ;
#31372 = VERTEX_POINT ( 'NONE', #113773 ) ;
#31373 = LINE ( 'NONE', #58893, #28683 ) ;
#31374 = CARTESIAN_POINT ( 'NONE',  ( 17.91370874550471370, -0.4812889678260146020, -4.985910759330065112 ) ) ;
#31375 = ADVANCED_FACE ( 'NONE', ( #105229 ), #64021, .T. ) ;
#31376 = DIRECTION ( 'NONE',  ( 0.000000000000000000, 1.000000000000000000, 0.000000000000000000 ) ) ;
#31377 = CARTESIAN_POINT ( 'NONE',  ( 6.449999999999930012, 2.500000000000000000, -1.818653347947326138 ) ) ;
#31378 = ADVANCED_FACE ( 'NONE', ( #24743 ), #61684, .T. ) ;
#31379 = AXIS2_PLACEMENT_3D ( 'NONE', #104600, #5106, #124894 ) ;
#31380 = ORIENTED_EDGE ( 'NONE', *, *, #170, .F. ) ;
#31381 = VERTEX_POINT ( 'NONE', #14262 ) ;
#31382 = EDGE_CURVE ( 'NONE', #7675, #60793, #86711, .T. ) ;
#31384 = EDGE_LOOP ( 'NONE', ( #100715, #123638 ) ) ;
#31383 = EDGE_CURVE ( 'NONE', #111448, #24152, #15544, .T. ) ;
#31385 = DIRECTION ( 'NONE',  ( 0.000000000000000000, -0.9999939076577903929, 0.003490651415223739937 ) ) ;
#31386 = ADVANCED_FACE ( 'NONE', ( #4420 ), #105590, .T. ) ;
#31387 = DIRECTION ( 'NONE',  ( 0.000000000000000000, 0.000000000000000000, 1.000000000000000000 ) ) ;
#31388 = ADVANCED_FACE ( 'NONE', ( #102647 ), #80471, .T. ) ;
#31389 = FACE_BOUND ( 'NONE', #105783, .T. ) ;
#31390 = AXIS2_PLACEMENT_3D ( 'NONE', #69213, #125706, #68575 ) ;
#31391 = FACE_OUTER_BOUND ( 'NONE', #49198, .T. ) ;
#31392 = DIRECTION ( 'NONE',  ( 0.000000000000000000, 1.000000000000000000, 0.000000000000000000 ) ) ;
#31393 = CARTESIAN_POINT ( 'NONE',  ( -12.09999999999999609, 2.500000000000000000, -4.922947341949750921 ) ) ;
#31394 = AXIS2_PLACEMENT_3D ( 'NONE', #2188, #72877, #46635 ) ;
#31395 = AXIS2_PLACEMENT_3D ( 'NONE', #113961, #24290, #124428 ) ;
#31396 = CARTESIAN_POINT ( 'NONE',  ( 10.39999999999991154, 12.50000000000000000, 5.022947341949748790 ) ) ;
#31397 = FACE_OUTER_BOUND ( 'NONE', #28210, .T. ) ;
#31398 = PLANE ( 'NONE',  #46959 ) ;
#31399 = ORIENTED_EDGE ( 'NONE', *, *, #30374, .F. ) ;
#31400 = CIRCLE ( 'NONE', #114899, 0.09999999999999982514 ) ;
#31401 = LINE ( 'NONE', #30765, #76222 ) ;
#31402 = DIRECTION ( 'NONE',  ( -0.000000000000000000, -1.000000000000000000, -0.000000000000000000 ) ) ;
#31403 = AXIS2_PLACEMENT_3D ( 'NONE', #39936, #111891, #89669 ) ;
#31404 = ORIENTED_EDGE ( 'NONE', *, *, #26052, .F. ) ;
#31405 = VERTEX_POINT ( 'NONE', #3175 ) ;
#31406 = PLANE ( 'NONE',  #117131 ) ;
#31407 = CARTESIAN_POINT ( 'NONE',  ( -6.050000000000022027, 2.500000000000000000, -6.048780366869526581 ) ) ;
#31408 = FACE_BOUND ( 'NONE', #24483, .T. ) ;
#31409 = DIRECTION ( 'NONE',  ( 0.000000000000000000, 1.000000000000000000, 0.000000000000000000 ) ) ;
#31410 = ORIENTED_EDGE ( 'NONE', *, *, #28841, .F. ) ;
#31412 = EDGE_CURVE ( 'NONE', #48527, #55655, #43122, .T. ) ;
#31411 = DIRECTION ( 'NONE',  ( 0.000000000000000000, 1.000000000000000000, 0.000000000000000000 ) ) ;
#31413 = CARTESIAN_POINT ( 'NONE',  ( 184.2916666666666572, 4.445597072760120838, -7.699999999999998401 ) ) ;
#31414 = ORIENTED_EDGE ( 'NONE', *, *, #234, .F. ) ;
#31415 = CARTESIAN_POINT ( 'NONE',  ( -4.350000000000023626, 2.500000000000000000, -2.511473670974877948 ) ) ;
#31416 = CARTESIAN_POINT ( 'NONE',  ( 13.54999999999989768, 2.500000000000000000, -2.411473670974877859 ) ) ;
#31418 = EDGE_CURVE ( 'NONE', #105096, #106661, #24022, .T. ) ;
#31417 = AXIS2_PLACEMENT_3D ( 'NONE', #114834, #66390, #33711 ) ;
#31419 = EDGE_CURVE ( 'NONE', #30923, #115271, #72141, .T. ) ;
#31420 = CARTESIAN_POINT ( 'NONE',  ( -11.64999999999999680, 12.50000000000000000, -2.857883832488649745 ) ) ;
#31421 = CARTESIAN_POINT ( 'NONE',  ( -11.84999999999999787, 12.50000000000000000, -6.148780366869522673 ) ) ;
#31422 = EDGE_CURVE ( 'NONE', #106999, #30477, #21983, .T. ) ;
#31423 = EDGE_LOOP ( 'NONE', ( #106706, #110305, #88755, #95240 ) ) ;
#31424 = CARTESIAN_POINT ( 'NONE',  ( 2.899999999999946620, 12.50000000000000000, -3.637306695894650055 ) ) ;
#31425 = AXIS2_PLACEMENT_3D ( 'NONE', #60506, #39589, #90580 ) ;
#31426 = DIRECTION ( 'NONE',  ( 0.000000000000000000, 0.000000000000000000, 1.000000000000000000 ) ) ;
#31427 = CARTESIAN_POINT ( 'NONE',  ( -12.09999999999999609, 2.500000000000000000, 4.230127018922196669 ) ) ;
#31428 = EDGE_CURVE ( 'NONE', #93141, #22544, #69996, .T. ) ;
#31429 = VERTEX_POINT ( 'NONE', #35852 ) ;
#31430 = ORIENTED_EDGE ( 'NONE', *, *, #16427, .T. ) ;
#31431 = EDGE_CURVE ( 'NONE', #356, #22999, #11497, .T. ) ;
#31432 = DIRECTION ( 'NONE',  ( 0.000000000000000000, 0.000000000000000000, -1.000000000000000000 ) ) ;
#31434 = ORIENTED_EDGE ( 'NONE', *, *, #77105, .F. ) ;
#31433 = EDGE_CURVE ( 'NONE', #91784, #68041, #1030, .T. ) ;
#31435 = DIRECTION ( 'NONE',  ( 0.000000000000000000, 0.000000000000000000, 1.000000000000000000 ) ) ;
#31436 = DIRECTION ( 'NONE',  ( -4.274815082592931898E-19, -0.9999939076577903929, -0.003490651415223739937 ) ) ;
#31437 = EDGE_CURVE ( 'NONE', #119726, #85603, #106516, .T. ) ;
#31438 = ADVANCED_FACE ( 'NONE', ( #97983 ), #47015, .T. ) ;
#31439 = DIRECTION ( 'NONE',  ( -0.000000000000000000, -1.000000000000000000, -0.000000000000000000 ) ) ;
#31440 = ORIENTED_EDGE ( 'NONE', *, *, #2633, .T. ) ;
#31441 = DIRECTION ( 'NONE',  ( -0.000000000000000000, 1.000000000000000000, -0.000000000000000000 ) ) ;
#31442 = DIRECTION ( 'NONE',  ( -0.000000000000000000, -1.000000000000000000, -0.000000000000000000 ) ) ;
#31443 = CARTESIAN_POINT ( 'NONE',  ( 4.399999999999937295, 2.500000000000000000, 4.676537180435972552 ) ) ;
#31444 = CARTESIAN_POINT ( 'NONE',  ( -5.400000000000019895, 2.500000000000000000, -2.276824562219559311E-15 ) ) ;
#31445 = CARTESIAN_POINT ( 'NONE',  ( -4.119968255444916849E-14, 12.50000000000000000, 3.702399969078682407 ) ) ;
#31447 = EDGE_CURVE ( 'NONE', #27262, #106163, #90917, .T. ) ;
#31446 = DIRECTION ( 'NONE',  ( 0.000000000000000000, 1.000000000000000000, 0.000000000000000000 ) ) ;
#31448 = ORIENTED_EDGE ( 'NONE', *, *, #13774, .F. ) ;
#31449 = ORIENTED_EDGE ( 'NONE', *, *, #120038, .T. ) ;
#31450 = CARTESIAN_POINT ( 'NONE',  ( -6.650000000000014566, 2.500000000000000000, 2.265063509461097357 ) ) ;
#31451 = EDGE_LOOP ( 'NONE', ( #100218, #83883, #82812, #60554 ) ) ;
#31452 = FACE_OUTER_BOUND ( 'NONE', #120312, .T. ) ;
#31454 = ORIENTED_EDGE ( 'NONE', *, *, #9953, .T. ) ;
#31453 = ORIENTED_EDGE ( 'NONE', *, *, #16592, .F. ) ;
#31455 = ORIENTED_EDGE ( 'NONE', *, *, #32287, .T. ) ;
#31456 = DIRECTION ( 'NONE',  ( 0.000000000000000000, 0.000000000000000000, 1.000000000000000000 ) ) ;
#31457 = AXIS2_PLACEMENT_3D ( 'NONE', #34032, #124987, #15655 ) ;
#31458 = CARTESIAN_POINT ( 'NONE',  ( 11.64999999999990266, 12.50000000000000000, 2.165063509461097713 ) ) ;
#31459 = CIRCLE ( 'NONE', #64875, 0.06509327318403745899 ) ;
#31460 = DIRECTION ( 'NONE',  ( 0.000000000000000000, 0.000000000000000000, 1.000000000000000000 ) ) ;
#31461 = FACE_OUTER_BOUND ( 'NONE', #91160, .T. ) ;
#31462 = CARTESIAN_POINT ( 'NONE',  ( 2.699999999999947331, 2.500000000000000000, -0.3464101615137783474 ) ) ;
#31463 = CARTESIAN_POINT ( 'NONE',  ( 2.899999999999943956, 2.500000000000000000, 4.330127018922196314 ) ) ;
#31464 = DIRECTION ( 'NONE',  ( -0.000000000000000000, -1.000000000000000000, -0.000000000000000000 ) ) ;
#31465 = CARTESIAN_POINT ( 'NONE',  ( 4.149999999999939959, 2.500000000000000000, 2.957883832488649389 ) ) ;
#31467 = AXIS2_PLACEMENT_3D ( 'NONE', #123593, #113792, #65309 ) ;
#31466 = CARTESIAN_POINT ( 'NONE',  ( 6.899999999999928413, 2.500000000000000000, -4.776537180435977525 ) ) ;
#31468 = VERTEX_POINT ( 'NONE', #45679 ) ;
#31469 = DIRECTION ( 'NONE',  ( -0.000000000000000000, -1.000000000000000000, -0.000000000000000000 ) ) ;
#31470 = ORIENTED_EDGE ( 'NONE', *, *, #96294, .T. ) ;
#31471 = ORIENTED_EDGE ( 'NONE', *, *, #97045, .F. ) ;
#31472 = CARTESIAN_POINT ( 'NONE',  ( 108.0000000000000142, 9.000000000000001776, -0.2500000000000000000 ) ) ;
#31473 = DIRECTION ( 'NONE',  ( 0.000000000000000000, 1.000000000000000000, 0.000000000000000000 ) ) ;
#31474 = CIRCLE ( 'NONE', #94160, 0.06509327318403743123 ) ;
#31475 = CARTESIAN_POINT ( 'NONE',  ( -8.350000000000012079, 2.500000000000000000, 2.857883832488649301 ) ) ;
#31476 = AXIS2_PLACEMENT_3D ( 'NONE', #56150, #74522, #54859 ) ;
#31477 = EDGE_CURVE ( 'NONE', #128465, #102223, #84653, .T. ) ;
#31478 = DIRECTION ( 'NONE',  ( 0.000000000000000000, 0.000000000000000000, -1.000000000000000000 ) ) ;
#31479 = DIRECTION ( 'NONE',  ( -4.274815082592931898E-19, -0.9999939076577903929, -0.003490651415223739937 ) ) ;
#31480 = CARTESIAN_POINT ( 'NONE',  ( -10.84999999999999964, 2.500000000000000000, 5.802370205355744659 ) ) ;
#31481 = VERTEX_POINT ( 'NONE', #57429 ) ;
#31482 = AXIS2_PLACEMENT_3D ( 'NONE', #28151, #68065, #58904 ) ;
#31483 = ORIENTED_EDGE ( 'NONE', *, *, #4062, .T. ) ;
#31484 = VERTEX_POINT ( 'NONE', #27299 ) ;
#31485 = CARTESIAN_POINT ( 'NONE',  ( 9.399999999999915090, 12.50000000000000000, 4.676537180435972552 ) ) ;
#31486 = AXIS2_PLACEMENT_3D ( 'NONE', #26569, #117487, #13008 ) ;
#31487 = VERTEX_POINT ( 'NONE', #108445 ) ;
#31488 = EDGE_CURVE ( 'NONE', #127679, #16283, #118610, .T. ) ;
#31489 = EDGE_LOOP ( 'NONE', ( #25575, #98938 ) ) ;
#31490 = CARTESIAN_POINT ( 'NONE',  ( -8.350000000000013856, 12.50000000000000000, -6.495190528383297135 ) ) ;
#31491 = CARTESIAN_POINT ( 'NONE',  ( -4.999999999999990230, 2.500000000000000000, -4.330127018922201643 ) ) ;
#31492 = DIRECTION ( 'NONE',  ( -0.000000000000000000, 1.000000000000000000, -0.000000000000000000 ) ) ;
#31493 = DIRECTION ( 'NONE',  ( 0.000000000000000000, 0.000000000000000000, 1.000000000000000000 ) ) ;
#31494 = LINE ( 'NONE', #92333, #30498 ) ;
#31495 = ORIENTED_EDGE ( 'NONE', *, *, #91366, .T. ) ;
#31496 = DIRECTION ( 'NONE',  ( 0.000000000000000000, 0.000000000000000000, 1.000000000000000000 ) ) ;
#31497 = DIRECTION ( 'NONE',  ( -0.000000000000000000, 1.000000000000000000, -0.000000000000000000 ) ) ;
#31498 = DIRECTION ( 'NONE',  ( -0.000000000000000000, 1.000000000000000000, -0.000000000000000000 ) ) ;
#31499 = DIRECTION ( 'NONE',  ( -0.000000000000000000, -1.000000000000000000, -0.000000000000000000 ) ) ;
#31500 = DIRECTION ( 'NONE',  ( -0.000000000000000000, 1.000000000000000000, -0.000000000000000000 ) ) ;
#31501 = EDGE_LOOP ( 'NONE', ( #10130, #53097, #114971, #20158 ) ) ;
#31502 = EDGE_LOOP ( 'NONE', ( #127875, #63466 ) ) ;
#31503 = ORIENTED_EDGE ( 'NONE', *, *, #28908, .F. ) ;
#31504 = VECTOR ( 'NONE', #98261, 1000.000000000000000 ) ;
#31505 = CARTESIAN_POINT ( 'NONE',  ( -11.69999999999999929, 12.50000000000000000, -4.330127018922198978 ) ) ;
#31506 = VECTOR ( 'NONE', #95719, 1000.000000000000000 ) ;
#31507 = CIRCLE ( 'NONE', #94194, 7.500000000000000000 ) ;
#31508 = EDGE_LOOP ( 'NONE', ( #53148, #99493, #65596, #3996 ) ) ;
#31509 = CARTESIAN_POINT ( 'NONE',  ( -2.100000000000033840, 2.500000000000000000, 5.122947341949749323 ) ) ;
#31510 = DIRECTION ( 'NONE',  ( 0.000000000000000000, 0.000000000000000000, 1.000000000000000000 ) ) ;
#31511 = ADVANCED_FACE ( 'NONE', ( #97345 ), #7659, .T. ) ;
#31512 = AXIS2_PLACEMENT_3D ( 'NONE', #1402, #41357, #81265 ) ;
#31514 = ORIENTED_EDGE ( 'NONE', *, *, #110352, .F. ) ;
#31513 = AXIS2_PLACEMENT_3D ( 'NONE', #81522, #121429, #102450 ) ;
#31515 = LINE ( 'NONE', #30890, #7641 ) ;
#31516 = DIRECTION ( 'NONE',  ( -0.000000000000000000, 1.000000000000000000, -0.000000000000000000 ) ) ;
#31517 = CARTESIAN_POINT ( 'NONE',  ( 2.699999999999946443, 2.500000000000000000, -3.883716857408426648 ) ) ;
#31518 = LINE ( 'NONE', #101549, #95752 ) ;
#31519 = EDGE_CURVE ( 'NONE', #71951, #97815, #105877, .T. ) ;
#31520 = DIRECTION ( 'NONE',  ( 0.000000000000000000, -0.9999939076577903929, 0.003490651415223739937 ) ) ;
#31521 = ORIENTED_EDGE ( 'NONE', *, *, #2053, .F. ) ;
#31522 = ADVANCED_FACE ( 'NONE', ( #117596 ), #38718, .T. ) ;
#31523 = EDGE_CURVE ( 'NONE', #65236, #125999, #109793, .T. ) ;
#31524 = EDGE_LOOP ( 'NONE', ( #128414, #62809, #2246, #107014 ) ) ;
#31525 = ADVANCED_FACE ( 'NONE', ( #86216 ), #88858, .T. ) ;
#31527 = EDGE_CURVE ( 'NONE', #15198, #122612, #18776, .T. ) ;
#31526 = CARTESIAN_POINT ( 'NONE',  ( 35.03127169446342037, 3.271239217524853249, -3.345729450120381365 ) ) ;
#31528 = ADVANCED_FACE ( 'NONE', ( #36513 ), #76424, .T. ) ;
#31529 = DIRECTION ( 'NONE',  ( -4.274815082592931898E-19, -0.9999939076577903929, -0.003490651415223739937 ) ) ;
#31530 = FACE_OUTER_BOUND ( 'NONE', #21649, .T. ) ;
#31531 = LINE ( 'NONE', #71433, #91885 ) ;
#31532 = VERTEX_POINT ( 'NONE', #48907 ) ;
#31533 = ORIENTED_EDGE ( 'NONE', *, *, #14929, .F. ) ;
#31534 = CARTESIAN_POINT ( 'NONE',  ( -11.84999999999999787, 2.500000000000000000, -2.511473670974873951 ) ) ;
#31535 = DIRECTION ( 'NONE',  ( 0.000000000000000000, 1.000000000000000000, 0.000000000000000000 ) ) ;
#31536 = EDGE_CURVE ( 'NONE', #2251, #113231, #57474, .T. ) ;
#31537 = CARTESIAN_POINT ( 'NONE',  ( -11.44999999999999751, 12.50000000000000000, 6.213873640053559022 ) ) ;
#31538 = DIRECTION ( 'NONE',  ( 0.000000000000000000, -0.000000000000000000, 1.000000000000000000 ) ) ;
#31539 = ORIENTED_EDGE ( 'NONE', *, *, #68407, .T. ) ;
#31540 = EDGE_CURVE ( 'NONE', #86369, #39107, #42920, .T. ) ;
#31541 = CONICAL_SURFACE ( 'NONE', #50323, 0.1000000000000002554, 0.003490658503988666988 ) ;
#31543 = EDGE_CURVE ( 'NONE', #66987, #92109, #44954, .T. ) ;
#31542 = DIRECTION ( 'NONE',  ( 0.000000000000000000, 0.000000000000000000, 1.000000000000000000 ) ) ;
#31544 = AXIS2_PLACEMENT_3D ( 'NONE', #128733, #68484, #8908 ) ;
#31545 = DIRECTION ( 'NONE',  ( 0.000000000000000000, 1.000000000000000000, 0.000000000000000000 ) ) ;
#31546 = VERTEX_POINT ( 'NONE', #91385 ) ;
#31547 = FACE_OUTER_BOUND ( 'NONE', #99871, .T. ) ;
#31548 = ORIENTED_EDGE ( 'NONE', *, *, #39539, .F. ) ;
#31549 = AXIS2_PLACEMENT_3D ( 'NONE', #8329, #48263, #39120 ) ;
#31550 = DIRECTION ( 'NONE',  ( -4.274815082592931898E-19, -0.9999939076577903929, -0.003490651415223739937 ) ) ;
#31551 = AXIS2_PLACEMENT_3D ( 'NONE', #13096, #123077, #54331 ) ;
#31552 = ORIENTED_EDGE ( 'NONE', *, *, #50024, .T. ) ;
#31553 = ORIENTED_EDGE ( 'NONE', *, *, #25295, .T. ) ;
#31554 = DIRECTION ( 'NONE',  ( 0.000000000000000000, 1.000000000000000000, 0.000000000000000000 ) ) ;
#31555 = CARTESIAN_POINT ( 'NONE',  ( 10.61495711629421557, 2.499999999999999112, -8.020491763388227113 ) ) ;
#31556 = VERTEX_POINT ( 'NONE', #22027 ) ;
#31557 = EDGE_LOOP ( 'NONE', ( #22003, #65006, #94542, #58272 ) ) ;
#31558 = DIRECTION ( 'NONE',  ( -4.274815082592931898E-19, -0.9999939076577903929, -0.003490651415223739937 ) ) ;
#31559 = DIRECTION ( 'NONE',  ( 0.000000000000000000, 0.000000000000000000, -1.000000000000000000 ) ) ;
#31560 = VERTEX_POINT ( 'NONE', #31831 ) ;
#31562 = CARTESIAN_POINT ( 'NONE',  ( 186.8385416670080872, 6.551208109652274736, 3.782341765625001351 ) ) ;
#31561 = CIRCLE ( 'NONE', #73313, 0.06509327318403745899 ) ;
#31563 = CARTESIAN_POINT ( 'NONE',  ( 184.2760416670080588, 6.551208109652274736, 3.782341765625001351 ) ) ;
#31564 = CONICAL_SURFACE ( 'NONE', #12757, 0.1000000000000000472, 0.003490658503988666988 ) ;
#31565 = DIRECTION ( 'NONE',  ( 0.000000000000000000, 1.000000000000000000, 0.000000000000000000 ) ) ;
#31566 = CARTESIAN_POINT ( 'NONE',  ( 0.4499999999999573785, 12.50000000000000000, -6.495190528383302464 ) ) ;
#31567 = DIRECTION ( 'NONE',  ( 0.000000000000000000, 0.000000000000000000, -1.000000000000000000 ) ) ;
#31568 = PLANE ( 'NONE',  #59865 ) ;
#31569 = DIRECTION ( 'NONE',  ( -0.000000000000000000, 1.000000000000000000, -0.000000000000000000 ) ) ;
#31570 = AXIS2_PLACEMENT_3D ( 'NONE', #88847, #8345, #70493 ) ;
#31571 = EDGE_LOOP ( 'NONE', ( #63924, #114537 ) ) ;
#31572 = ORIENTED_EDGE ( 'NONE', *, *, #31382, .T. ) ;
#31573 = DIRECTION ( 'NONE',  ( -0.000000000000000000, 1.000000000000000000, -0.000000000000000000 ) ) ;
#31574 = ORIENTED_EDGE ( 'NONE', *, *, #85901, .F. ) ;
#31575 = AXIS2_PLACEMENT_3D ( 'NONE', #3547, #43488, #94489 ) ;
#31576 = CARTESIAN_POINT ( 'NONE',  ( 0.8499999999999527933, 2.500000000000000000, 7.188010851410848723 ) ) ;
#31577 = DIRECTION ( 'NONE',  ( 0.000000000000000000, 1.000000000000000000, 0.000000000000000000 ) ) ;
#31578 = DIRECTION ( 'NONE',  ( -0.000000000000000000, -1.000000000000000000, -0.000000000000000000 ) ) ;
#31580 = ORIENTED_EDGE ( 'NONE', *, *, #58085, .T. ) ;
#31579 = VERTEX_POINT ( 'NONE', #90085 ) ;
#31581 = FACE_BOUND ( 'NONE', #13063, .T. ) ;
#31582 = EDGE_LOOP ( 'NONE', ( #82623, #79529, #90808, #86792 ) ) ;
#31583 = EDGE_CURVE ( 'NONE', #56340, #79920, #50827, .T. ) ;
#31584 = CARTESIAN_POINT ( 'NONE',  ( -2.700000000000031264, 2.500000000000000000, 4.776537180435972196 ) ) ;
#31585 = LINE ( 'NONE', #58481, #106537 ) ;
#31586 = EDGE_CURVE ( 'NONE', #115443, #91335, #120166, .T. ) ;
#31587 = CARTESIAN_POINT ( 'NONE',  ( -9.600000000000008527, 2.500000000000000000, -4.330127018922197202 ) ) ;
#31588 = FACE_OUTER_BOUND ( 'NONE', #1398, .T. ) ;
#31589 = CARTESIAN_POINT ( 'NONE',  ( -4.600000000000028066, 2.500000000000000000, -3.637306695894650055 ) ) ;
#31590 = EDGE_CURVE ( 'NONE', #77313, #25933, #53275, .T. ) ;
#31591 = CARTESIAN_POINT ( 'NONE',  ( 13.09999999999989839, 2.500000000000000000, 0.2464101615137735679 ) ) ;
#31592 = FACE_OUTER_BOUND ( 'NONE', #46084, .T. ) ;
#31593 = DIRECTION ( 'NONE',  ( 0.000000000000000000, 1.000000000000000000, 0.000000000000000000 ) ) ;
#31594 = DIRECTION ( 'NONE',  ( 0.000000000000000000, 0.000000000000000000, 1.000000000000000000 ) ) ;
#31595 = DIRECTION ( 'NONE',  ( -0.000000000000000000, 1.000000000000000000, -0.000000000000000000 ) ) ;
#31597 = ADVANCED_FACE ( 'NONE', ( #110382 ), #99933, .T. ) ;
#31596 = CARTESIAN_POINT ( 'NONE',  ( 88.00000000000001421, 1.065442715258197248E-15, -8.699999999999999289 ) ) ;
#31598 = ORIENTED_EDGE ( 'NONE', *, *, #32466, .T. ) ;
#31599 = ORIENTED_EDGE ( 'NONE', *, *, #124315, .T. ) ;
#31600 = ORIENTED_EDGE ( 'NONE', *, *, #112844, .T. ) ;
#31601 = EDGE_LOOP ( 'NONE', ( #28398, #125844, #61209, #82885 ) ) ;
#31602 = FACE_OUTER_BOUND ( 'NONE', #73464, .T. ) ;
#31603 = AXIS2_PLACEMENT_3D ( 'NONE', #1994, #32133, #123686 ) ;
#31604 = FACE_OUTER_BOUND ( 'NONE', #67351, .T. ) ;
#31605 = AXIS2_PLACEMENT_3D ( 'NONE', #19742, #97643, #129064 ) ;
#31606 = AXIS2_PLACEMENT_3D ( 'NONE', #121944, #22477, #89896 ) ;
#31608 = EDGE_LOOP ( 'NONE', ( #97237, #42198, #119024, #80519 ) ) ;
#31607 = ORIENTED_EDGE ( 'NONE', *, *, #118265, .F. ) ;
#31609 = VERTEX_POINT ( 'NONE', #1712 ) ;
#31610 = CARTESIAN_POINT ( 'NONE',  ( 13.74999999999989519, 12.50000000000000000, -2.857883832488653741 ) ) ;
#31611 = AXIS2_PLACEMENT_3D ( 'NONE', #106051, #56924, #107336 ) ;
#31612 = CARTESIAN_POINT ( 'NONE',  ( -0.4500000000000397571, 2.500000000000000000, -2.065063509461102065 ) ) ;
#31613 = CARTESIAN_POINT ( 'NONE',  ( -7.900000000000011013, 12.50000000000000000, 5.022947341949748790 ) ) ;
#31614 = CARTESIAN_POINT ( 'NONE',  ( 9.599999999999914380, 2.500000000000000000, 5.022947341949748790 ) ) ;
#31615 = DIRECTION ( 'NONE',  ( 0.000000000000000000, 0.000000000000000000, 1.000000000000000000 ) ) ;
#31616 = CARTESIAN_POINT ( 'NONE',  ( 0.8499999999999545697, 2.500000000000000000, 2.957883832488649389 ) ) ;
#31617 = AXIS2_PLACEMENT_3D ( 'NONE', #91830, #110185, #2150 ) ;
#31618 = DIRECTION ( 'NONE',  ( -0.000000000000000000, -1.000000000000000000, -0.000000000000000000 ) ) ;
#31619 = ADVANCED_FACE ( 'NONE', ( #29895 ), #69157, .T. ) ;
#31620 = ORIENTED_EDGE ( 'NONE', *, *, #7096, .T. ) ;
#31621 = FACE_OUTER_BOUND ( 'NONE', #13332, .T. ) ;
#31622 = ORIENTED_EDGE ( 'NONE', *, *, #112362, .F. ) ;
#31623 = ORIENTED_EDGE ( 'NONE', *, *, #29341, .T. ) ;
#31624 = ORIENTED_EDGE ( 'NONE', *, *, #127886, .F. ) ;
#31625 = CARTESIAN_POINT ( 'NONE',  ( 185.2812500006828031, 0.000000000000000000, 7.700000000000000178 ) ) ;
#31626 = EDGE_LOOP ( 'NONE', ( #99723, #43494 ) ) ;
#31627 = VERTEX_POINT ( 'NONE', #128768 ) ;
#31628 = ORIENTED_EDGE ( 'NONE', *, *, #51957, .F. ) ;
#31629 = DIRECTION ( 'NONE',  ( 0.000000000000000000, 1.000000000000000000, 0.000000000000000000 ) ) ;
#31630 = AXIS2_PLACEMENT_3D ( 'NONE', #94861, #13707, #14976 ) ;
#31631 = LINE ( 'NONE', #10667, #18346 ) ;
#31632 = DIRECTION ( 'NONE',  ( 0.000000000000000000, 0.000000000000000000, -1.000000000000000000 ) ) ;
#31633 = ADVANCED_FACE ( 'NONE', ( #111005 ), #50199, .T. ) ;
#31634 = DIRECTION ( 'NONE',  ( 0.000000000000000000, 0.000000000000000000, 1.000000000000000000 ) ) ;
#31635 = DIRECTION ( 'NONE',  ( 0.000000000000000000, -0.9999939076577903929, 0.003490651415223739937 ) ) ;
#31636 = CARTESIAN_POINT ( 'NONE',  ( 3.549999999999942979, 2.500000000000000000, 1.718653347947321386 ) ) ;
#31637 = CARTESIAN_POINT ( 'NONE',  ( 14.79999999999989235, 2.500000000000000000, 0.3464101615137735735 ) ) ;
#31638 = CONICAL_SURFACE ( 'NONE', #48355, 0.1000000000000002554, 0.003490658503988666988 ) ;
#31639 = EDGE_LOOP ( 'NONE', ( #49678, #3274 ) ) ;
#31640 = DIRECTION ( 'NONE',  ( -0.000000000000000000, -1.000000000000000000, -0.000000000000000000 ) ) ;
#31641 = VERTEX_POINT ( 'NONE', #20083 ) ;
#31642 = DIRECTION ( 'NONE',  ( 0.000000000000000000, -0.9999939076577903929, 0.003490651415223739937 ) ) ;
#31643 = EDGE_LOOP ( 'NONE', ( #40645, #122161 ) ) ;
#31644 = DIRECTION ( 'NONE',  ( 0.000000000000000000, -0.9999939076577903929, 0.003490651415223739937 ) ) ;
#31645 = EDGE_CURVE ( 'NONE', #8661, #1776, #113914, .T. ) ;
#31646 = ORIENTED_EDGE ( 'NONE', *, *, #3032, .F. ) ;
#31647 = CARTESIAN_POINT ( 'NONE',  ( 184.5260416670080588, -6.551208109652273848, -3.782341765625003571 ) ) ;
#31648 = CIRCLE ( 'NONE', #54610, 0.06509327318403745899 ) ;
#31649 = DIRECTION ( 'NONE',  ( 0.000000000000000000, 0.000000000000000000, 1.000000000000000000 ) ) ;
#31650 = ORIENTED_EDGE ( 'NONE', *, *, #4306, .F. ) ;
#31651 = EDGE_LOOP ( 'NONE', ( #120345, #109295, #80158, #77559 ) ) ;
#31652 = DIRECTION ( 'NONE',  ( 1.000000000000000000, 0.000000000000000000, 0.000000000000000000 ) ) ;
#31653 = CARTESIAN_POINT ( 'NONE',  ( 8.749999999999920064, 12.50000000000000000, 5.802370205355744659 ) ) ;
#31654 = CARTESIAN_POINT ( 'NONE',  ( 184.2135416670080588, 4.367472073101518859, -7.564683531249999149 ) ) ;
#31655 = DIRECTION ( 'NONE',  ( -4.274815082592931898E-19, -0.9999939076577903929, -0.003490651415223739937 ) ) ;
#31656 = AXIS2_PLACEMENT_3D ( 'NONE', #118283, #37795, #128780 ) ;
#31657 = CIRCLE ( 'NONE', #42122, 0.06509327318403745899 ) ;
#31658 = DIRECTION ( 'NONE',  ( 0.000000000000000000, 1.000000000000000000, 0.000000000000000000 ) ) ;
#31659 = ORIENTED_EDGE ( 'NONE', *, *, #40558, .T. ) ;
#31660 = LINE ( 'NONE', #31043, #123995 ) ;
#31661 = VECTOR ( 'NONE', #43601, 1000.000000000000000 ) ;
#31662 = VECTOR ( 'NONE', #16059, 1000.000000000000000 ) ;
#31663 = ORIENTED_EDGE ( 'NONE', *, *, #68878, .F. ) ;
#31664 = FACE_OUTER_BOUND ( 'NONE', #79595, .T. ) ;
#31665 = CARTESIAN_POINT ( 'NONE',  ( -6.071532165918824830E-15, 2.500000000000000000, -4.230127018922201998 ) ) ;
#31666 = EDGE_CURVE ( 'NONE', #58654, #73675, #9535, .T. ) ;
#31667 = VECTOR ( 'NONE', #85326, 1000.000000000000000 ) ;
#31668 = CIRCLE ( 'NONE', #255, 0.09999999999999982514 ) ;
#31669 = CARTESIAN_POINT ( 'NONE',  ( 187.1718750003414016, 9.264065473108010111E-16, -7.564683531250000925 ) ) ;
#31670 = DIRECTION ( 'NONE',  ( 0.000000000000000000, 0.000000000000000000, -1.000000000000000000 ) ) ;
#31671 = DIRECTION ( 'NONE',  ( 0.000000000000000000, 0.000000000000000000, 1.000000000000000000 ) ) ;
#31672 = DIRECTION ( 'NONE',  ( -0.000000000000000000, -1.000000000000000000, -0.000000000000000000 ) ) ;
#31673 = DIRECTION ( 'NONE',  ( 0.000000000000000000, 0.000000000000000000, -1.000000000000000000 ) ) ;
#31674 = EDGE_LOOP ( 'NONE', ( #58470, #28915, #92467, #30273 ) ) ;
#31675 = EDGE_CURVE ( 'NONE', #17546, #69331, #111944, .T. ) ;
#31676 = CARTESIAN_POINT ( 'NONE',  ( 11.24999999999990585, 2.500000000000000000, -5.802370205355749988 ) ) ;
#31677 = CARTESIAN_POINT ( 'NONE',  ( 105.5000000000000142, -1.500000000000000222, -1.322875655532295136 ) ) ;
#31678 = CARTESIAN_POINT ( 'NONE',  ( -3.150000000000029221, 12.50000000000000000, 2.576566944158910744 ) ) ;
#31679 = ADVANCED_FACE ( 'NONE', ( #40374 ), #99435, .T. ) ;
#31680 = EDGE_CURVE ( 'NONE', #43214, #115043, #55505, .T. ) ;
#31681 = EDGE_CURVE ( 'NONE', #22692, #101260, #63826, .T. ) ;
#31682 = EDGE_CURVE ( 'NONE', #20502, #27204, #39743, .T. ) ;
#31683 = ORIENTED_EDGE ( 'NONE', *, *, #15699, .F. ) ;
#31684 = DIRECTION ( 'NONE',  ( -0.000000000000000000, 1.000000000000000000, -0.000000000000000000 ) ) ;
#31685 = ORIENTED_EDGE ( 'NONE', *, *, #111008, .T. ) ;
#31686 = ORIENTED_EDGE ( 'NONE', *, *, #24370, .T. ) ;
#31687 = DIRECTION ( 'NONE',  ( 0.000000000000000000, 0.000000000000000000, 1.000000000000000000 ) ) ;
#31688 = ADVANCED_FACE ( 'NONE', ( #124068 ), #28314, .T. ) ;
#31689 = CONICAL_SURFACE ( 'NONE', #104824, 0.09999999999999982514, 0.003490658503988666988 ) ;
#31690 = AXIS2_PLACEMENT_3D ( 'NONE', #53848, #93771, #95710 ) ;
#31691 = EDGE_CURVE ( 'NONE', #117766, #111163, #11579, .T. ) ;
#31692 = ORIENTED_EDGE ( 'NONE', *, *, #8159, .T. ) ;
#31693 = CARTESIAN_POINT ( 'NONE',  ( 17.88933034088538676, -0.4802206367769989992, -4.999988745082089459 ) ) ;
#31694 = FACE_OUTER_BOUND ( 'NONE', #101584, .T. ) ;
#31695 = EDGE_CURVE ( 'NONE', #69772, #124524, #83519, .T. ) ;
#31696 = DIRECTION ( 'NONE',  ( 0.000000000000000000, 0.000000000000000000, -1.000000000000000000 ) ) ;
#31697 = ORIENTED_EDGE ( 'NONE', *, *, #45022, .T. ) ;
#31698 = ADVANCED_FACE ( 'NONE', ( #122159 ), #49256, .T. ) ;
#31701 = ADVANCED_FACE ( 'NONE', ( #34426 ), #14733, .T. ) ;
#31700 = PLANE ( 'NONE',  #2775 ) ;
#31699 = VECTOR ( 'NONE', #93507, 1000.000000000000000 ) ;
#31702 = LINE ( 'NONE', #61156, #37030 ) ;
#31703 = AXIS2_PLACEMENT_3D ( 'NONE', #40956, #80862, #31130 ) ;
#31704 = ADVANCED_FACE ( 'NONE', ( #54048 ), #70084, .T. ) ;
#31705 = ORIENTED_EDGE ( 'NONE', *, *, #126602, .F. ) ;
#31706 = AXIS2_PLACEMENT_3D ( 'NONE', #56652, #96580, #104481 ) ;
#31707 = ORIENTED_EDGE ( 'NONE', *, *, #51166, .F. ) ;
#31708 = ORIENTED_EDGE ( 'NONE', *, *, #113933, .F. ) ;
#31709 = DIRECTION ( 'NONE',  ( 0.000000000000000000, 1.000000000000000000, 0.000000000000000000 ) ) ;
#31710 = DIRECTION ( 'NONE',  ( 0.000000000000000000, 1.000000000000000000, 0.000000000000000000 ) ) ;
#31711 = CARTESIAN_POINT ( 'NONE',  ( -2.700000000000031264, 12.50000000000000000, 4.676537180435972552 ) ) ;
#31712 = FACE_BOUND ( 'NONE', #10688, .T. ) ;
#31713 = EDGE_LOOP ( 'NONE', ( #125580, #63145 ) ) ;
#31714 = CARTESIAN_POINT ( 'NONE',  ( -5.200000000000020606, 2.500000000000000000, -0.3464101615137782364 ) ) ;
#31715 = DIRECTION ( 'NONE',  ( -0.000000000000000000, -1.000000000000000000, -0.000000000000000000 ) ) ;
#31716 = VERTEX_POINT ( 'NONE', #93972 ) ;
#31717 = CARTESIAN_POINT ( 'NONE',  ( 5.649999999999936406, 12.50000000000000000, -6.148780366869526226 ) ) ;
#31718 = CARTESIAN_POINT ( 'NONE',  ( -11.24999999999996447, 2.500000000000000000, -6.395190528383298378 ) ) ;
#31719 = DIRECTION ( 'NONE',  ( 0.000000000000000000, 1.000000000000000000, 0.000000000000000000 ) ) ;
#31720 = CARTESIAN_POINT ( 'NONE',  ( -1.450000000000035483, 2.500000000000000000, 1.718653347947321386 ) ) ;
#31721 = DIRECTION ( 'NONE',  ( 0.000000000000000000, 0.000000000000000000, 1.000000000000000000 ) ) ;
#31722 = DIRECTION ( 'NONE',  ( 0.000000000000000000, 0.000000000000000000, 1.000000000000000000 ) ) ;
#31723 = DIRECTION ( 'NONE',  ( 0.000000000000000000, -0.000000000000000000, 1.000000000000000000 ) ) ;
#31724 = CIRCLE ( 'NONE', #127864, 0.06509327318403745899 ) ;
#31725 = VECTOR ( 'NONE', #106182, 1000.000000000000000 ) ;
#31726 = ORIENTED_EDGE ( 'NONE', *, *, #61807, .F. ) ;
#31727 = ORIENTED_EDGE ( 'NONE', *, *, #13933, .F. ) ;
#31728 = ORIENTED_EDGE ( 'NONE', *, *, #113582, .T. ) ;
#31729 = ORIENTED_EDGE ( 'NONE', *, *, #95695, .F. ) ;
#31730 = DIRECTION ( 'NONE',  ( 0.000000000000000000, -0.9999939076577903929, 0.003490651415223739937 ) ) ;
#31731 = CARTESIAN_POINT ( 'NONE',  ( 1.249999999999988898, 12.50000000000000000, -6.430097255199264339 ) ) ;
#31732 = ORIENTED_EDGE ( 'NONE', *, *, #82729, .T. ) ;
#31733 = FACE_BOUND ( 'NONE', #89027, .T. ) ;
#31734 = VECTOR ( 'NONE', #39283, 1000.000000000000000 ) ;
#31735 = FACE_OUTER_BOUND ( 'NONE', #80687, .T. ) ;
#31736 = DIRECTION ( 'NONE',  ( -0.000000000000000000, -1.000000000000000000, -0.000000000000000000 ) ) ;
#31737 = CONICAL_SURFACE ( 'NONE', #4593, 0.1000000000000000056, 0.003490658503988666988 ) ;
#31738 = ADVANCED_FACE ( 'NONE', ( #23947 ), #95219, .T. ) ;
#31740 = DIRECTION ( 'NONE',  ( 0.000000000000000000, 1.000000000000000000, 0.000000000000000000 ) ) ;
#31739 = CIRCLE ( 'NONE', #34082, 0.06509327318403745899 ) ;
#31741 = CIRCLE ( 'NONE', #90495, 0.1000000000000002554 ) ;
#31742 = CIRCLE ( 'NONE', #125805, 5.200000000000000178 ) ;
#31743 = DIRECTION ( 'NONE',  ( -4.274815082592931898E-19, -0.9999939076577903929, -0.003490651415223739937 ) ) ;
#31744 = EDGE_CURVE ( 'NONE', #65177, #50078, #44885, .T. ) ;
#31745 = DIRECTION ( 'NONE',  ( 0.000000000000000000, 0.000000000000000000, 1.000000000000000000 ) ) ;
#31746 = DIRECTION ( 'NONE',  ( 0.000000000000000000, 0.000000000000000000, 1.000000000000000000 ) ) ;
#31747 = CARTESIAN_POINT ( 'NONE',  ( -13.54999999999999005, 2.500000000000000000, 2.511473670974877503 ) ) ;
#31748 = FACE_OUTER_BOUND ( 'NONE', #61658, .T. ) ;
#31749 = DIRECTION ( 'NONE',  ( -0.000000000000000000, 1.000000000000000000, -0.000000000000000000 ) ) ;
#31750 = EDGE_LOOP ( 'NONE', ( #27475, #79644, #39199, #34153 ) ) ;
#31751 = EDGE_CURVE ( 'NONE', #56139, #77490, #63868, .T. ) ;
#31752 = EDGE_LOOP ( 'NONE', ( #77279, #125395, #128894, #66555 ) ) ;
#31753 = PLANE ( 'NONE',  #4846 ) ;
#31754 = AXIS2_PLACEMENT_3D ( 'NONE', #114129, #33642, #123937 ) ;
#31755 = EDGE_CURVE ( 'NONE', #17445, #116268, #122786, .T. ) ;
#31756 = ORIENTED_EDGE ( 'NONE', *, *, #24040, .F. ) ;
#31757 = VERTEX_POINT ( 'NONE', #4270 ) ;
#31758 = VERTEX_POINT ( 'NONE', #92032 ) ;
#31760 = ORIENTED_EDGE ( 'NONE', *, *, #45751, .F. ) ;
#31759 = AXIS2_PLACEMENT_3D ( 'NONE', #26413, #104939, #65668 ) ;
#31761 = AXIS2_PLACEMENT_3D ( 'NONE', #47253, #18420, #87150 ) ;
#31762 = CIRCLE ( 'NONE', #98622, 0.09999999999999982514 ) ;
#31763 = CARTESIAN_POINT ( 'NONE',  ( 5.649999999999934630, 2.500000000000000000, 6.048780366869521252 ) ) ;
#31764 = EDGE_LOOP ( 'NONE', ( #85081, #42050 ) ) ;
#31765 = VERTEX_POINT ( 'NONE', #92680 ) ;
#31766 = CONICAL_SURFACE ( 'NONE', #60988, 0.09999999999999982514, 0.003490658503988666988 ) ;
#31767 = CARTESIAN_POINT ( 'NONE',  ( 12.89999999999990266, 2.500000000000000000, 5.022947341949748790 ) ) ;
#31768 = DIRECTION ( 'NONE',  ( 0.000000000000000000, 0.000000000000000000, -1.000000000000000000 ) ) ;
#31769 = DIRECTION ( 'NONE',  ( 0.000000000000000000, 0.000000000000000000, 1.000000000000000000 ) ) ;
#31770 = CARTESIAN_POINT ( 'NONE',  ( -13.29999999999999005, 12.50000000000000000, 1.843143693225357538E-15 ) ) ;
#31771 = EDGE_LOOP ( 'NONE', ( #4580, #30050 ) ) ;
#31772 = DIRECTION ( 'NONE',  ( -0.000000000000000000, -1.000000000000000000, -0.000000000000000000 ) ) ;
#31773 = VERTEX_POINT ( 'NONE', #53409 ) ;
#31774 = ORIENTED_EDGE ( 'NONE', *, *, #120752, .T. ) ;
#31775 = LINE ( 'NONE', #120151, #122141 ) ;
#31776 = DIRECTION ( 'NONE',  ( 0.000000000000000000, 0.000000000000000000, 1.000000000000000000 ) ) ;
#31777 = DIRECTION ( 'NONE',  ( 0.000000000000000000, 0.000000000000000000, -1.000000000000000000 ) ) ;
#31778 = VERTEX_POINT ( 'NONE', #103790 ) ;
#31779 = ORIENTED_EDGE ( 'NONE', *, *, #111159, .F. ) ;
#31780 = ADVANCED_FACE ( 'NONE', ( #2340 ), #72247, .T. ) ;
#31781 = CARTESIAN_POINT ( 'NONE',  ( -2.300000000000033129, 2.500000000000000000, 3.983716857408420076 ) ) ;
#31782 = CARTESIAN_POINT ( 'NONE',  ( 1.249999999999988898, 2.500000000000000000, -6.495190528383302464 ) ) ;
#31783 = LINE ( 'NONE', #50146, #3844 ) ;
#31785 = DIRECTION ( 'NONE',  ( 0.000000000000000000, 1.000000000000000000, 0.000000000000000000 ) ) ;
#31784 = CIRCLE ( 'NONE', #119591, 0.09999999999999982514 ) ;
#31786 = ORIENTED_EDGE ( 'NONE', *, *, #76780, .F. ) ;
#31787 = CIRCLE ( 'NONE', #33926, 0.06509327318403745899 ) ;
#31788 = AXIS2_PLACEMENT_3D ( 'NONE', #70752, #71372, #120499 ) ;
#31789 = CARTESIAN_POINT ( 'NONE',  ( -9.350000000000008527, 12.50000000000000000, -6.841600689897072485 ) ) ;
#31790 = ORIENTED_EDGE ( 'NONE', *, *, #912, .T. ) ;
#31791 = CARTESIAN_POINT ( 'NONE',  ( 11.75764115802628140, -2.499999999999999556, 7.679135278744470661 ) ) ;
#31792 = AXIS2_PLACEMENT_3D ( 'NONE', #23812, #104916, #45390 ) ;
#31794 = ORIENTED_EDGE ( 'NONE', *, *, #106127, .F. ) ;
#31793 = AXIS2_PLACEMENT_3D ( 'NONE', #17634, #116479, #115841 ) ;
#31795 = CARTESIAN_POINT ( 'NONE',  ( 87.50000000000002842, 6.761363245278263712, -3.308765358479923258 ) ) ;
#31796 = CIRCLE ( 'NONE', #33836, 0.06509327318403745899 ) ;
#31797 = PLANE ( 'NONE',  #96487 ) ;
#31798 = CARTESIAN_POINT ( 'NONE',  ( 10.84999999999990905, 2.500000000000000000, 2.165063509461097713 ) ) ;
#31799 = ADVANCED_FACE ( 'NONE', ( #14102 ), #22069, .T. ) ;
#31800 = AXIS2_PLACEMENT_3D ( 'NONE', #114736, #107504, #27016 ) ;
#31801 = DIRECTION ( 'NONE',  ( 0.000000000000000000, -0.9999939076577903929, 0.003490651415223739937 ) ) ;
#31802 = EDGE_CURVE ( 'NONE', #63751, #35293, #38807, .T. ) ;
#31803 = FACE_OUTER_BOUND ( 'NONE', #66794, .T. ) ;
#31804 = ORIENTED_EDGE ( 'NONE', *, *, #124857, .F. ) ;
#31805 = CIRCLE ( 'NONE', #52621, 0.1000000000000002554 ) ;
#31806 = DIRECTION ( 'NONE',  ( -0.000000000000000000, 1.000000000000000000, -0.000000000000000000 ) ) ;
#31807 = DIRECTION ( 'NONE',  ( 0.000000000000000000, 0.000000000000000000, 1.000000000000000000 ) ) ;
#31808 = ORIENTED_EDGE ( 'NONE', *, *, #96341, .T. ) ;
#31809 = EDGE_LOOP ( 'NONE', ( #57435, #4095, #73094, #46312 ) ) ;
#31811 = ORIENTED_EDGE ( 'NONE', *, *, #54920, .T. ) ;
#31810 = EDGE_CURVE ( 'NONE', #25500, #91178, #62590, .T. ) ;
#31812 = DIRECTION ( 'NONE',  ( -0.000000000000000000, 1.000000000000000000, -0.000000000000000000 ) ) ;
#31813 = LINE ( 'NONE', #119526, #15777 ) ;
#31814 = CARTESIAN_POINT ( 'NONE',  ( 186.0000000000000000, 0.000000000000000000, 7.700000000000000178 ) ) ;
#31815 = CARTESIAN_POINT ( 'NONE',  ( 5.649999999999936406, 2.500000000000000000, -6.841600689897077814 ) ) ;
#31816 = FACE_OUTER_BOUND ( 'NONE', #72332, .T. ) ;
#31817 = FACE_OUTER_BOUND ( 'NONE', #114357, .T. ) ;
#31818 = DIRECTION ( 'NONE',  ( 0.000000000000000000, -0.9999939076577903929, 0.003490651415223739937 ) ) ;
#31819 = AXIS2_PLACEMENT_3D ( 'NONE', #84127, #73663, #93324 ) ;
#31820 = EDGE_LOOP ( 'NONE', ( #100579, #13042, #2642, #66995 ) ) ;
#31821 = CARTESIAN_POINT ( 'NONE',  ( 105.0000000000000142, 8.500000000000000000, 0.2500000000000003886 ) ) ;
#31822 = DIRECTION ( 'NONE',  ( -0.000000000000000000, 1.000000000000000000, -0.000000000000000000 ) ) ;
#31823 = DIRECTION ( 'NONE',  ( -0.000000000000000000, -1.000000000000000000, -0.000000000000000000 ) ) ;
#31824 = DIRECTION ( 'NONE',  ( 0.000000000000000000, 0.000000000000000000, 1.000000000000000000 ) ) ;
#31825 = CIRCLE ( 'NONE', #10860, 0.06509327318403745899 ) ;
#31826 = AXIS2_PLACEMENT_3D ( 'NONE', #119349, #49999, #51287 ) ;
#31827 = ORIENTED_EDGE ( 'NONE', *, *, #80353, .T. ) ;
#31828 = DIRECTION ( 'NONE',  ( 0.000000000000000000, 0.000000000000000000, 1.000000000000000000 ) ) ;
#31829 = ADVANCED_FACE ( 'NONE', ( #12806 ), #93330, .T. ) ;
#31830 = VECTOR ( 'NONE', #57913, 1000.000000000000000 ) ;
#31831 = CARTESIAN_POINT ( 'NONE',  ( -9.350000000000004974, 2.500000000000000000, 6.741600689897071952 ) ) ;
#31833 = ORIENTED_EDGE ( 'NONE', *, *, #49112, .F. ) ;
#31832 = DIRECTION ( 'NONE',  ( 0.000000000000000000, 1.000000000000000000, 0.000000000000000000 ) ) ;
#31834 = ADVANCED_FACE ( 'NONE', ( #73041 ), #32540, .T. ) ;
#31835 = EDGE_CURVE ( 'NONE', #88926, #17926, #16033, .T. ) ;
#31836 = EDGE_CURVE ( 'NONE', #68676, #113589, #95268, .T. ) ;
#31837 = ORIENTED_EDGE ( 'NONE', *, *, #98731, .F. ) ;
#31839 = CIRCLE ( 'NONE', #44350, 0.06509327318403745899 ) ;
#31838 = DIRECTION ( 'NONE',  ( -0.000000000000000000, 1.000000000000000000, -0.000000000000000000 ) ) ;
#31840 = ORIENTED_EDGE ( 'NONE', *, *, #122973, .F. ) ;
#31841 = CIRCLE ( 'NONE', #125911, 0.09999999999999982514 ) ;
#31843 = ORIENTED_EDGE ( 'NONE', *, *, #99351, .F. ) ;
#31842 = CIRCLE ( 'NONE', #21466, 0.09999999999999982514 ) ;
#31844 = AXIS2_PLACEMENT_3D ( 'NONE', #127069, #36761, #64900 ) ;
#31845 = PLANE ( 'NONE',  #80170 ) ;
#31846 = ADVANCED_FACE ( 'NONE', ( #86725 ), #109889, .T. ) ;
#31847 = ADVANCED_FACE ( 'NONE', ( #87992 ), #126616, .T. ) ;
#31848 = EDGE_CURVE ( 'NONE', #126587, #116590, #103531, .T. ) ;
#31849 = AXIS2_PLACEMENT_3D ( 'NONE', #83084, #93536, #81768 ) ;
#31850 = CARTESIAN_POINT ( 'NONE',  ( -1.700000000000034817, 2.500000000000000000, 0.09999999999999761857 ) ) ;
#31851 = CARTESIAN_POINT ( 'NONE',  ( -1.450000000000035483, 2.500000000000000000, 6.248780366869521430 ) ) ;
#31852 = CARTESIAN_POINT ( 'NONE',  ( 129.5000000000000000, 1.500000000000000000, 0.000000000000000000 ) ) ;
#31853 = VERTEX_POINT ( 'NONE', #36359 ) ;
#31854 = EDGE_CURVE ( 'NONE', #106131, #56932, #30394, .T. ) ;
#31855 = FACE_OUTER_BOUND ( 'NONE', #109151, .T. ) ;
#31856 = EDGE_LOOP ( 'NONE', ( #120952, #58498, #93108, #42968 ) ) ;
#31857 = FACE_OUTER_BOUND ( 'NONE', #44225, .T. ) ;
#31858 = EDGE_CURVE ( 'NONE', #108453, #97422, #97262, .T. ) ;
#31859 = CARTESIAN_POINT ( 'NONE',  ( -5.850000000000021849, 2.500000000000000000, -2.857883832488653741 ) ) ;
#31860 = EDGE_CURVE ( 'NONE', #63793, #90411, #57572, .T. ) ;
#31861 = EDGE_LOOP ( 'NONE', ( #28954, #56606, #115798, #72902 ) ) ;
#31862 = ORIENTED_EDGE ( 'NONE', *, *, #95922, .F. ) ;
#31863 = ORIENTED_EDGE ( 'NONE', *, *, #99106, .F. ) ;
#31864 = VERTEX_POINT ( 'NONE', #35700 ) ;
#31865 = CARTESIAN_POINT ( 'NONE',  ( -4.800000000000022915, 12.50000000000000000, 3.983716857408420076 ) ) ;
#31866 = CARTESIAN_POINT ( 'NONE',  ( 1.649999999999950617, 12.50000000000000000, -2.099970236277064473 ) ) ;
#31867 = FACE_BOUND ( 'NONE', #46609, .T. ) ;
#31868 = VERTEX_POINT ( 'NONE', #76907 ) ;
#31869 = DIRECTION ( 'NONE',  ( 0.000000000000000000, -0.9999939076577903929, 0.003490651415223739937 ) ) ;
#31870 = CARTESIAN_POINT ( 'NONE',  ( 187.0260416670080588, -6.551208109652273848, -3.782341765625003571 ) ) ;
#31871 = CARTESIAN_POINT ( 'NONE',  ( 0.000000000000000000, 2.500000000000000000, -8.999999999999998224 ) ) ;
#31872 = CARTESIAN_POINT ( 'NONE',  ( 10.84999999999990905, 12.50000000000000000, 2.922977105672686982 ) ) ;
#31873 = CONICAL_SURFACE ( 'NONE', #107159, 0.09999999999999982514, 0.003490658503988666988 ) ;
#31874 = AXIS2_PLACEMENT_3D ( 'NONE', #80543, #120456, #58333 ) ;
#31876 = CIRCLE ( 'NONE', #105014, 0.06509327318403745899 ) ;
#31875 = CARTESIAN_POINT ( 'NONE',  ( 15.19999999999989271, 2.500000000000000000, -0.3464101615137783474 ) ) ;
#31877 = DIRECTION ( 'NONE',  ( 0.000000000000000000, -0.000000000000000000, 1.000000000000000000 ) ) ;
#31878 = CARTESIAN_POINT ( 'NONE',  ( -6.249999999999981348, 12.50000000000000000, 6.495190528383297135 ) ) ;
#31879 = AXIS2_PLACEMENT_3D ( 'NONE', #73312, #73971, #113238 ) ;
#31880 = DIRECTION ( 'NONE',  ( -4.274815082592931898E-19, -0.9999939076577903929, -0.003490651415223739937 ) ) ;
#31881 = CONICAL_SURFACE ( 'NONE', #105022, 0.09999999999999982514, 0.003490658503988666988 ) ;
#31882 = ORIENTED_EDGE ( 'NONE', *, *, #88997, .F. ) ;
#31883 = VERTEX_POINT ( 'NONE', #127942 ) ;
#31884 = ORIENTED_EDGE ( 'NONE', *, *, #12521, .F. ) ;
#31885 = EDGE_LOOP ( 'NONE', ( #70207, #58153 ) ) ;
#31887 = EDGE_LOOP ( 'NONE', ( #66301, #72796, #78817, #72856 ) ) ;
#31886 = VECTOR ( 'NONE', #84065, 1000.000000000000000 ) ;
#31888 = DIRECTION ( 'NONE',  ( 0.000000000000000000, -0.000000000000000000, -1.000000000000000000 ) ) ;
#31889 = CONICAL_SURFACE ( 'NONE', #88291, 0.1000000000000002554, 0.003490658503988666988 ) ;
#31890 = CARTESIAN_POINT ( 'NONE',  ( -7.100000000000014744, 2.500000000000000000, 4.430127018922196847 ) ) ;
#31891 = ORIENTED_EDGE ( 'NONE', *, *, #50023, .T. ) ;
#31892 = FACE_BOUND ( 'NONE', #39959, .T. ) ;
#31893 = CIRCLE ( 'NONE', #113356, 0.06509327318403745899 ) ;
#31894 = FACE_OUTER_BOUND ( 'NONE', #1479, .T. ) ;
#31895 = EDGE_CURVE ( 'NONE', #97989, #20397, #74291, .T. ) ;
#31896 = EDGE_CURVE ( 'NONE', #83631, #87862, #112028, .T. ) ;
#31897 = VERTEX_POINT ( 'NONE', #57924 ) ;
#31898 = CARTESIAN_POINT ( 'NONE',  ( -6.650000000000018119, 2.500000000000000000, -7.288010851410854585 ) ) ;
#31899 = DIRECTION ( 'NONE',  ( 0.000000000000000000, 0.000000000000000000, -1.000000000000000000 ) ) ;
#31900 = DIRECTION ( 'NONE',  ( 0.000000000000000000, 1.000000000000000000, 0.000000000000000000 ) ) ;
#31901 = DIRECTION ( 'NONE',  ( 0.000000000000000000, 0.000000000000000000, 1.000000000000000000 ) ) ;
#31902 = EDGE_LOOP ( 'NONE', ( #76291, #84501, #33757, #71063 ) ) ;
#31903 = FACE_OUTER_BOUND ( 'NONE', #12249, .T. ) ;
#31904 = AXIS2_PLACEMENT_3D ( 'NONE', #21888, #12038, #51987 ) ;
#31905 = VERTEX_POINT ( 'NONE', #75601 ) ;
#31906 = ORIENTED_EDGE ( 'NONE', *, *, #87389, .F. ) ;
#31907 = ORIENTED_EDGE ( 'NONE', *, *, #93575, .T. ) ;
#31908 = DIRECTION ( 'NONE',  ( -0.000000000000000000, 1.000000000000000000, -0.000000000000000000 ) ) ;
#31909 = CARTESIAN_POINT ( 'NONE',  ( -2.700000000000030820, 12.50000000000000000, -3.983716857408426293 ) ) ;
#31910 = EDGE_LOOP ( 'NONE', ( #51352, #41870, #4303, #26707 ) ) ;
#31911 = CARTESIAN_POINT ( 'NONE',  ( -6.450000000000014388, 12.50000000000000000, 6.083687093685483660 ) ) ;
#31912 = CONICAL_SURFACE ( 'NONE', #65336, 0.1000000000000000472, 0.003490658503988666988 ) ;
#31914 = DIRECTION ( 'NONE',  ( 0.000000000000000000, 1.000000000000000000, 0.000000000000000000 ) ) ;
#31913 = AXIS2_PLACEMENT_3D ( 'NONE', #44185, #74306, #95236 ) ;
#31915 = PLANE ( 'NONE',  #39455 ) ;
#31916 = FACE_OUTER_BOUND ( 'NONE', #10286, .T. ) ;
#31917 = CARTESIAN_POINT ( 'NONE',  ( 186.3229166673494603, -4.445597072760122614, 7.699999999999998401 ) ) ;
#31918 = EDGE_LOOP ( 'NONE', ( #111154, #119249, #49947, #58642 ) ) ;
#31919 = CARTESIAN_POINT ( 'NONE',  ( 3.949999999999940670, 12.50000000000000000, 1.818653347947321475 ) ) ;
#31920 = AXIS2_PLACEMENT_3D ( 'NONE', #108314, #77560, #49419 ) ;
#31921 = ORIENTED_EDGE ( 'NONE', *, *, #123415, .F. ) ;
#31922 = CARTESIAN_POINT ( 'NONE',  ( 1.899999999999949507, 12.50000000000000000, 4.676537180435972552 ) ) ;
#31923 = VECTOR ( 'NONE', #103596, 1000.000000000000000 ) ;
#31924 = CIRCLE ( 'NONE', #10955, 0.09999999999999982514 ) ;
#31925 = EDGE_LOOP ( 'NONE', ( #88584, #99379, #103054, #125136 ) ) ;
#31926 = CIRCLE ( 'NONE', #40234, 7.700000000000000178 ) ;
#31927 = CARTESIAN_POINT ( 'NONE',  ( 1.649999999999951505, 2.500000000000000000, 2.857883832488649301 ) ) ;
#31928 = VERTEX_POINT ( 'NONE', #97193 ) ;
#31929 = DIRECTION ( 'NONE',  ( -4.274815082592931898E-19, -0.9999939076577903929, -0.003490651415223739937 ) ) ;
#31930 = DIRECTION ( 'NONE',  ( -0.000000000000000000, -1.000000000000000000, -0.000000000000000000 ) ) ;
#31931 = CARTESIAN_POINT ( 'NONE',  ( -10.40000000000000391, 12.50000000000000000, -3.637306695894645614 ) ) ;
#31932 = DIRECTION ( 'NONE',  ( 0.000000000000000000, 1.000000000000000000, 0.000000000000000000 ) ) ;
#31933 = DIRECTION ( 'NONE',  ( 0.000000000000000000, 0.000000000000000000, 1.000000000000000000 ) ) ;
#31934 = AXIS2_PLACEMENT_3D ( 'NONE', #28807, #8490, #99484 ) ;
#31935 = VERTEX_POINT ( 'NONE', #115519 ) ;
#31936 = ORIENTED_EDGE ( 'NONE', *, *, #80339, .F. ) ;
#31937 = CIRCLE ( 'NONE', #84138, 0.06509327318403741736 ) ;
#31939 = EDGE_LOOP ( 'NONE', ( #36615, #39684, #126377, #121351 ) ) ;
#31938 = EDGE_CURVE ( 'NONE', #28339, #116464, #105728, .T. ) ;
#31940 = CARTESIAN_POINT ( 'NONE',  ( 11.64999999999990443, 12.50000000000000000, 1.407149913249508000 ) ) ;
#31941 = CARTESIAN_POINT ( 'NONE',  ( -10.85000000000000142, 2.500000000000000000, -5.702370205355745902 ) ) ;
#31942 = VECTOR ( 'NONE', #24865, 1000.000000000000000 ) ;
#31943 = VECTOR ( 'NONE', #68124, 1000.000000000000000 ) ;
#31944 = CARTESIAN_POINT ( 'NONE',  ( 9.549999999999918998, 12.50000000000000000, 2.165063509461097713 ) ) ;
#31946 = ORIENTED_EDGE ( 'NONE', *, *, #14435, .T. ) ;
#31945 = EDGE_LOOP ( 'NONE', ( #27379, #8814, #30290, #34994 ) ) ;
#31947 = VERTEX_POINT ( 'NONE', #46151 ) ;
#31948 = DIRECTION ( 'NONE',  ( 0.000000000000000000, 0.000000000000000000, 1.000000000000000000 ) ) ;
#31949 = VECTOR ( 'NONE', #118326, 1000.000000000000000 ) ;
#31950 = EDGE_LOOP ( 'NONE', ( #2429, #104518, #128921, #94351 ) ) ;
#31952 = ADVANCED_FACE ( 'NONE', ( #116821 ), #61869, .T. ) ;
#31951 = FACE_OUTER_BOUND ( 'NONE', #10259, .T. ) ;
#31953 = FACE_OUTER_BOUND ( 'NONE', #50549, .T. ) ;
#31954 = DIRECTION ( 'NONE',  ( 0.000000000000000000, 1.000000000000000000, 0.000000000000000000 ) ) ;
#31955 = AXIS2_PLACEMENT_3D ( 'NONE', #97412, #28688, #59456 ) ;
#31956 = DIRECTION ( 'NONE',  ( -0.000000000000000000, -1.000000000000000000, -0.000000000000000000 ) ) ;
#31957 = DIRECTION ( 'NONE',  ( 0.000000000000000000, 0.000000000000000000, 1.000000000000000000 ) ) ;
#31958 = DIRECTION ( 'NONE',  ( -4.274815082592931898E-19, -0.9999939076577903929, -0.003490651415223739937 ) ) ;
#31959 = DIRECTION ( 'NONE',  ( 0.000000000000000000, -0.000000000000000000, 1.000000000000000000 ) ) ;
#31960 = EDGE_CURVE ( 'NONE', #74521, #34772, #22172, .T. ) ;
#31961 = ADVANCED_FACE ( 'NONE', ( #6847 ), #13717, .T. ) ;
#31962 = DIRECTION ( 'NONE',  ( 0.000000000000000000, 0.000000000000000000, 1.000000000000000000 ) ) ;
#31963 = EDGE_LOOP ( 'NONE', ( #125188, #58814, #58710, #107341 ) ) ;
#31964 = CARTESIAN_POINT ( 'NONE',  ( -5.650000000000023448, 2.500000000000000000, -2.511473670974877948 ) ) ;
#31965 = ADVANCED_FACE ( 'NONE', ( #77540 ), #80642, .T. ) ;
#31966 = CARTESIAN_POINT ( 'NONE',  ( 76.45351065593905560, -3.568406926272937874, 6.085611128998389852 ) ) ;
#31967 = ORIENTED_EDGE ( 'NONE', *, *, #71849, .F. ) ;
#31968 = EDGE_LOOP ( 'NONE', ( #60226, #37645, #37676, #16483 ) ) ;
#31969 = AXIS2_PLACEMENT_3D ( 'NONE', #48521, #129040, #53 ) ;
#31970 = CIRCLE ( 'NONE', #105093, 0.06509327318403745899 ) ;
#31971 = ADVANCED_FACE ( 'NONE', ( #8155 ), #70172, .T. ) ;
#31972 = CARTESIAN_POINT ( 'NONE',  ( 187.2968750003414300, 8.734944146203032389, 5.348610694689227483E-16 ) ) ;
#31973 = CARTESIAN_POINT ( 'NONE',  ( 5.849999999999932143, 12.50000000000000000, 1.472243186433545459 ) ) ;
#31974 = CARTESIAN_POINT ( 'NONE',  ( 8.349999999999919709, 2.500000000000000000, -1.472243186433550122 ) ) ;
#31975 = CARTESIAN_POINT ( 'NONE',  ( -1.250000000000001554, 2.500000000000000000, 6.595190528383296780 ) ) ;
#31976 = DIRECTION ( 'NONE',  ( 0.000000000000000000, 0.000000000000000000, 1.000000000000000000 ) ) ;
#31977 = DIRECTION ( 'NONE',  ( 0.000000000000000000, 0.000000000000000000, 1.000000000000000000 ) ) ;
#31978 = CONICAL_SURFACE ( 'NONE', #17358, 0.1000000000000002554, 0.003490658503988666988 ) ;
#31979 = CARTESIAN_POINT ( 'NONE',  ( 8.149999999999923972, 2.500000000000000000, -6.148780366869526226 ) ) ;
#31980 = CARTESIAN_POINT ( 'NONE',  ( 4.399999999999937295, 12.50000000000000000, 3.918623584224383727 ) ) ;
#31981 = CONICAL_SURFACE ( 'NONE', #98758, 0.09999999999999982514, 0.003490658503988666988 ) ;
#31982 = AXIS2_PLACEMENT_3D ( 'NONE', #35670, #74308, #44853 ) ;
#31983 = DIRECTION ( 'NONE',  ( 0.000000000000000000, 0.000000000000000000, 1.000000000000000000 ) ) ;
#31984 = VERTEX_POINT ( 'NONE', #50669 ) ;
#31985 = AXIS2_PLACEMENT_3D ( 'NONE', #60340, #9929, #38109 ) ;
#31986 = ORIENTED_EDGE ( 'NONE', *, *, #48014, .F. ) ;
#31987 = CIRCLE ( 'NONE', #48706, 0.06509327318403745899 ) ;
#31988 = CONICAL_SURFACE ( 'NONE', #6802, 0.1000000000000002554, 0.003490658503988666988 ) ;
#31989 = ORIENTED_EDGE ( 'NONE', *, *, #56500, .F. ) ;
#31990 = AXIS2_PLACEMENT_3D ( 'NONE', #90505, #81356, #847 ) ;
#31991 = AXIS2_PLACEMENT_3D ( 'NONE', #101095, #20611, #31092 ) ;
#31992 = ORIENTED_EDGE ( 'NONE', *, *, #122307, .T. ) ;
#31993 = FACE_OUTER_BOUND ( 'NONE', #12049, .T. ) ;
#31994 = FACE_OUTER_BOUND ( 'NONE', #85985, .T. ) ;
#31995 = AXIS2_PLACEMENT_3D ( 'NONE', #30543, #72395, #23259 ) ;
#31996 = ORIENTED_EDGE ( 'NONE', *, *, #54442, .F. ) ;
#31997 = FACE_OUTER_BOUND ( 'NONE', #26607, .T. ) ;
#31998 = ADVANCED_FACE ( 'NONE', ( #50056 ), #24204, .T. ) ;
#31999 = DIRECTION ( 'NONE',  ( 0.000000000000000000, -0.9999939076577903929, 0.003490651415223739937 ) ) ;
#32000 = FACE_OUTER_BOUND ( 'NONE', #109169, .T. ) ;
#32002 = VERTEX_POINT ( 'NONE', #40880 ) ;
#32001 = DIRECTION ( 'NONE',  ( 0.000000000000000000, 1.000000000000000000, 0.000000000000000000 ) ) ;
#32003 = ADVANCED_FACE ( 'NONE', ( #39597 ), #91093, .T. ) ;
#32004 = DIRECTION ( 'NONE',  ( 0.000000000000000000, 1.000000000000000000, 0.000000000000000000 ) ) ;
#32005 = ADVANCED_FACE ( 'NONE', ( #120059 ), #47190, .T. ) ;
#32007 = CARTESIAN_POINT ( 'NONE',  ( 8.099999999999923261, 2.500000000000000000, -3.983716857408426293 ) ) ;
#32006 = AXIS2_PLACEMENT_3D ( 'NONE', #41536, #60528, #81443 ) ;
#32008 = ORIENTED_EDGE ( 'NONE', *, *, #75595, .T. ) ;
#32009 = ORIENTED_EDGE ( 'NONE', *, *, #68733, .T. ) ;
#32010 = VERTEX_POINT ( 'NONE', #1561 ) ;
#32011 = VERTEX_POINT ( 'NONE', #30413 ) ;
#32012 = DIRECTION ( 'NONE',  ( -0.000000000000000000, 1.000000000000000000, -0.000000000000000000 ) ) ;
#32013 = EDGE_CURVE ( 'NONE', #6668, #36299, #82802, .T. ) ;
#32014 = ADVANCED_FACE ( 'NONE', ( #31057 ), #30485, .T. ) ;
#32015 = EDGE_CURVE ( 'NONE', #56105, #85940, #95304, .T. ) ;
#32016 = EDGE_CURVE ( 'NONE', #10801, #5618, #108925, .T. ) ;
#32018 = AXIS2_PLACEMENT_3D ( 'NONE', #66911, #106833, #119091 ) ;
#32017 = LINE ( 'NONE', #12346, #90571 ) ;
#32019 = DIRECTION ( 'NONE',  ( -0.000000000000000000, -1.000000000000000000, -0.000000000000000000 ) ) ;
#32020 = AXIS2_PLACEMENT_3D ( 'NONE', #123317, #104944, #56499 ) ;
#32021 = ORIENTED_EDGE ( 'NONE', *, *, #63, .F. ) ;
#32022 = EDGE_CURVE ( 'NONE', #78167, #5697, #101563, .T. ) ;
#32023 = LINE ( 'NONE', #100725, #46043 ) ;
#32024 = EDGE_LOOP ( 'NONE', ( #123851, #82598, #67197, #27906 ) ) ;
#32025 = LINE ( 'NONE', #92202, #72600 ) ;
#32026 = CARTESIAN_POINT ( 'NONE',  ( 16.55874544816221317, -0.4845305829210151960, -6.091953208799018249 ) ) ;
#32027 = DIRECTION ( 'NONE',  ( -0.000000000000000000, -1.000000000000000000, -0.000000000000000000 ) ) ;
#32028 = CARTESIAN_POINT ( 'NONE',  ( 5.849999999999933920, 2.500000000000000000, 5.902370205355745192 ) ) ;
#32029 = CIRCLE ( 'NONE', #4793, 0.06509327318403745899 ) ;
#32030 = ADVANCED_FACE ( 'NONE', ( #41522 ), #81431, .T. ) ;
#32031 = EDGE_CURVE ( 'NONE', #90584, #47691, #15871, .T. ) ;
#32032 = VECTOR ( 'NONE', #128365, 1000.000000000000000 ) ;
#32033 = VERTEX_POINT ( 'NONE', #118763 ) ;
#32034 = CONICAL_SURFACE ( 'NONE', #84226, 0.1000000000000002554, 0.003490658503988666988 ) ;
#32035 = ORIENTED_EDGE ( 'NONE', *, *, #13621, .F. ) ;
#32036 = ORIENTED_EDGE ( 'NONE', *, *, #85429, .T. ) ;
#32037 = CARTESIAN_POINT ( 'NONE',  ( 4.999999999999938716, 2.500000000000000000, -4.922947341949753586 ) ) ;
#32038 = DIRECTION ( 'NONE',  ( -0.000000000000000000, 1.000000000000000000, -0.000000000000000000 ) ) ;
#32039 = CARTESIAN_POINT ( 'NONE',  ( 1.249999999999952038, 12.50000000000000000, 5.802370205355744659 ) ) ;
#32040 = FACE_BOUND ( 'NONE', #93401, .T. ) ;
#32041 = CARTESIAN_POINT ( 'NONE',  ( 10.59999999999991260, 2.500000000000000000, 0.3464101615137735735 ) ) ;
#32043 = DIRECTION ( 'NONE',  ( 0.000000000000000000, -0.000000000000000000, 1.000000000000000000 ) ) ;
#32042 = AXIS2_PLACEMENT_3D ( 'NONE', #55535, #35888, #75796 ) ;
#32044 = FACE_OUTER_BOUND ( 'NONE', #19473, .T. ) ;
#32045 = CONICAL_SURFACE ( 'NONE', #80051, 0.09999999999999982514, 0.003490658503988666988 ) ;
#32046 = CIRCLE ( 'NONE', #69669, 0.06509327318403745899 ) ;
#32047 = AXIS2_PLACEMENT_3D ( 'NONE', #58810, #29361, #69252 ) ;
#32048 = DIRECTION ( 'NONE',  ( 0.000000000000000000, -0.9999939076577903929, 0.003490651415223739937 ) ) ;
#32049 = DIRECTION ( 'NONE',  ( 0.000000000000000000, 0.000000000000000000, -1.000000000000000000 ) ) ;
#32050 = DIRECTION ( 'NONE',  ( 0.000000000000000000, 0.000000000000000000, -1.000000000000000000 ) ) ;
#32051 = EDGE_LOOP ( 'NONE', ( #37068, #122020 ) ) ;
#32052 = DIRECTION ( 'NONE',  ( -0.000000000000000000, -1.000000000000000000, -0.000000000000000000 ) ) ;
#32053 = CARTESIAN_POINT ( 'NONE',  ( 6.649999999999931966, 12.50000000000000000, -7.188010851410854052 ) ) ;
#32054 = AXIS2_PLACEMENT_3D ( 'NONE', #76343, #48825, #86793 ) ;
#32055 = EDGE_LOOP ( 'NONE', ( #4427, #125352 ) ) ;
#32056 = ORIENTED_EDGE ( 'NONE', *, *, #119322, .T. ) ;
#32057 = CARTESIAN_POINT ( 'NONE',  ( 7.099999999999927702, 2.500000000000000000, 5.022947341949748790 ) ) ;
#32058 = DIRECTION ( 'NONE',  ( 0.000000000000000000, 0.000000000000000000, 1.000000000000000000 ) ) ;
#32059 = FACE_BOUND ( 'NONE', #9868, .T. ) ;
#32060 = LINE ( 'NONE', #43812, #124591 ) ;
#32061 = ADVANCED_FACE ( 'NONE', ( #8796 ), #107819, .T. ) ;
#32063 = ORIENTED_EDGE ( 'NONE', *, *, #33319, .F. ) ;
#32062 = CIRCLE ( 'NONE', #59253, 0.06509327318403745899 ) ;
#32065 = AXIS2_PLACEMENT_3D ( 'NONE', #118846, #48836, #98541 ) ;
#32064 = DIRECTION ( 'NONE',  ( 0.000000000000000000, 0.000000000000000000, 1.000000000000000000 ) ) ;
#32066 = CARTESIAN_POINT ( 'NONE',  ( 184.7916666666666856, 4.445597072760120838, -7.699999999999998401 ) ) ;
#32067 = EDGE_LOOP ( 'NONE', ( #82801, #126818 ) ) ;
#32068 = DIRECTION ( 'NONE',  ( 0.000000000000000000, 0.000000000000000000, 1.000000000000000000 ) ) ;
#32069 = FACE_OUTER_BOUND ( 'NONE', #69876, .T. ) ;
#32070 = EDGE_CURVE ( 'NONE', #49864, #179, #57653, .T. ) ;
#32071 = AXIS2_PLACEMENT_3D ( 'NONE', #47461, #69020, #46824 ) ;
#32072 = CONICAL_SURFACE ( 'NONE', #40383, 0.1000000000000002554, 0.003490658503988666988 ) ;
#32073 = AXIS2_PLACEMENT_3D ( 'NONE', #101031, #60485, #42785 ) ;
#32074 = ORIENTED_EDGE ( 'NONE', *, *, #104631, .F. ) ;
#32075 = DIRECTION ( 'NONE',  ( -0.000000000000000000, 1.000000000000000000, -0.000000000000000000 ) ) ;
#32076 = DIRECTION ( 'NONE',  ( 0.000000000000000000, 1.000000000000000000, 0.000000000000000000 ) ) ;
#32077 = CIRCLE ( 'NONE', #38333, 0.06509327318403745899 ) ;
#32079 = ORIENTED_EDGE ( 'NONE', *, *, #69792, .T. ) ;
#32078 = AXIS2_PLACEMENT_3D ( 'NONE', #11534, #51477, #31828 ) ;
#32080 = DIRECTION ( 'NONE',  ( 0.000000000000000000, 0.000000000000000000, 1.000000000000000000 ) ) ;
#32081 = DIRECTION ( 'NONE',  ( 0.000000000000000000, 0.000000000000000000, -1.000000000000000000 ) ) ;
#32082 = DIRECTION ( 'NONE',  ( -0.000000000000000000, -1.000000000000000000, 0.000000000000000000 ) ) ;
#32084 = EDGE_LOOP ( 'NONE', ( #127991, #95354 ) ) ;
#32083 = CIRCLE ( 'NONE', #90554, 0.06509327318403745899 ) ;
#32085 = ORIENTED_EDGE ( 'NONE', *, *, #122403, .T. ) ;
#32086 = DIRECTION ( 'NONE',  ( 0.000000000000000000, 1.000000000000000000, 0.000000000000000000 ) ) ;
#32087 = AXIS2_PLACEMENT_3D ( 'NONE', #60328, #1370, #9914 ) ;
#32088 = VERTEX_POINT ( 'NONE', #9461 ) ;
#32089 = LINE ( 'NONE', #62824, #72136 ) ;
#32090 = CARTESIAN_POINT ( 'NONE',  ( 129.5000000000000000, 0.6250000000000028866, -7.634788798650556707 ) ) ;
#32091 = DIRECTION ( 'NONE',  ( -0.000000000000000000, 1.000000000000000000, -0.000000000000000000 ) ) ;
#32092 = ORIENTED_EDGE ( 'NONE', *, *, #80299, .T. ) ;
#32093 = CARTESIAN_POINT ( 'NONE',  ( -5.650000000000023448, 12.50000000000000000, -6.213873640053564351 ) ) ;
#32094 = CARTESIAN_POINT ( 'NONE',  ( 7.949999999999925571, 2.500000000000000000, 2.065063509461097624 ) ) ;
#32095 = DIRECTION ( 'NONE',  ( 0.000000000000000000, 1.000000000000000000, 0.000000000000000000 ) ) ;
#32096 = FACE_OUTER_BOUND ( 'NONE', #54216, .T. ) ;
#32097 = CARTESIAN_POINT ( 'NONE',  ( 1.249999999999954259, 2.500000000000000000, -7.188010851410854052 ) ) ;
#32098 = CARTESIAN_POINT ( 'NONE',  ( 4.599999999999940137, 12.50000000000000000, -4.330127018922201643 ) ) ;
#32099 = CIRCLE ( 'NONE', #105233, 0.09999999999999999167 ) ;
#32100 = ORIENTED_EDGE ( 'NONE', *, *, #128348, .T. ) ;
#32101 = ORIENTED_EDGE ( 'NONE', *, *, #7076, .F. ) ;
#32102 = DIRECTION ( 'NONE',  ( 0.000000000000000000, -1.000000000000000000, 0.000000000000000000 ) ) ;
#32103 = ORIENTED_EDGE ( 'NONE', *, *, #119597, .T. ) ;
#32104 = CARTESIAN_POINT ( 'NONE',  ( 3.149999999999946176, 2.500000000000000000, -6.048780366869526581 ) ) ;
#32106 = ORIENTED_EDGE ( 'NONE', *, *, #33064, .T. ) ;
#32105 = ORIENTED_EDGE ( 'NONE', *, *, #37618, .T. ) ;
#32107 = ORIENTED_EDGE ( 'NONE', *, *, #86638, .T. ) ;
#32108 = DIRECTION ( 'NONE',  ( -0.000000000000000000, 1.000000000000000000, -0.000000000000000000 ) ) ;
#32109 = VECTOR ( 'NONE', #104594, 1000.000000000000000 ) ;
#32110 = CIRCLE ( 'NONE', #67676, 0.1000000000000002554 ) ;
#32112 = EDGE_CURVE ( 'NONE', #102565, #125530, #1213, .T. ) ;
#32111 = DIRECTION ( 'NONE',  ( 0.000000000000000000, 0.000000000000000000, 1.000000000000000000 ) ) ;
#32113 = AXIS2_PLACEMENT_3D ( 'NONE', #110404, #11554, #120239 ) ;
#32114 = CARTESIAN_POINT ( 'NONE',  ( -12.09999999999999609, 2.500000000000000000, -3.637306695894647390 ) ) ;
#32115 = CARTESIAN_POINT ( 'NONE',  ( -2.700000000000030820, 12.50000000000000000, -4.048810130592463530 ) ) ;
#32116 = FACE_OUTER_BOUND ( 'NONE', #104746, .T. ) ;
#32117 = DIRECTION ( 'NONE',  ( -4.274815082592931898E-19, -0.9999939076577903929, -0.003490651415223739937 ) ) ;
#32118 = DIRECTION ( 'NONE',  ( 0.000000000000000000, -0.9999939076577903929, 0.003490651415223739937 ) ) ;
#32119 = FACE_OUTER_BOUND ( 'NONE', #17270, .T. ) ;
#32120 = ADVANCED_FACE ( 'NONE', ( #58570 ), #99778, .T. ) ;
#32121 = AXIS2_PLACEMENT_3D ( 'NONE', #28816, #9164, #68719 ) ;
#32122 = EDGE_CURVE ( 'NONE', #87037, #16575, #118279, .T. ) ;
#32123 = CIRCLE ( 'NONE', #27895, 0.1000000000000002554 ) ;
#32124 = CARTESIAN_POINT ( 'NONE',  ( 187.5000000000000000, 0.9999999999999985567, -7.634788798650556707 ) ) ;
#32125 = CIRCLE ( 'NONE', #128264, 3.000000000000000000 ) ;
#32126 = EDGE_LOOP ( 'NONE', ( #68539, #116980, #16479, #99340 ) ) ;
#32127 = AXIS2_PLACEMENT_3D ( 'NONE', #42642, #82556, #11855 ) ;
#32128 = EDGE_CURVE ( 'NONE', #45762, #120531, #59225, .T. ) ;
#32129 = DIRECTION ( 'NONE',  ( -4.274815082592931898E-19, -0.9999939076577903929, -0.003490651415223739937 ) ) ;
#32130 = ORIENTED_EDGE ( 'NONE', *, *, #4353, .F. ) ;
#32131 = ORIENTED_EDGE ( 'NONE', *, *, #87210, .T. ) ;
#32132 = EDGE_CURVE ( 'NONE', #105289, #38108, #2859, .T. ) ;
#32133 = DIRECTION ( 'NONE',  ( -0.000000000000000000, 1.000000000000000000, -0.000000000000000000 ) ) ;
#32135 = CIRCLE ( 'NONE', #28191, 0.06509327318403745899 ) ;
#32134 = DIRECTION ( 'NONE',  ( 0.000000000000000000, 0.000000000000000000, 1.000000000000000000 ) ) ;
#32136 = CARTESIAN_POINT ( 'NONE',  ( 129.5000000000000000, -1.500000000000000000, 6.000000000000000000 ) ) ;
#32137 = DIRECTION ( 'NONE',  ( -0.000000000000000000, 1.000000000000000000, -0.000000000000000000 ) ) ;
#32138 = CARTESIAN_POINT ( 'NONE',  ( -9.800000000000004263, 12.50000000000000000, 3.983716857408420076 ) ) ;
#32139 = CONICAL_SURFACE ( 'NONE', #48856, 0.09999999999999982514, 0.003490658503988666988 ) ;
#32140 = CARTESIAN_POINT ( 'NONE',  ( 9.599999999999914380, 2.500000000000000000, -4.330127018922201643 ) ) ;
#32141 = AXIS2_PLACEMENT_3D ( 'NONE', #53630, #20946, #11763 ) ;
#32142 = VECTOR ( 'NONE', #48848, 1000.000000000000000 ) ;
#32143 = CARTESIAN_POINT ( 'NONE',  ( -5.400000000000020783, 2.500000000000000000, 5.022947341949748790 ) ) ;
#32144 = VERTEX_POINT ( 'NONE', #34274 ) ;
#32145 = CIRCLE ( 'NONE', #105280, 0.09999999999999982514 ) ;
#32146 = AXIS2_PLACEMENT_3D ( 'NONE', #85314, #63754, #53928 ) ;
#32147 = ORIENTED_EDGE ( 'NONE', *, *, #54304, .F. ) ;
#32148 = ORIENTED_EDGE ( 'NONE', *, *, #11583, .F. ) ;
#32149 = ORIENTED_EDGE ( 'NONE', *, *, #110141, .T. ) ;
#32150 = ORIENTED_EDGE ( 'NONE', *, *, #103710, .F. ) ;
#32151 = DIRECTION ( 'NONE',  ( -0.000000000000000000, 1.000000000000000000, -0.000000000000000000 ) ) ;
#32152 = DIRECTION ( 'NONE',  ( -0.000000000000000000, 1.000000000000000000, -0.000000000000000000 ) ) ;
#32153 = DIRECTION ( 'NONE',  ( 0.000000000000000000, 0.000000000000000000, -1.000000000000000000 ) ) ;
#32154 = CARTESIAN_POINT ( 'NONE',  ( -8.350000000000013856, 2.500000000000000000, -2.165063509461101710 ) ) ;
#32155 = LINE ( 'NONE', #49862, #40965 ) ;
#32156 = ORIENTED_EDGE ( 'NONE', *, *, #86084, .F. ) ;
#32157 = FACE_OUTER_BOUND ( 'NONE', #109105, .T. ) ;
#32159 = CIRCLE ( 'NONE', #117897, 0.09999999999999982514 ) ;
#32158 = LINE ( 'NONE', #123715, #26456 ) ;
#32160 = AXIS2_PLACEMENT_3D ( 'NONE', #45112, #15622, #53635 ) ;
#32161 = DIRECTION ( 'NONE',  ( 0.000000000000000000, 0.000000000000000000, -1.000000000000000000 ) ) ;
#32162 = DIRECTION ( 'NONE',  ( 0.000000000000000000, -0.000000000000000000, 1.000000000000000000 ) ) ;
#32163 = DIRECTION ( 'NONE',  ( -0.000000000000000000, -1.000000000000000000, -0.000000000000000000 ) ) ;
#32164 = VERTEX_POINT ( 'NONE', #52597 ) ;
#32165 = CIRCLE ( 'NONE', #90627, 0.06509327318403745899 ) ;
#32166 = VECTOR ( 'NONE', #47593, 1000.000000000000000 ) ;
#32167 = AXIS2_PLACEMENT_3D ( 'NONE', #3867, #14317, #94181 ) ;
#32168 = ORIENTED_EDGE ( 'NONE', *, *, #174, .F. ) ;
#32169 = AXIS2_PLACEMENT_3D ( 'NONE', #67147, #59323, #18724 ) ;
#32170 = VERTEX_POINT ( 'NONE', #111523 ) ;
#32172 = EDGE_CURVE ( 'NONE', #1525, #41325, #29642, .T. ) ;
#32171 = AXIS2_PLACEMENT_3D ( 'NONE', #83953, #23769, #124546 ) ;
#32173 = CARTESIAN_POINT ( 'NONE',  ( 11.64999999999990798, 12.50000000000000000, -1.472243186433550122 ) ) ;
#32174 = EDGE_CURVE ( 'NONE', #81531, #26010, #4564, .T. ) ;
#32175 = EDGE_CURVE ( 'NONE', #91490, #80874, #38058, .T. ) ;
#32176 = EDGE_LOOP ( 'NONE', ( #120091, #8624, #11970, #103363 ) ) ;
#32177 = DIRECTION ( 'NONE',  ( -0.000000000000000000, -1.000000000000000000, -0.000000000000000000 ) ) ;
#32178 = CARTESIAN_POINT ( 'NONE',  ( 8.299999999999922551, 2.500000000000000000, 4.430127018922196847 ) ) ;
#32179 = CONICAL_SURFACE ( 'NONE', #78229, 0.09999999999999982514, 0.003490658503988666988 ) ;
#32180 = AXIS2_PLACEMENT_3D ( 'NONE', #77433, #95148, #65010 ) ;
#32181 = EDGE_CURVE ( 'NONE', #91773, #119162, #112175, .T. ) ;
#32182 = VECTOR ( 'NONE', #5222, 1000.000000000000000 ) ;
#32183 = ORIENTED_EDGE ( 'NONE', *, *, #66666, .F. ) ;
#32184 = CARTESIAN_POINT ( 'NONE',  ( 11.69999999999990514, 12.50000000000000000, -2.276824562219559311E-15 ) ) ;
#32185 = CARTESIAN_POINT ( 'NONE',  ( 108.0000000000000142, 8.700999999999998735, 5.000000000000004441 ) ) ;
#32186 = CARTESIAN_POINT ( 'NONE',  ( 184.4999999999999716, -7.210521358426481342, 2.491478058008155472 ) ) ;
#32187 = LINE ( 'NONE', #10567, #99873 ) ;
#32188 = ADVANCED_FACE ( 'NONE', ( #44072 ), #127933, .T. ) ;
#32189 = EDGE_CURVE ( 'NONE', #23353, #75521, #8787, .T. ) ;
#32190 = CARTESIAN_POINT ( 'NONE',  ( 10.39999999999991154, 12.50000000000000000, -5.022947341949754119 ) ) ;
#32191 = ORIENTED_EDGE ( 'NONE', *, *, #125670, .T. ) ;
#32192 = ORIENTED_EDGE ( 'NONE', *, *, #59750, .T. ) ;
#32193 = CARTESIAN_POINT ( 'NONE',  ( -7.700000000000016165, 2.500000000000000000, -4.083716857408426826 ) ) ;
#32194 = CARTESIAN_POINT ( 'NONE',  ( -8.750000000000007105, 2.500000000000000000, 7.288010851410849256 ) ) ;
#32195 = EDGE_CURVE ( 'NONE', #93758, #100479, #98674, .T. ) ;
#32196 = CARTESIAN_POINT ( 'NONE',  ( -8.100000000000013856, 2.500000000000000000, -4.676537180435977881 ) ) ;
#32197 = AXIS2_PLACEMENT_3D ( 'NONE', #34121, #83220, #24291 ) ;
#32198 = CARTESIAN_POINT ( 'NONE',  ( 4.549999999999937650, 12.50000000000000000, 2.165063509461097713 ) ) ;
#32199 = VERTEX_POINT ( 'NONE', #83980 ) ;
#32200 = ORIENTED_EDGE ( 'NONE', *, *, #23724, .T. ) ;
#32201 = DIRECTION ( 'NONE',  ( 0.000000000000000000, -0.9999939076577903929, 0.003490651415223739937 ) ) ;
#32202 = DIRECTION ( 'NONE',  ( 0.000000000000000000, 1.000000000000000000, 0.000000000000000000 ) ) ;
#32203 = CARTESIAN_POINT ( 'NONE',  ( 6.249999999999932498, 12.50000000000000000, 5.867463478539781896 ) ) ;
#32204 = DIRECTION ( 'NONE',  ( -0.000000000000000000, -1.000000000000000000, -0.000000000000000000 ) ) ;
#32205 = ORIENTED_EDGE ( 'NONE', *, *, #102164, .F. ) ;
#32206 = CIRCLE ( 'NONE', #117941, 0.06509327318403745899 ) ;
#32207 = AXIS2_PLACEMENT_3D ( 'NONE', #64850, #45878, #87067 ) ;
#32208 = CARTESIAN_POINT ( 'NONE',  ( 5.449999999999936229, 2.500000000000000000, 6.495190528383297135 ) ) ;
#32209 = DIRECTION ( 'NONE',  ( 0.000000000000000000, 0.000000000000000000, -1.000000000000000000 ) ) ;
#32210 = ORIENTED_EDGE ( 'NONE', *, *, #116704, .F. ) ;
#32211 = CARTESIAN_POINT ( 'NONE',  ( -15.59999999999998010, 12.50000000000000000, 0.3464101615137759604 ) ) ;
#32212 = VECTOR ( 'NONE', #128144, 1000.000000000000000 ) ;
#32213 = ORIENTED_EDGE ( 'NONE', *, *, #112319, .F. ) ;
#32214 = FACE_OUTER_BOUND ( 'NONE', #69596, .T. ) ;
#32215 = AXIS2_PLACEMENT_3D ( 'NONE', #61882, #12110, #1641 ) ;
#32216 = AXIS2_PLACEMENT_3D ( 'NONE', #63873, #102507, #55342 ) ;
#32217 = ORIENTED_EDGE ( 'NONE', *, *, #28255, .F. ) ;
#32218 = CARTESIAN_POINT ( 'NONE',  ( -10.40000000000000213, 2.500000000000000000, -5.022947341949749678 ) ) ;
#32219 = PLANE ( 'NONE',  #64720 ) ;
#32220 = EDGE_LOOP ( 'NONE', ( #25564, #60565 ) ) ;
#32221 = EDGE_LOOP ( 'NONE', ( #78653, #27595 ) ) ;
#32222 = CARTESIAN_POINT ( 'NONE',  ( -1.450000000000035927, 2.500000000000000000, -1.818653347947326138 ) ) ;
#32223 = PLANE ( 'NONE',  #14220 ) ;
#32224 = DIRECTION ( 'NONE',  ( -0.000000000000000000, -1.000000000000000000, -0.000000000000000000 ) ) ;
#32225 = CARTESIAN_POINT ( 'NONE',  ( 185.1927083336747160, 6.551208109652275624, -3.782341765624998686 ) ) ;
#32226 = EDGE_CURVE ( 'NONE', #17587, #59274, #36003, .T. ) ;
#32227 = CIRCLE ( 'NONE', #88642, 0.06509327318403745899 ) ;
#32229 = AXIS2_PLACEMENT_3D ( 'NONE', #103378, #33368, #3247 ) ;
#32228 = CARTESIAN_POINT ( 'NONE',  ( -1.050000000000037792, 2.500000000000000000, 1.718653347947321386 ) ) ;
#32230 = CIRCLE ( 'NONE', #120044, 0.06509327318403745899 ) ;
#32231 = DIRECTION ( 'NONE',  ( 0.000000000000000000, 0.000000000000000000, 1.000000000000000000 ) ) ;
#32232 = LINE ( 'NONE', #1448, #40524 ) ;
#32233 = DIRECTION ( 'NONE',  ( -4.274815082592931898E-19, -0.9999939076577903929, -0.003490651415223739937 ) ) ;
#32234 = VECTOR ( 'NONE', #66335, 1000.000000000000000 ) ;
#32235 = DIRECTION ( 'NONE',  ( 0.000000000000000000, 0.000000000000000000, 1.000000000000000000 ) ) ;
#32236 = CIRCLE ( 'NONE', #99123, 0.06509327318403745899 ) ;
#32237 = VERTEX_POINT ( 'NONE', #33615 ) ;
#32238 = EDGE_LOOP ( 'NONE', ( #57949, #107064, #25887, #35666 ) ) ;
#32239 = CARTESIAN_POINT ( 'NONE',  ( 11.24999999999990763, 2.500000000000000000, 1.372243186433545370 ) ) ;
#32240 = ORIENTED_EDGE ( 'NONE', *, *, #61840, .T. ) ;
#32241 = CARTESIAN_POINT ( 'NONE',  ( 0.4499999999999569344, 2.500000000000000000, 2.065063509461097624 ) ) ;
#32242 = DIRECTION ( 'NONE',  ( -4.274815082592931898E-19, -0.9999939076577903929, -0.003490651415223739937 ) ) ;
#32243 = CARTESIAN_POINT ( 'NONE',  ( 6.649999999999928413, 2.500000000000000000, 2.857883832488649301 ) ) ;
#32245 = ORIENTED_EDGE ( 'NONE', *, *, #23518, .F. ) ;
#32244 = ORIENTED_EDGE ( 'NONE', *, *, #100437, .F. ) ;
#32246 = FACE_BOUND ( 'NONE', #129202, .T. ) ;
#32247 = EDGE_LOOP ( 'NONE', ( #62880, #57489, #112907, #72102 ) ) ;
#32248 = DIRECTION ( 'NONE',  ( 0.000000000000000000, 1.000000000000000000, 0.000000000000000000 ) ) ;
#32249 = CARTESIAN_POINT ( 'NONE',  ( 2.099999999999948574, 2.500000000000000000, 3.537306695894645081 ) ) ;
#32250 = DIRECTION ( 'NONE',  ( -0.000000000000000000, 1.000000000000000000, -0.000000000000000000 ) ) ;
#32251 = DIRECTION ( 'NONE',  ( 0.000000000000000000, 1.000000000000000000, 0.000000000000000000 ) ) ;
#32252 = CARTESIAN_POINT ( 'NONE',  ( 184.3229166673494603, -4.445597072760039126, 7.700000000000142286 ) ) ;
#32253 = DIRECTION ( 'NONE',  ( 0.000000000000000000, 0.000000000000000000, 1.000000000000000000 ) ) ;
#32254 = CIRCLE ( 'NONE', #69883, 0.1000000000000002554 ) ;
#32255 = DIRECTION ( 'NONE',  ( -0.000000000000000000, -1.000000000000000000, -0.000000000000000000 ) ) ;
#32256 = LINE ( 'NONE', #72170, #58930 ) ;
#32257 = CIRCLE ( 'NONE', #42726, 0.1000000000000000472 ) ;
#32258 = CIRCLE ( 'NONE', #124269, 0.1000000000000002554 ) ;
#32259 = DIRECTION ( 'NONE',  ( 0.000000000000000000, 1.000000000000000000, 0.000000000000000000 ) ) ;
#32260 = DIRECTION ( 'NONE',  ( -0.000000000000000000, 1.000000000000000000, -0.000000000000000000 ) ) ;
#32261 = PLANE ( 'NONE',  #66035 ) ;
#32263 = ORIENTED_EDGE ( 'NONE', *, *, #111349, .F. ) ;
#32262 = VECTOR ( 'NONE', #124050, 1000.000000000000000 ) ;
#32264 = EDGE_LOOP ( 'NONE', ( #12272, #81124 ) ) ;
#32265 = EDGE_LOOP ( 'NONE', ( #56531, #121630 ) ) ;
#32267 = CARTESIAN_POINT ( 'NONE',  ( 12.09999999999990195, 2.500000000000000000, -2.276824562219559311E-15 ) ) ;
#32266 = CONICAL_SURFACE ( 'NONE', #90732, 0.1000000000000002554, 0.003490658503988666988 ) ;
#32268 = ORIENTED_EDGE ( 'NONE', *, *, #111642, .F. ) ;
#32269 = DIRECTION ( 'NONE',  ( 0.000000000000000000, 0.000000000000000000, 1.000000000000000000 ) ) ;
#32270 = DIRECTION ( 'NONE',  ( -0.000000000000000000, -1.000000000000000000, -0.000000000000000000 ) ) ;
#32272 = ORIENTED_EDGE ( 'NONE', *, *, #44533, .F. ) ;
#32271 = EDGE_LOOP ( 'NONE', ( #41046, #17696, #88270, #18279 ) ) ;
#32273 = ORIENTED_EDGE ( 'NONE', *, *, #81346, .F. ) ;
#32274 = DIRECTION ( 'NONE',  ( 0.000000000000000000, 0.000000000000000000, 1.000000000000000000 ) ) ;
#32275 = CIRCLE ( 'NONE', #105407, 0.06509327318403745899 ) ;
#32277 = ADVANCED_FACE ( 'NONE', ( #123913 ), #96513, .T. ) ;
#32276 = AXIS2_PLACEMENT_3D ( 'NONE', #100306, #10600, #50538 ) ;
#32278 = CARTESIAN_POINT ( 'NONE',  ( -0.4000000000000396572, 2.500000000000000000, 4.330127018922196314 ) ) ;
#32279 = SHAPE_REPRESENTATION_RELATIONSHIP ( 'NONE' , 'NONE' ,  #1094, #119481 ) ;
#32280 = DIRECTION ( 'NONE',  ( 0.000000000000000000, 0.000000000000000000, 1.000000000000000000 ) ) ;
#32281 = DIRECTION ( 'NONE',  ( 0.000000000000000000, -0.9999939076577903929, 0.003490651415223739937 ) ) ;
#32282 = FACE_OUTER_BOUND ( 'NONE', #54050, .T. ) ;
#32283 = AXIS2_PLACEMENT_3D ( 'NONE', #114379, #3160, #42443 ) ;
#32284 = DIRECTION ( 'NONE',  ( 0.000000000000000000, 0.000000000000000000, 1.000000000000000000 ) ) ;
#32285 = EDGE_CURVE ( 'NONE', #37178, #88690, #21317, .T. ) ;
#32286 = ORIENTED_EDGE ( 'NONE', *, *, #14435, .F. ) ;
#32287 = EDGE_CURVE ( 'NONE', #30841, #74045, #64353, .T. ) ;
#32288 = CARTESIAN_POINT ( 'NONE',  ( 3.149999999999946176, 2.500000000000000000, -2.511473670974877948 ) ) ;
#32289 = VERTEX_POINT ( 'NONE', #91888 ) ;
#32290 = VERTEX_POINT ( 'NONE', #12024 ) ;
#32291 = ORIENTED_EDGE ( 'NONE', *, *, #84446, .F. ) ;
#32292 = EDGE_CURVE ( 'NONE', #32739, #17445, #94468, .T. ) ;
#32294 = ADVANCED_FACE ( 'NONE', ( #72261 ), #117431, .T. ) ;
#32293 = FACE_OUTER_BOUND ( 'NONE', #20036, .T. ) ;
#32296 = VERTEX_POINT ( 'NONE', #112821 ) ;
#32295 = EDGE_CURVE ( 'NONE', #6764, #88013, #102360, .T. ) ;
#32297 = EDGE_LOOP ( 'NONE', ( #93048, #125556, #106215, #85508 ) ) ;
#32298 = ADVANCED_FACE ( 'NONE', ( #102984 ), #46354, .T. ) ;
#32300 = ORIENTED_EDGE ( 'NONE', *, *, #2219, .F. ) ;
#32299 = ADVANCED_FACE ( 'NONE', ( #43450 ), #106984, .T. ) ;
#32301 = VECTOR ( 'NONE', #89019, 1000.000000000000000 ) ;
#32302 = DIRECTION ( 'NONE',  ( 0.000000000000000000, 1.000000000000000000, 0.000000000000000000 ) ) ;
#32303 = DIRECTION ( 'NONE',  ( 0.000000000000000000, 0.000000000000000000, 1.000000000000000000 ) ) ;
#32304 = CARTESIAN_POINT ( 'NONE',  ( 14.14999999999989377, 2.500000000000000000, -2.757883832488654097 ) ) ;
#32305 = LINE ( 'NONE', #82680, #8673 ) ;
#32306 = CARTESIAN_POINT ( 'NONE',  ( -4.600000000000024514, 2.500000000000000000, 3.637306695894644726 ) ) ;
#32307 = CARTESIAN_POINT ( 'NONE',  ( 12.69999999999990159, 2.500000000000000000, -3.983716857408426293 ) ) ;
#32308 = EDGE_CURVE ( 'NONE', #55936, #38064, #125863, .T. ) ;
#32309 = DIRECTION ( 'NONE',  ( 0.000000000000000000, 0.000000000000000000, 1.000000000000000000 ) ) ;
#32310 = CIRCLE ( 'NONE', #57318, 0.06509327318403741736 ) ;
#32311 = AXIS2_PLACEMENT_3D ( 'NONE', #30761, #70660, #62789 ) ;
#32312 = ORIENTED_EDGE ( 'NONE', *, *, #89307, .F. ) ;
#32313 = CARTESIAN_POINT ( 'NONE',  ( -1.850000000000033396, 2.500000000000000000, -6.741600689897077281 ) ) ;
#32314 = VERTEX_POINT ( 'NONE', #6060 ) ;
#32315 = CARTESIAN_POINT ( 'NONE',  ( 3.099999999999945022, 2.500000000000000000, -4.676537180435978769 ) ) ;
#32316 = ORIENTED_EDGE ( 'NONE', *, *, #69202, .T. ) ;
#32317 = DIRECTION ( 'NONE',  ( 0.000000000000000000, 0.000000000000000000, 1.000000000000000000 ) ) ;
#32318 = VERTEX_POINT ( 'NONE', #86564 ) ;
#32319 = DIRECTION ( 'NONE',  ( 0.000000000000000000, 0.000000000000000000, 1.000000000000000000 ) ) ;
#32320 = CIRCLE ( 'NONE', #11358, 0.1000000000000002554 ) ;
#32321 = CARTESIAN_POINT ( 'NONE',  ( 4.999999999999969802, 2.500000000000000000, 4.430127018922196847 ) ) ;
#32322 = ORIENTED_EDGE ( 'NONE', *, *, #129062, .F. ) ;
#32323 = VERTEX_POINT ( 'NONE', #46654 ) ;
#32324 = CARTESIAN_POINT ( 'NONE',  ( 2.699999999999946443, 12.50000000000000000, -3.983716857408426293 ) ) ;
#32325 = LINE ( 'NONE', #62416, #95403 ) ;
#32326 = CARTESIAN_POINT ( 'NONE',  ( 15.39999999999989200, 12.50000000000000000, 0.6277270498435120194 ) ) ;
#32327 = LINE ( 'NONE', #42796, #40941 ) ;
#32328 = FACE_OUTER_BOUND ( 'NONE', #101610, .T. ) ;
#32329 = ORIENTED_EDGE ( 'NONE', *, *, #5841, .T. ) ;
#32330 = CIRCLE ( 'NONE', #40644, 0.09999999999999982514 ) ;
#32331 = CIRCLE ( 'NONE', #84524, 0.09999999999999999167 ) ;
#32332 = DIRECTION ( 'NONE',  ( 0.000000000000000000, 0.000000000000000000, -1.000000000000000000 ) ) ;
#32333 = CIRCLE ( 'NONE', #99213, 0.09999999999999999167 ) ;
#32334 = EDGE_CURVE ( 'NONE', #47052, #17385, #111191, .T. ) ;
#32335 = EDGE_CURVE ( 'NONE', #128936, #740, #56804, .T. ) ;
#32336 = VERTEX_POINT ( 'NONE', #57768 ) ;
#32337 = AXIS2_PLACEMENT_3D ( 'NONE', #72292, #72922, #70343 ) ;
#32338 = DIRECTION ( 'NONE',  ( 0.000000000000000000, 1.000000000000000000, 0.000000000000000000 ) ) ;
#32339 = CARTESIAN_POINT ( 'NONE',  ( 9.599999999999917932, 12.50000000000000000, -0.6928203230275541413 ) ) ;
#32340 = ADVANCED_FACE ( 'NONE', ( #66916 ), #36200, .T. ) ;
#32341 = CARTESIAN_POINT ( 'NONE',  ( 186.3385416670080872, 6.551208109652274736, 3.782341765625001351 ) ) ;
#32342 = CARTESIAN_POINT ( 'NONE',  ( 9.599999999999914380, 2.500000000000000000, -3.637306695894650055 ) ) ;
#32343 = DIRECTION ( 'NONE',  ( -0.000000000000000000, 1.000000000000000000, -0.000000000000000000 ) ) ;
#32344 = EDGE_CURVE ( 'NONE', #4941, #121191, #73539, .T. ) ;
#32345 = CARTESIAN_POINT ( 'NONE',  ( -8.100000000000013856, 2.500000000000000000, -4.676537180435977881 ) ) ;
#32346 = DIRECTION ( 'NONE',  ( 0.000000000000000000, 1.000000000000000000, 0.000000000000000000 ) ) ;
#32347 = ORIENTED_EDGE ( 'NONE', *, *, #124515, .F. ) ;
#32348 = EDGE_CURVE ( 'NONE', #19669, #87504, #54760, .T. ) ;
#32349 = EDGE_CURVE ( 'NONE', #91045, #32427, #123705, .T. ) ;
#32350 = DIRECTION ( 'NONE',  ( 0.000000000000000000, 1.000000000000000000, 0.000000000000000000 ) ) ;
#32351 = EDGE_CURVE ( 'NONE', #98420, #48878, #10834, .T. ) ;
#32352 = DIRECTION ( 'NONE',  ( 0.000000000000000000, 0.000000000000000000, 1.000000000000000000 ) ) ;
#32353 = DIRECTION ( 'NONE',  ( 0.000000000000000000, -0.9999939076577903929, 0.003490651415223739937 ) ) ;
#32354 = CIRCLE ( 'NONE', #69981, 0.1000000000000002554 ) ;
#32355 = ORIENTED_EDGE ( 'NONE', *, *, #45302, .T. ) ;
#32356 = CIRCLE ( 'NONE', #40753, 0.1000000000000002554 ) ;
#32357 = AXIS2_PLACEMENT_3D ( 'NONE', #86802, #118841, #117522 ) ;
#32358 = ORIENTED_EDGE ( 'NONE', *, *, #64205, .F. ) ;
#32359 = EDGE_CURVE ( 'NONE', #70177, #12234, #90259, .T. ) ;
#32360 = CARTESIAN_POINT ( 'NONE',  ( -9.350000000000006750, 12.50000000000000000, 2.511473670974873507 ) ) ;
#32361 = AXIS2_PLACEMENT_3D ( 'NONE', #31318, #98097, #8419 ) ;
#32362 = VECTOR ( 'NONE', #108691, 1000.000000000000000 ) ;
#32363 = EDGE_LOOP ( 'NONE', ( #28364, #26872 ) ) ;
#32364 = AXIS2_PLACEMENT_3D ( 'NONE', #72368, #83479, #52079 ) ;
#32365 = ORIENTED_EDGE ( 'NONE', *, *, #19158, .F. ) ;
#32366 = FACE_OUTER_BOUND ( 'NONE', #110659, .T. ) ;
#32367 = CIRCLE ( 'NONE', #72349, 0.1000000000000000472 ) ;
#32368 = ORIENTED_EDGE ( 'NONE', *, *, #73503, .F. ) ;
#32369 = CARTESIAN_POINT ( 'NONE',  ( 16.79927703353608592, -2.472530191752320139, -3.248144252806293597 ) ) ;
#32370 = FACE_OUTER_BOUND ( 'NONE', #85186, .T. ) ;
#32371 = CARTESIAN_POINT ( 'NONE',  ( 8.349999999999923261, 2.500000000000000000, -7.188010851410854052 ) ) ;
#32372 = VERTEX_POINT ( 'NONE', #66288 ) ;
#32373 = CONICAL_SURFACE ( 'NONE', #105506, 0.09999999999999982514, 0.003490658503988666988 ) ;
#32374 = CONICAL_SURFACE ( 'NONE', #26088, 0.1000000000000000472, 0.003490658503988666988 ) ;
#32375 = CARTESIAN_POINT ( 'NONE',  ( 5.649999999999934630, 2.500000000000000000, -1.818653347947325916 ) ) ;
#32376 = DIRECTION ( 'NONE',  ( 0.000000000000000000, 0.000000000000000000, 1.000000000000000000 ) ) ;
#32377 = AXIS2_PLACEMENT_3D ( 'NONE', #18762, #91373, #50814 ) ;
#32378 = EDGE_CURVE ( 'NONE', #93110, #9428, #27567, .T. ) ;
#32379 = EDGE_LOOP ( 'NONE', ( #12427, #49517 ) ) ;
#32380 = VERTEX_POINT ( 'NONE', #34921 ) ;
#32381 = ORIENTED_EDGE ( 'NONE', *, *, #74680, .F. ) ;
#32382 = DIRECTION ( 'NONE',  ( 0.000000000000000000, 1.000000000000000000, 0.000000000000000000 ) ) ;
#32383 = DIRECTION ( 'NONE',  ( -0.000000000000000000, 1.000000000000000000, -0.000000000000000000 ) ) ;
#32384 = CARTESIAN_POINT ( 'NONE',  ( -4.150000000000027889, 2.500000000000000000, -7.188010851410854052 ) ) ;
#32385 = FACE_BOUND ( 'NONE', #94494, .T. ) ;
#32386 = ORIENTED_EDGE ( 'NONE', *, *, #83379, .F. ) ;
#32387 = DIRECTION ( 'NONE',  ( -4.274815082592931898E-19, -0.9999939076577903929, -0.003490651415223739937 ) ) ;
#32388 = DIRECTION ( 'NONE',  ( 0.000000000000000000, 1.000000000000000000, 0.000000000000000000 ) ) ;
#32389 = AXIS2_PLACEMENT_3D ( 'NONE', #1050, #41009, #109726 ) ;
#32390 = ORIENTED_EDGE ( 'NONE', *, *, #57138, .T. ) ;
#32391 = DIRECTION ( 'NONE',  ( 0.000000000000000000, 1.000000000000000000, 0.000000000000000000 ) ) ;
#32392 = DIRECTION ( 'NONE',  ( -0.000000000000000000, -1.000000000000000000, -0.000000000000000000 ) ) ;
#32393 = ADVANCED_FACE ( 'NONE', ( #105574 ), #44303, .T. ) ;
#32394 = DIRECTION ( 'NONE',  ( -4.274815082592931898E-19, -0.9999939076577903929, -0.003490651415223739937 ) ) ;
#32395 = DIRECTION ( 'NONE',  ( -0.000000000000000000, 1.000000000000000000, -0.000000000000000000 ) ) ;
#32396 = DIRECTION ( 'NONE',  ( -4.274815082592931898E-19, -0.9999939076577903929, -0.003490651415223739937 ) ) ;
#32397 = CARTESIAN_POINT ( 'NONE',  ( -6.850000000000017408, 12.50000000000000000, -6.776507416713039689 ) ) ;
#32398 = CARTESIAN_POINT ( 'NONE',  ( -4.400000000000028777, 12.50000000000000000, -4.676537180435978769 ) ) ;
#32399 = CIRCLE ( 'NONE', #49109, 0.09999999999999982514 ) ;
#32400 = ORIENTED_EDGE ( 'NONE', *, *, #125202, .F. ) ;
#32401 = VERTEX_POINT ( 'NONE', #8002 ) ;
#32402 = ORIENTED_EDGE ( 'NONE', *, *, #26123, .F. ) ;
#32403 = VERTEX_POINT ( 'NONE', #17146 ) ;
#32404 = FACE_OUTER_BOUND ( 'NONE', #10196, .T. ) ;
#32405 = CARTESIAN_POINT ( 'NONE',  ( -1.250000000000036193, 2.500000000000000000, 5.702370205355745014 ) ) ;
#32406 = LINE ( 'NONE', #43498, #105374 ) ;
#32407 = ORIENTED_EDGE ( 'NONE', *, *, #6989, .T. ) ;
#32408 = ADVANCED_FACE ( 'NONE', ( #64982 ), #81953, .T. ) ;
#32409 = FACE_BOUND ( 'NONE', #46725, .T. ) ;
#32410 = CARTESIAN_POINT ( 'NONE',  ( 1.249999999999954259, 2.500000000000000000, -7.088010851410853519 ) ) ;
#32411 = CARTESIAN_POINT ( 'NONE',  ( -15.39999999999997904, 2.500000000000000000, -0.1000000000000000056 ) ) ;
#32412 = CIRCLE ( 'NONE', #101343, 0.06509327318403745899 ) ;
#32413 = CARTESIAN_POINT ( 'NONE',  ( -11.25000000000000178, 2.500000000000000000, -1.472243186433546125 ) ) ;
#32414 = CARTESIAN_POINT ( 'NONE',  ( -13.34999999999999076, 2.500000000000000000, -2.757883832488651876 ) ) ;
#32415 = AXIS2_PLACEMENT_3D ( 'NONE', #92921, #43179, #83097 ) ;
#32416 = CARTESIAN_POINT ( 'NONE',  ( -4.400000000000025224, 2.500000000000000000, -0.4464101615137783252 ) ) ;
#32417 = LINE ( 'NONE', #23196, #28727 ) ;
#32418 = LINE ( 'NONE', #91301, #100091 ) ;
#32419 = FACE_OUTER_BOUND ( 'NONE', #117099, .T. ) ;
#32420 = CARTESIAN_POINT ( 'NONE',  ( 1.699999999999951994, 2.500000000000000000, -0.1000000000000022815 ) ) ;
#32421 = VERTEX_POINT ( 'NONE', #95753 ) ;
#32422 = AXIS2_PLACEMENT_3D ( 'NONE', #77892, #98184, #8501 ) ;
#32423 = ORIENTED_EDGE ( 'NONE', *, *, #4401, .T. ) ;
#32424 = EDGE_LOOP ( 'NONE', ( #46204, #107506, #15546, #13469 ) ) ;
#32425 = AXIS2_PLACEMENT_3D ( 'NONE', #70372, #110296, #118826 ) ;
#32426 = ORIENTED_EDGE ( 'NONE', *, *, #47669, .T. ) ;
#32427 = VERTEX_POINT ( 'NONE', #97040 ) ;
#32428 = ORIENTED_EDGE ( 'NONE', *, *, #98186, .F. ) ;
#32429 = DIRECTION ( 'NONE',  ( 0.000000000000000000, 0.000000000000000000, 1.000000000000000000 ) ) ;
#32430 = EDGE_LOOP ( 'NONE', ( #8798, #18461, #71265, #45800 ) ) ;
#32431 = ORIENTED_EDGE ( 'NONE', *, *, #81915, .F. ) ;
#32432 = CIRCLE ( 'NONE', #128575, 0.09999999999999999167 ) ;
#32433 = EDGE_CURVE ( 'NONE', #15887, #76186, #15229, .T. ) ;
#32434 = CARTESIAN_POINT ( 'NONE',  ( -3.350000000000029399, 12.50000000000000000, 6.430097255199259010 ) ) ;
#32435 = CARTESIAN_POINT ( 'NONE',  ( 15.50668943717099602, -1.500000000000000222, 6.997696160023530787 ) ) ;
#32436 = CARTESIAN_POINT ( 'NONE',  ( -10.45000000000000107, 2.500000000000000000, 2.165063509461097713 ) ) ;
#32437 = CARTESIAN_POINT ( 'NONE',  ( 7.699999999999923794, 2.500000000000000000, -0.4464101615137783252 ) ) ;
#32438 = ORIENTED_EDGE ( 'NONE', *, *, #104165, .T. ) ;
#32439 = CARTESIAN_POINT ( 'NONE',  ( -3.749999999999991118, 2.500000000000000000, 2.165063509461097713 ) ) ;
#32440 = ORIENTED_EDGE ( 'NONE', *, *, #128230, .F. ) ;
#32442 = ORIENTED_EDGE ( 'NONE', *, *, #74417, .F. ) ;
#32441 = AXIS2_PLACEMENT_3D ( 'NONE', #115826, #56260, #7147 ) ;
#32443 = FACE_OUTER_BOUND ( 'NONE', #34162, .T. ) ;
#32444 = CIRCLE ( 'NONE', #78498, 0.09999999999999982514 ) ;
#32445 = EDGE_CURVE ( 'NONE', #30581, #80023, #75688, .T. ) ;
#32447 = EDGE_CURVE ( 'NONE', #80892, #110135, #92421, .T. ) ;
#32446 = DIRECTION ( 'NONE',  ( 0.000000000000000000, 0.000000000000000000, 1.000000000000000000 ) ) ;
#32448 = EDGE_CURVE ( 'NONE', #45085, #58857, #35555, .T. ) ;
#32449 = ADVANCED_FACE ( 'NONE', ( #25714 ), #62770, .T. ) ;
#32450 = ORIENTED_EDGE ( 'NONE', *, *, #98439, .F. ) ;
#32451 = ORIENTED_EDGE ( 'NONE', *, *, #29259, .F. ) ;
#32452 = DIRECTION ( 'NONE',  ( 0.000000000000000000, 0.000000000000000000, 1.000000000000000000 ) ) ;
#32453 = AXIS2_PLACEMENT_3D ( 'NONE', #15507, #25998, #65902 ) ;
#32454 = CONICAL_SURFACE ( 'NONE', #74188, 0.09999999999999982514, 0.003490658503988666988 ) ;
#32455 = AXIS2_PLACEMENT_3D ( 'NONE', #30364, #70275, #63025 ) ;
#32456 = PLANE ( 'NONE',  #114312 ) ;
#32457 = DIRECTION ( 'NONE',  ( -4.274815082592931898E-19, -0.9999939076577903929, -0.003490651415223739937 ) ) ;
#32458 = DIRECTION ( 'NONE',  ( 0.000000000000000000, -0.000000000000000000, 1.000000000000000000 ) ) ;
#32459 = CARTESIAN_POINT ( 'NONE',  ( -2.050000000000032685, 12.50000000000000000, -6.495190528383302464 ) ) ;
#32460 = EDGE_CURVE ( 'NONE', #82094, #120092, #43990, .T. ) ;
#32461 = VERTEX_POINT ( 'NONE', #41841 ) ;
#32462 = DIRECTION ( 'NONE',  ( -0.000000000000000000, 1.000000000000000000, -0.000000000000000000 ) ) ;
#32463 = ADVANCED_FACE ( 'NONE', ( #70634 ), #77422, .T. ) ;
#32464 = CIRCLE ( 'NONE', #28322, 0.06509327318403745899 ) ;
#32465 = VECTOR ( 'NONE', #96436, 1000.000000000000000 ) ;
#32466 = EDGE_CURVE ( 'NONE', #127948, #72667, #82415, .T. ) ;
#32467 = ORIENTED_EDGE ( 'NONE', *, *, #107874, .T. ) ;
#32468 = LINE ( 'NONE', #34388, #81705 ) ;
#32469 = CARTESIAN_POINT ( 'NONE',  ( 7.099999999999927702, 12.50000000000000000, 4.957854068765711553 ) ) ;
#32470 = CARTESIAN_POINT ( 'NONE',  ( -9.150000000000009237, 12.50000000000000000, -7.188010851410848723 ) ) ;
#32471 = CIRCLE ( 'NONE', #40871, 0.06509327318403745899 ) ;
#32472 = DIRECTION ( 'NONE',  ( 0.000000000000000000, 0.000000000000000000, 1.000000000000000000 ) ) ;
#32473 = CARTESIAN_POINT ( 'NONE',  ( 179.5000000000000000, 0.6250000000000000000, -6.000000000000000000 ) ) ;
#32474 = ORIENTED_EDGE ( 'NONE', *, *, #105422, .F. ) ;
#32475 = CARTESIAN_POINT ( 'NONE',  ( 10.59999999999990905, 2.500000000000000000, 3.983716857408420076 ) ) ;
#32476 = DIRECTION ( 'NONE',  ( -4.274815082592931898E-19, -0.9999939076577903929, -0.003490651415223739937 ) ) ;
#32477 = ORIENTED_EDGE ( 'NONE', *, *, #83562, .F. ) ;
#32478 = VERTEX_POINT ( 'NONE', #62120 ) ;
#32479 = ORIENTED_EDGE ( 'NONE', *, *, #973, .F. ) ;
#32480 = FACE_OUTER_BOUND ( 'NONE', #20954, .T. ) ;
#32481 = CARTESIAN_POINT ( 'NONE',  ( -0.2000000000000408673, 2.500000000000000000, -3.983716857408426293 ) ) ;
#32482 = CARTESIAN_POINT ( 'NONE',  ( 186.4427083336747160, -6.551208109652278289, 3.782341765624995134 ) ) ;
#32483 = AXIS2_PLACEMENT_3D ( 'NONE', #40110, #158, #78761 ) ;
#32484 = CARTESIAN_POINT ( 'NONE',  ( -0.4000000000000331624, 2.500000000000000000, -0.7928203230275518987 ) ) ;
#32485 = PLANE ( 'NONE',  #31995 ) ;
#32486 = CARTESIAN_POINT ( 'NONE',  ( 17.01005371150552037, 1.931450858213933808, -5.528361852685595323 ) ) ;
#32487 = CARTESIAN_POINT ( 'NONE',  ( -12.09999999999999432, 12.50000000000000000, 3.702399969078682407 ) ) ;
#32488 = CONICAL_SURFACE ( 'NONE', #49208, 0.1000000000000000472, 0.003490658503988666988 ) ;
#32489 = CIRCLE ( 'NONE', #51356, 0.06509327318403745899 ) ;
#32490 = DIRECTION ( 'NONE',  ( -0.000000000000000000, -1.000000000000000000, -0.000000000000000000 ) ) ;
#32491 = ORIENTED_EDGE ( 'NONE', *, *, #34902, .T. ) ;
#32492 = CARTESIAN_POINT ( 'NONE',  ( -7.500000000000016875, 12.50000000000000000, -3.637306695894650055 ) ) ;
#32493 = DIRECTION ( 'NONE',  ( -0.000000000000000000, -1.000000000000000000, -0.000000000000000000 ) ) ;
#32494 = CARTESIAN_POINT ( 'NONE',  ( 11.69999999999990870, 2.500000000000000000, 4.230127018922196669 ) ) ;
#32495 = DIRECTION ( 'NONE',  ( 0.000000000000000000, 1.000000000000000000, 0.000000000000000000 ) ) ;
#32496 = ORIENTED_EDGE ( 'NONE', *, *, #1401, .F. ) ;
#32497 = CARTESIAN_POINT ( 'NONE',  ( -11.64999999999999680, 2.500000000000000000, -2.757883832488650100 ) ) ;
#32498 = AXIS2_PLACEMENT_3D ( 'NONE', #41994, #3984, #114581 ) ;
#32499 = EDGE_CURVE ( 'NONE', #50102, #11701, #102470, .T. ) ;
#32501 = EDGE_CURVE ( 'NONE', #92671, #68126, #70001, .T. ) ;
#32500 = AXIS2_PLACEMENT_3D ( 'NONE', #99360, #77131, #77756 ) ;
#32502 = CARTESIAN_POINT ( 'NONE',  ( -6.650000000000014566, 2.500000000000000000, 2.165063509461097713 ) ) ;
#32504 = EDGE_LOOP ( 'NONE', ( #78631, #91730, #59060, #68964 ) ) ;
#32503 = FACE_OUTER_BOUND ( 'NONE', #76109, .T. ) ;
#32505 = ORIENTED_EDGE ( 'NONE', *, *, #120188, .F. ) ;
#32506 = EDGE_CURVE ( 'NONE', #7114, #104821, #32023, .T. ) ;
#32507 = FACE_OUTER_BOUND ( 'NONE', #59547, .T. ) ;
#32508 = VECTOR ( 'NONE', #36260, 1000.000000000000000 ) ;
#32509 = ORIENTED_EDGE ( 'NONE', *, *, #115026, .T. ) ;
#32510 = EDGE_LOOP ( 'NONE', ( #21968, #119216, #24277, #32150 ) ) ;
#32511 = DIRECTION ( 'NONE',  ( -0.000000000000000000, -1.000000000000000000, -0.000000000000000000 ) ) ;
#32512 = CARTESIAN_POINT ( 'NONE',  ( 19.72570408286475185, 0.6078483229322081405, -4.299616118078707139 ) ) ;
#32513 = DIRECTION ( 'NONE',  ( -0.000000000000000000, 1.000000000000000000, -0.000000000000000000 ) ) ;
#32514 = DIRECTION ( 'NONE',  ( -0.000000000000000000, 1.000000000000000000, -0.000000000000000000 ) ) ;
#32515 = VERTEX_POINT ( 'NONE', #22851 ) ;
#32516 = CONICAL_SURFACE ( 'NONE', #93146, 0.1000000000000002554, 0.003490658503988666988 ) ;
#32517 = PLANE ( 'NONE',  #73391 ) ;
#32518 = ORIENTED_EDGE ( 'NONE', *, *, #1132, .F. ) ;
#32519 = DIRECTION ( 'NONE',  ( -0.000000000000000000, 1.000000000000000000, -0.000000000000000000 ) ) ;
#32520 = DIRECTION ( 'NONE',  ( 0.000000000000000000, 0.000000000000000000, 1.000000000000000000 ) ) ;
#32521 = AXIS2_PLACEMENT_3D ( 'NONE', #7783, #77179, #108571 ) ;
#32522 = EDGE_LOOP ( 'NONE', ( #95671, #104051, #96966, #88777 ) ) ;
#32523 = VECTOR ( 'NONE', #3791, 1000.000000000000000 ) ;
#32524 = ORIENTED_EDGE ( 'NONE', *, *, #36285, .F. ) ;
#32525 = AXIS2_PLACEMENT_3D ( 'NONE', #36820, #16501, #95087 ) ;
#32526 = VERTEX_POINT ( 'NONE', #71942 ) ;
#32527 = EDGE_LOOP ( 'NONE', ( #88218, #104356 ) ) ;
#32528 = CARTESIAN_POINT ( 'NONE',  ( -0.4500000000000397571, 12.50000000000000000, -2.165063509461101710 ) ) ;
#32529 = FACE_OUTER_BOUND ( 'NONE', #78473, .T. ) ;
#32530 = CARTESIAN_POINT ( 'NONE',  ( 1.249999999999986899, 12.50000000000000000, 6.495190528383297135 ) ) ;
#32531 = FACE_BOUND ( 'NONE', #114633, .T. ) ;
#32532 = VERTEX_POINT ( 'NONE', #127783 ) ;
#32533 = CARTESIAN_POINT ( 'NONE',  ( 185.4895833340161175, -4.445597072760115509, -7.700000000000001954 ) ) ;
#32534 = CARTESIAN_POINT ( 'NONE',  ( 13.94999999999989804, 12.50000000000000000, 1.883746621131358934 ) ) ;
#32535 = DIRECTION ( 'NONE',  ( 0.000000000000000000, 0.000000000000000000, 1.000000000000000000 ) ) ;
#32536 = AXIS2_PLACEMENT_3D ( 'NONE', #104859, #15182, #55137 ) ;
#32537 = VECTOR ( 'NONE', #60473, 1000.000000000000000 ) ;
#32538 = ADVANCED_FACE ( 'NONE', ( #62763 ), #12353, .T. ) ;
#32539 = CARTESIAN_POINT ( 'NONE',  ( -3.749999999999991562, 12.50000000000000000, 6.430097255199259010 ) ) ;
#32540 = CONICAL_SURFACE ( 'NONE', #105681, 0.09999999999999982514, 0.003490658503988666988 ) ;
#32541 = DIRECTION ( 'NONE',  ( 0.000000000000000000, 0.000000000000000000, 1.000000000000000000 ) ) ;
#32542 = DIRECTION ( 'NONE',  ( -0.000000000000000000, -1.000000000000000000, -0.000000000000000000 ) ) ;
#32543 = CONICAL_SURFACE ( 'NONE', #82713, 0.1000000000000002554, 0.003490658503988666988 ) ;
#32544 = AXIS2_PLACEMENT_3D ( 'NONE', #10009, #118021, #39498 ) ;
#32545 = DIRECTION ( 'NONE',  ( -0.000000000000000000, 1.000000000000000000, -0.000000000000000000 ) ) ;
#32546 = CIRCLE ( 'NONE', #20098, 0.06509327318403743123 ) ;
#32547 = ORIENTED_EDGE ( 'NONE', *, *, #47179, .F. ) ;
#32548 = VERTEX_POINT ( 'NONE', #92200 ) ;
#32549 = ORIENTED_EDGE ( 'NONE', *, *, #97306, .F. ) ;
#32550 = VERTEX_POINT ( 'NONE', #32678 ) ;
#32551 = AXIS2_PLACEMENT_3D ( 'NONE', #71395, #51147, #121792 ) ;
#32553 = ORIENTED_EDGE ( 'NONE', *, *, #56764, .F. ) ;
#32552 = EDGE_CURVE ( 'NONE', #19348, #84309, #96191, .T. ) ;
#32554 = CARTESIAN_POINT ( 'NONE',  ( 7.049999999999928768, 12.50000000000000000, -2.165063509461101710 ) ) ;
#32555 = DIRECTION ( 'NONE',  ( 0.000000000000000000, -0.9999939076577903929, 0.003490651415223739937 ) ) ;
#32556 = VERTEX_POINT ( 'NONE', #51016 ) ;
#32557 = EDGE_CURVE ( 'NONE', #97573, #81547, #31371, .T. ) ;
#32558 = FACE_BOUND ( 'NONE', #103368, .T. ) ;
#32559 = CARTESIAN_POINT ( 'NONE',  ( -12.29999999999999716, 12.50000000000000000, -3.983716857408423628 ) ) ;
#32560 = ORIENTED_EDGE ( 'NONE', *, *, #1089, .F. ) ;
#32561 = DIRECTION ( 'NONE',  ( 0.000000000000000000, 1.000000000000000000, 0.000000000000000000 ) ) ;
#32562 = ADVANCED_FACE ( 'NONE', ( #41201 ), #110557, .T. ) ;
#32563 = DIRECTION ( 'NONE',  ( 0.000000000000000000, -0.000000000000000000, 1.000000000000000000 ) ) ;
#32564 = DIRECTION ( 'NONE',  ( -0.000000000000000000, -1.000000000000000000, -0.000000000000000000 ) ) ;
#32566 = ORIENTED_EDGE ( 'NONE', *, *, #118111, .F. ) ;
#32565 = AXIS2_PLACEMENT_3D ( 'NONE', #107395, #77290, #47848 ) ;
#32567 = DIRECTION ( 'NONE',  ( -4.274815082592931898E-19, -0.9999939076577903929, -0.003490651415223739937 ) ) ;
#32568 = ORIENTED_EDGE ( 'NONE', *, *, #101453, .T. ) ;
#32569 = ORIENTED_EDGE ( 'NONE', *, *, #67280, .T. ) ;
#32570 = ORIENTED_EDGE ( 'NONE', *, *, #37525, .F. ) ;
#32571 = DIRECTION ( 'NONE',  ( -0.000000000000000000, 1.000000000000000000, -0.000000000000000000 ) ) ;
#32572 = CARTESIAN_POINT ( 'NONE',  ( -7.499999999999980460, 12.50000000000000000, -4.330127018922201643 ) ) ;
#32573 = CIRCLE ( 'NONE', #111980, 0.06509327318403743123 ) ;
#32574 = DIRECTION ( 'NONE',  ( 0.000000000000000000, 1.000000000000000000, 0.000000000000000000 ) ) ;
#32575 = ORIENTED_EDGE ( 'NONE', *, *, #106734, .T. ) ;
#32576 = DIRECTION ( 'NONE',  ( -4.274815082592931898E-19, -0.9999939076577903929, -0.003490651415223739937 ) ) ;
#32577 = AXIS2_PLACEMENT_3D ( 'NONE', #33653, #103025, #23174 ) ;
#32578 = VECTOR ( 'NONE', #966, 1000.000000000000000 ) ;
#32579 = DIRECTION ( 'NONE',  ( 0.000000000000000000, 0.000000000000000000, 1.000000000000000000 ) ) ;
#32580 = CIRCLE ( 'NONE', #28643, 0.1000000000000000472 ) ;
#32582 = EDGE_CURVE ( 'NONE', #114322, #10341, #110860, .T. ) ;
#32581 = CARTESIAN_POINT ( 'NONE',  ( 12.89999999999990088, 12.50000000000000000, -4.330127018922201643 ) ) ;
#32583 = DIRECTION ( 'NONE',  ( -0.000000000000000000, 1.000000000000000000, -0.000000000000000000 ) ) ;
#32584 = CARTESIAN_POINT ( 'NONE',  ( -4.150000000000025224, 12.50000000000000000, 6.495190528383297135 ) ) ;
#32585 = ORIENTED_EDGE ( 'NONE', *, *, #1089, .T. ) ;
#32586 = DIRECTION ( 'NONE',  ( 0.000000000000000000, -0.9999939076577903929, 0.003490651415223739937 ) ) ;
#32587 = ORIENTED_EDGE ( 'NONE', *, *, #63171, .F. ) ;
#32588 = DIRECTION ( 'NONE',  ( 0.000000000000000000, 1.000000000000000000, 0.000000000000000000 ) ) ;
#32589 = CONICAL_SURFACE ( 'NONE', #66006, 0.09999999999999982514, 0.003490658503988666988 ) ;
#32590 = EDGE_CURVE ( 'NONE', #22957, #59076, #112933, .T. ) ;
#32591 = ORIENTED_EDGE ( 'NONE', *, *, #87078, .F. ) ;
#32593 = AXIS2_PLACEMENT_3D ( 'NONE', #33822, #85505, #125432 ) ;
#32592 = VECTOR ( 'NONE', #1327, 1000.000000000000000 ) ;
#32594 = ORIENTED_EDGE ( 'NONE', *, *, #827, .T. ) ;
#32595 = CARTESIAN_POINT ( 'NONE',  ( -3.150000000000029221, 12.50000000000000000, -1.883746621131363597 ) ) ;
#32596 = DIRECTION ( 'NONE',  ( 0.000000000000000000, 0.000000000000000000, -1.000000000000000000 ) ) ;
#32597 = EDGE_CURVE ( 'NONE', #61381, #40379, #111187, .T. ) ;
#32598 = PLANE ( 'NONE',  #15267 ) ;
#32600 = EDGE_CURVE ( 'NONE', #19176, #75526, #51659, .T. ) ;
#32599 = DIRECTION ( 'NONE',  ( 0.000000000000000000, 1.000000000000000000, 0.000000000000000000 ) ) ;
#32601 = EDGE_CURVE ( 'NONE', #115027, #109720, #60711, .T. ) ;
#32602 = CARTESIAN_POINT ( 'NONE',  ( 6.899999999999926636, 12.50000000000000000, 0.3464101615137736845 ) ) ;
#32603 = EDGE_CURVE ( 'NONE', #37202, #4262, #592, .T. ) ;
#32604 = ORIENTED_EDGE ( 'NONE', *, *, #495, .F. ) ;
#32605 = ORIENTED_EDGE ( 'NONE', *, *, #4064, .F. ) ;
#32606 = DIRECTION ( 'NONE',  ( -0.000000000000000000, 1.000000000000000000, -0.000000000000000000 ) ) ;
#32607 = CIRCLE ( 'NONE', #15838, 0.09999999999999999167 ) ;
#32608 = CIRCLE ( 'NONE', #118252, 0.06509327318403745899 ) ;
#32609 = CARTESIAN_POINT ( 'NONE',  ( 14.54999999999989235, 2.500000000000000000, -2.165063509461101710 ) ) ;
#32610 = ADVANCED_FACE ( 'NONE', ( #33312 ), #123390, .T. ) ;
#32611 = DIRECTION ( 'NONE',  ( -0.000000000000000000, -1.000000000000000000, -0.000000000000000000 ) ) ;
#32612 = ORIENTED_EDGE ( 'NONE', *, *, #77399, .F. ) ;
#32613 = VERTEX_POINT ( 'NONE', #83050 ) ;
#32614 = ADVANCED_FACE ( 'NONE', ( #53587 ), #5738, .T. ) ;
#32615 = PLANE ( 'NONE',  #20626 ) ;
#32616 = ORIENTED_EDGE ( 'NONE', *, *, #105912, .F. ) ;
#32617 = DIRECTION ( 'NONE',  ( 0.000000000000000000, 0.000000000000000000, -1.000000000000000000 ) ) ;
#32618 = DIRECTION ( 'NONE',  ( -0.000000000000000000, 1.000000000000000000, -0.000000000000000000 ) ) ;
#32619 = EDGE_CURVE ( 'NONE', #107723, #67419, #29316, .T. ) ;
#32620 = EDGE_CURVE ( 'NONE', #70966, #119822, #74505, .T. ) ;
#32621 = DIRECTION ( 'NONE',  ( 0.000000000000000000, 0.000000000000000000, 1.000000000000000000 ) ) ;
#32622 = ORIENTED_EDGE ( 'NONE', *, *, #124056, .T. ) ;
#32623 = DIRECTION ( 'NONE',  ( -0.000000000000000000, 1.000000000000000000, -0.000000000000000000 ) ) ;
#32624 = CARTESIAN_POINT ( 'NONE',  ( 6.249999999999968914, 2.500000000000000000, -6.495190528383302464 ) ) ;
#32625 = DIRECTION ( 'NONE',  ( 0.000000000000000000, 0.000000000000000000, 1.000000000000000000 ) ) ;
#32626 = DIRECTION ( 'NONE',  ( 0.000000000000000000, 0.000000000000000000, 1.000000000000000000 ) ) ;
#32628 = ADVANCED_FACE ( 'NONE', ( #115050 ), #6294, .T. ) ;
#32627 = DIRECTION ( 'NONE',  ( 0.000000000000000000, 1.000000000000000000, 0.000000000000000000 ) ) ;
#32629 = ORIENTED_EDGE ( 'NONE', *, *, #17755, .T. ) ;
#32630 = DIRECTION ( 'NONE',  ( 0.000000000000000000, 0.000000000000000000, 1.000000000000000000 ) ) ;
#32631 = AXIS2_PLACEMENT_3D ( 'NONE', #112236, #102417, #123971 ) ;
#32632 = VECTOR ( 'NONE', #112000, 1000.000000000000000 ) ;
#32633 = DIRECTION ( 'NONE',  ( 0.000000000000000000, -0.000000000000000000, 1.000000000000000000 ) ) ;
#32634 = ORIENTED_EDGE ( 'NONE', *, *, #1655, .T. ) ;
#32635 =( BOUNDED_CURVE ( )  B_SPLINE_CURVE ( 2, ( #19371, #80254, #69778, #70426, #50155, #99255, #101177 ),
 .UNSPECIFIED., .F., .F. ) 
 B_SPLINE_CURVE_WITH_KNOTS ( ( 3, 2, 2, 3 ),
 ( 0.2857142857142859760, 0.3095238095238098119, 0.3333333333333335924, 0.3571428571428574283 ),
 .UNSPECIFIED. ) 
 CURVE ( )  GEOMETRIC_REPRESENTATION_ITEM ( )  RATIONAL_B_SPLINE_CURVE ( ( 0.9999999999999984457, 0.8660254037844402619, 1.000000000000000000, 0.8660254037844387076, 1.000000000000000000, 0.8660254037844371533, 1.000000000000001554 ) ) 
 REPRESENTATION_ITEM ( '' )  );
#32636 = ORIENTED_EDGE ( 'NONE', *, *, #79007, .T. ) ;
#32637 = CARTESIAN_POINT ( 'NONE',  ( 183.9843750003414016, -8.734944146203032389, -1.604583208406768146E-15 ) ) ;
#32638 = LINE ( 'NONE', #72540, #44873 ) ;
#32639 = DIRECTION ( 'NONE',  ( 0.000000000000000000, 0.000000000000000000, -1.000000000000000000 ) ) ;
#32640 = DIRECTION ( 'NONE',  ( 0.000000000000000000, 0.000000000000000000, 1.000000000000000000 ) ) ;
#32641 = DIRECTION ( 'NONE',  ( -0.000000000000000000, 1.000000000000000000, -0.000000000000000000 ) ) ;
#32642 = DIRECTION ( 'NONE',  ( 0.000000000000000000, 1.000000000000000000, 0.000000000000000000 ) ) ;
#32643 = FACE_OUTER_BOUND ( 'NONE', #9997, .T. ) ;
#32644 = DIRECTION ( 'NONE',  ( -0.000000000000000000, -1.000000000000000000, -0.000000000000000000 ) ) ;
#32645 = DIRECTION ( 'NONE',  ( -0.000000000000000000, -1.000000000000000000, -0.000000000000000000 ) ) ;
#32646 = CONICAL_SURFACE ( 'NONE', #122416, 0.1000000000000002554, 0.003490658503988666988 ) ;
#32647 = VERTEX_POINT ( 'NONE', #75780 ) ;
#32648 = ORIENTED_EDGE ( 'NONE', *, *, #58897, .F. ) ;
#32649 = AXIS2_PLACEMENT_3D ( 'NONE', #109362, #19704, #51109 ) ;
#32650 = ORIENTED_EDGE ( 'NONE', *, *, #29137, .F. ) ;
#32651 = VECTOR ( 'NONE', #60174, 1000.000000000000000 ) ;
#32652 = EDGE_LOOP ( 'NONE', ( #12928, #101811, #92519, #48184 ) ) ;
#32653 = CARTESIAN_POINT ( 'NONE',  ( 8.349999999999923261, 2.500000000000000000, 2.857883832488649301 ) ) ;
#32654 = DIRECTION ( 'NONE',  ( -0.000000000000000000, 1.000000000000000000, -0.000000000000000000 ) ) ;
#32655 = ORIENTED_EDGE ( 'NONE', *, *, #7166, .F. ) ;
#32656 = CARTESIAN_POINT ( 'NONE',  ( 7.899999999999924860, 2.500000000000000000, -4.230127018922201998 ) ) ;
#32657 = ADVANCED_FACE ( 'NONE', ( #13637 ), #89939, .T. ) ;
#32658 = EDGE_CURVE ( 'NONE', #87021, #128668, #54846, .T. ) ;
#32659 = DIRECTION ( 'NONE',  ( 0.000000000000000000, 1.000000000000000000, 0.000000000000000000 ) ) ;
#32661 = ORIENTED_EDGE ( 'NONE', *, *, #32359, .T. ) ;
#32660 = DIRECTION ( 'NONE',  ( -4.274815082592931898E-19, -0.9999939076577903929, -0.003490651415223739937 ) ) ;
#32662 = DIRECTION ( 'NONE',  ( 0.000000000000000000, -0.9999939076577903929, 0.003490651415223739937 ) ) ;
#32663 = CIRCLE ( 'NONE', #59939, 0.06509327318403745899 ) ;
#32664 = CARTESIAN_POINT ( 'NONE',  ( 187.5000000000000000, 0.000000000000000000, 0.000000000000000000 ) ) ;
#32665 = VERTEX_POINT ( 'NONE', #122965 ) ;
#32666 = EDGE_LOOP ( 'NONE', ( #14152, #84076 ) ) ;
#32667 = ORIENTED_EDGE ( 'NONE', *, *, #47230, .F. ) ;
#32668 = ORIENTED_EDGE ( 'NONE', *, *, #31858, .F. ) ;
#32669 = DIRECTION ( 'NONE',  ( -0.000000000000000000, 1.000000000000000000, -0.000000000000000000 ) ) ;
#32670 = CIRCLE ( 'NONE', #101694, 0.06509327318403745899 ) ;
#32671 = AXIS2_PLACEMENT_3D ( 'NONE', #25758, #17191, #75491 ) ;
#32672 = CARTESIAN_POINT ( 'NONE',  ( 6.649999999999930189, 2.500000000000000000, 7.088010851410848190 ) ) ;
#32673 = LINE ( 'NONE', #100723, #42024 ) ;
#32674 = AXIS2_PLACEMENT_3D ( 'NONE', #63607, #104169, #74707 ) ;
#32675 = CARTESIAN_POINT ( 'NONE',  ( 12.69999999999990159, 2.500000000000000000, 4.576537180435972019 ) ) ;
#32676 = ORIENTED_EDGE ( 'NONE', *, *, #76052, .F. ) ;
#32677 = CONICAL_SURFACE ( 'NONE', #66087, 0.1000000000000002554, 0.003490658503988666988 ) ;
#32678 = CARTESIAN_POINT ( 'NONE',  ( -10.65000000000000391, 2.500000000000000000, -2.411473670974874306 ) ) ;
#32679 = ORIENTED_EDGE ( 'NONE', *, *, #98084, .T. ) ;
#32680 = CARTESIAN_POINT ( 'NONE',  ( 87.50000000000001421, 0.000000000000000000, 0.000000000000000000 ) ) ;
#32681 = CARTESIAN_POINT ( 'NONE',  ( 2.500000000000002220, -1.499999999999999556, -9.999999999999998224 ) ) ;
#32682 = LINE ( 'NONE', #62767, #6612 ) ;
#32683 = DIRECTION ( 'NONE',  ( 0.000000000000000000, 1.000000000000000000, 0.000000000000000000 ) ) ;
#32684 = CONICAL_SURFACE ( 'NONE', #61916, 0.09999999999999982514, 0.003490658503988666988 ) ;
#32685 = ORIENTED_EDGE ( 'NONE', *, *, #104918, .F. ) ;
#32687 = VECTOR ( 'NONE', #52502, 1000.000000000000000 ) ;
#32686 = AXIS2_PLACEMENT_3D ( 'NONE', #33242, #82977, #92124 ) ;
#32688 = EDGE_LOOP ( 'NONE', ( #73037, #35076 ) ) ;
#32689 = ORIENTED_EDGE ( 'NONE', *, *, #10125, .T. ) ;
#32690 = DIRECTION ( 'NONE',  ( 0.000000000000000000, -0.9999939076577903929, 0.003490651415223739937 ) ) ;
#32691 = CARTESIAN_POINT ( 'NONE',  ( -12.04999999999999716, 12.50000000000000000, -2.099970236277060476 ) ) ;
#32692 = CARTESIAN_POINT ( 'NONE',  ( -6.050000000000017586, 2.500000000000000000, 6.148780366869520009 ) ) ;
#32693 = FACE_BOUND ( 'NONE', #88814, .T. ) ;
#32694 = LINE ( 'NONE', #91584, #122546 ) ;
#32695 = PLANE ( 'NONE',  #119748 ) ;
#32696 = DIRECTION ( 'NONE',  ( 0.000000000000000000, 0.000000000000000000, -1.000000000000000000 ) ) ;
#32697 = ADVANCED_FACE ( 'NONE', ( #124255 ), #94140, .T. ) ;
#32698 = DIRECTION ( 'NONE',  ( 0.000000000000000000, 0.000000000000000000, 1.000000000000000000 ) ) ;
#32699 = FACE_OUTER_BOUND ( 'NONE', #21877, .T. ) ;
#32700 = CARTESIAN_POINT ( 'NONE',  ( 12.09999999999990195, 2.500000000000000000, -0.5928203230275541635 ) ) ;
#32701 = ORIENTED_EDGE ( 'NONE', *, *, #84164, .T. ) ;
#32702 = DIRECTION ( 'NONE',  ( -0.000000000000000000, -1.000000000000000000, -0.000000000000000000 ) ) ;
#32703 = ORIENTED_EDGE ( 'NONE', *, *, #10091, .F. ) ;
#32704 = ORIENTED_EDGE ( 'NONE', *, *, #88023, .F. ) ;
#32705 = ADVANCED_FACE ( 'NONE', ( #114418 ), #87865, .T. ) ;
#32706 = DIRECTION ( 'NONE',  ( -0.000000000000000000, 1.000000000000000000, -0.000000000000000000 ) ) ;
#32708 = EDGE_CURVE ( 'NONE', #102277, #124065, #23467, .T. ) ;
#32707 = CARTESIAN_POINT ( 'NONE',  ( 5.599999999999934808, 2.500000000000000000, -3.983716857408426293 ) ) ;
#32709 = FACE_BOUND ( 'NONE', #47079, .T. ) ;
#32710 = DIRECTION ( 'NONE',  ( -4.274815082592931898E-19, -0.9999939076577903929, -0.003490651415223739937 ) ) ;
#32711 = CIRCLE ( 'NONE', #128858, 0.06509327318403745899 ) ;
#32712 = CIRCLE ( 'NONE', #97519, 0.1000000000000002554 ) ;
#32713 = ORIENTED_EDGE ( 'NONE', *, *, #47230, .T. ) ;
#32714 = DIRECTION ( 'NONE',  ( 0.000000000000000000, 1.000000000000000000, 0.000000000000000000 ) ) ;
#32715 = ADVANCED_FACE ( 'NONE', ( #64677 ), #98254, .T. ) ;
#32716 = CARTESIAN_POINT ( 'NONE',  ( 9.349999999999916156, 12.50000000000000000, -1.818653347947326138 ) ) ;
#32717 = EDGE_LOOP ( 'NONE', ( #61318, #8519 ) ) ;
#32718 = FACE_OUTER_BOUND ( 'NONE', #47220, .T. ) ;
#32719 = DIRECTION ( 'NONE',  ( -0.000000000000000000, 1.000000000000000000, -0.000000000000000000 ) ) ;
#32721 = AXIS2_PLACEMENT_3D ( 'NONE', #20126, #70504, #110429 ) ;
#32720 = AXIS2_PLACEMENT_3D ( 'NONE', #4587, #94954, #114566 ) ;
#32722 = ORIENTED_EDGE ( 'NONE', *, *, #86460, .T. ) ;
#32723 = DIRECTION ( 'NONE',  ( 0.000000000000000000, 0.000000000000000000, 1.000000000000000000 ) ) ;
#32724 = DIRECTION ( 'NONE',  ( 0.000000000000000000, 1.000000000000000000, 0.000000000000000000 ) ) ;
#32726 = CONICAL_SURFACE ( 'NONE', #41044, 0.1000000000000000472, 0.003490658503988666988 ) ;
#32725 = CIRCLE ( 'NONE', #114186, 7.700000000000000178 ) ;
#32727 = ORIENTED_EDGE ( 'NONE', *, *, #44494, .F. ) ;
#32728 = VECTOR ( 'NONE', #94232, 1000.000000000000000 ) ;
#32729 = DIRECTION ( 'NONE',  ( 0.000000000000000000, 1.000000000000000000, 0.000000000000000000 ) ) ;
#32730 = DIRECTION ( 'NONE',  ( 0.000000000000000000, 0.000000000000000000, -1.000000000000000000 ) ) ;
#32731 = DIRECTION ( 'NONE',  ( -0.000000000000000000, 1.000000000000000000, -0.000000000000000000 ) ) ;
#32732 = ORIENTED_EDGE ( 'NONE', *, *, #96914, .F. ) ;
#32733 = ORIENTED_EDGE ( 'NONE', *, *, #43960, .T. ) ;
#32734 = DIRECTION ( 'NONE',  ( 0.000000000000000000, 0.000000000000000000, 1.000000000000000000 ) ) ;
#32735 = ORIENTED_EDGE ( 'NONE', *, *, #34224, .T. ) ;
#32736 = DIRECTION ( 'NONE',  ( -0.000000000000000000, -1.000000000000000000, -0.000000000000000000 ) ) ;
#32737 = DIRECTION ( 'NONE',  ( -0.000000000000000000, -1.000000000000000000, -0.000000000000000000 ) ) ;
#32738 = EDGE_CURVE ( 'NONE', #87143, #28223, #25384, .T. ) ;
#32739 = VERTEX_POINT ( 'NONE', #103327 ) ;
#32740 = DIRECTION ( 'NONE',  ( 0.000000000000000000, 0.000000000000000000, -1.000000000000000000 ) ) ;
#32741 = DIRECTION ( 'NONE',  ( 0.000000000000000000, 1.000000000000000000, 0.000000000000000000 ) ) ;
#32742 = DIRECTION ( 'NONE',  ( 0.000000000000000000, 0.000000000000000000, -1.000000000000000000 ) ) ;
#32743 = PLANE ( 'NONE',  #40256 ) ;
#32744 = EDGE_CURVE ( 'NONE', #48591, #24755, #71161, .T. ) ;
#32745 = CIRCLE ( 'NONE', #128898, 0.09999999999999982514 ) ;
#32746 = DIRECTION ( 'NONE',  ( 0.000000000000000000, 1.000000000000000000, 0.000000000000000000 ) ) ;
#32747 = EDGE_CURVE ( 'NONE', #76320, #115380, #15568, .T. ) ;
#32748 = EDGE_LOOP ( 'NONE', ( #85854, #99184 ) ) ;
#32749 = ORIENTED_EDGE ( 'NONE', *, *, #122118, .F. ) ;
#32750 = CARTESIAN_POINT ( 'NONE',  ( -8.550000000000013145, 2.500000000000000000, -6.941600689897073906 ) ) ;
#32751 = EDGE_LOOP ( 'NONE', ( #116325, #7610, #63660, #38853 ) ) ;
#32752 = CIRCLE ( 'NONE', #34802, 0.09999999999999999167 ) ;
#32753 = LINE ( 'NONE', #72664, #114126 ) ;
#32754 = EDGE_CURVE ( 'NONE', #71951, #72177, #114970, .T. ) ;
#32756 = EDGE_LOOP ( 'NONE', ( #28550, #27604, #6780, #1714 ) ) ;
#32755 = EDGE_LOOP ( 'NONE', ( #110745, #52434 ) ) ;
#32757 = EDGE_CURVE ( 'NONE', #29668, #34370, #104516, .T. ) ;
#32758 = AXIS2_PLACEMENT_3D ( 'NONE', #80382, #51566, #109831 ) ;
#32759 = EDGE_LOOP ( 'NONE', ( #58107, #12343 ) ) ;
#32760 = ADVANCED_FACE ( 'NONE', ( #12981 ), #92870, .T. ) ;
#32761 = FACE_OUTER_BOUND ( 'NONE', #69829, .T. ) ;
#32762 = AXIS2_PLACEMENT_3D ( 'NONE', #104787, #68584, #106101 ) ;
#32763 = CIRCLE ( 'NONE', #112258, 0.1000000000000002554 ) ;
#32764 = CARTESIAN_POINT ( 'NONE',  ( -8.750000000000010658, 2.500000000000000000, -7.188010851410848723 ) ) ;
#32765 = CARTESIAN_POINT ( 'NONE',  ( 6.849999999999927702, 12.50000000000000000, 2.511473670974873507 ) ) ;
#32766 = AXIS2_PLACEMENT_3D ( 'NONE', #27010, #97030, #98306 ) ;
#32767 = FILL_AREA_STYLE ('',( #71356 ) ) ;
#32768 = EDGE_CURVE ( 'NONE', #37336, #93396, #75270, .T. ) ;
#32769 = CARTESIAN_POINT ( 'NONE',  ( -3.350000000000028511, 12.50000000000000000, 2.857883832488649301 ) ) ;
#32770 = CARTESIAN_POINT ( 'NONE',  ( 184.9479166673494603, -6.668395609140176816, -3.850000000000003642 ) ) ;
#32771 = DIRECTION ( 'NONE',  ( -0.000000000000000000, -0.000000000000000000, -1.000000000000000000 ) ) ;
#32772 = CARTESIAN_POINT ( 'NONE',  ( 4.999999999999935163, 12.50000000000000000, 3.572213422710607489 ) ) ;
#32773 = DIRECTION ( 'NONE',  ( 0.000000000000000000, 0.000000000000000000, -1.000000000000000000 ) ) ;
#32775 = EDGE_CURVE ( 'NONE', #79205, #100057, #92004, .T. ) ;
#32774 = CARTESIAN_POINT ( 'NONE',  ( -2.950000000000029932, 12.50000000000000000, 2.230156782645134950 ) ) ;
#32776 = AXIS2_PLACEMENT_3D ( 'NONE', #121511, #44092, #125238 ) ;
#32777 = VERTEX_POINT ( 'NONE', #7677 ) ;
#32779 = CIRCLE ( 'NONE', #74517, 0.1000000000000002554 ) ;
#32778 = VECTOR ( 'NONE', #109185, 1000.000000000000000 ) ;
#32780 = CARTESIAN_POINT ( 'NONE',  ( 0.3999999999999568345, 2.500000000000000000, -3.637306695894650055 ) ) ;
#32781 = ORIENTED_EDGE ( 'NONE', *, *, #66742, .F. ) ;
#32782 = ORIENTED_EDGE ( 'NONE', *, *, #98613, .F. ) ;
#32783 = DIRECTION ( 'NONE',  ( -0.000000000000000000, 1.000000000000000000, -0.000000000000000000 ) ) ;
#32784 = PLANE ( 'NONE',  #51851 ) ;
#32785 = CARTESIAN_POINT ( 'NONE',  ( 10.79999999999991367, 2.500000000000000000, -2.385244779468109755E-15 ) ) ;
#32786 = CARTESIAN_POINT ( 'NONE',  ( 8.349999999999919709, 2.500000000000000000, 6.395190528383296602 ) ) ;
#32787 = FACE_OUTER_BOUND ( 'NONE', #13857, .T. ) ;
#32788 = DIRECTION ( 'NONE',  ( 0.000000000000000000, 0.000000000000000000, 1.000000000000000000 ) ) ;
#32789 = CARTESIAN_POINT ( 'NONE',  ( 9.799999999999915445, 2.500000000000000000, 3.883716857408421319 ) ) ;
#32790 = VERTEX_POINT ( 'NONE', #87533 ) ;
#32791 = VERTEX_POINT ( 'NONE', #16202 ) ;
#32792 = VERTEX_POINT ( 'NONE', #57445 ) ;
#32793 = VERTEX_POINT ( 'NONE', #96703 ) ;
#32794 = ORIENTED_EDGE ( 'NONE', *, *, #2862, .F. ) ;
#32795 = DIRECTION ( 'NONE',  ( 0.000000000000000000, 1.000000000000000000, 0.000000000000000000 ) ) ;
#32796 = CARTESIAN_POINT ( 'NONE',  ( 187.2500000000000000, 9.429780353434619030E-16, -7.700000000000000178 ) ) ;
#32797 = VECTOR ( 'NONE', #86481, 1000.000000000000000 ) ;
#32798 = CARTESIAN_POINT ( 'NONE',  ( -7.300000000000013145, 2.500000000000000000, 3.883716857408420431 ) ) ;
#32799 = EDGE_CURVE ( 'NONE', #121834, #121812, #108721, .T. ) ;
#32801 = DIRECTION ( 'NONE',  ( 0.000000000000000000, 0.000000000000000000, -1.000000000000000000 ) ) ;
#32800 = CIRCLE ( 'NONE', #112299, 0.1000000000000000472 ) ;
#32802 = CARTESIAN_POINT ( 'NONE',  ( 87.50000000000001421, -1.433398978532512302, 7.395196794792774142 ) ) ;
#32803 = EDGE_LOOP ( 'NONE', ( #53778, #81641, #121553, #80992 ) ) ;
#32804 = DIRECTION ( 'NONE',  ( 0.000000000000000000, 0.000000000000000000, -1.000000000000000000 ) ) ;
#32805 = CARTESIAN_POINT ( 'NONE',  ( 9.399999999999915090, 2.500000000000000000, 4.776537180435972196 ) ) ;
#32806 = CARTESIAN_POINT ( 'NONE',  ( 3.349999999999945466, 12.50000000000000000, -2.099970236277064473 ) ) ;
#32808 = AXIS2_PLACEMENT_3D ( 'NONE', #108814, #19133, #80671 ) ;
#32807 = CONICAL_SURFACE ( 'NONE', #128956, 0.09999999999999982514, 0.003490658503988666988 ) ;
#32810 = EDGE_CURVE ( 'NONE', #527, #15992, #37800, .T. ) ;
#32809 = DIRECTION ( 'NONE',  ( -0.000000000000000000, 1.000000000000000000, -0.000000000000000000 ) ) ;
#32811 = ORIENTED_EDGE ( 'NONE', *, *, #59637, .F. ) ;
#32812 = ORIENTED_EDGE ( 'NONE', *, *, #15977, .F. ) ;
#32813 = VERTEX_POINT ( 'NONE', #77707 ) ;
#32814 = CARTESIAN_POINT ( 'NONE',  ( -11.24999999999996270, 12.50000000000000000, 6.495190528383297135 ) ) ;
#32815 = CONICAL_SURFACE ( 'NONE', #85011, 0.1000000000000002554, 0.003490658503988666988 ) ;
#32816 = CIRCLE ( 'NONE', #105951, 0.06509327318403745899 ) ;
#32817 = CARTESIAN_POINT ( 'NONE',  ( -11.04999999999999893, 2.500000000000000000, 1.818653347947321475 ) ) ;
#32818 = CARTESIAN_POINT ( 'NONE',  ( -4.800000000000022915, 2.500000000000000000, 3.983716857408420076 ) ) ;
#32819 = CIRCLE ( 'NONE', #26540, 0.1000000000000002554 ) ;
#32820 = VERTEX_POINT ( 'NONE', #118290 ) ;
#32821 = LINE ( 'NONE', #112654, #78867 ) ;
#32822 = FACE_OUTER_BOUND ( 'NONE', #8205, .T. ) ;
#32823 = FACE_OUTER_BOUND ( 'NONE', #64444, .T. ) ;
#32824 = CARTESIAN_POINT ( 'NONE',  ( -13.29999999999999005, 12.50000000000000000, -0.06509327318403558549 ) ) ;
#32825 = CARTESIAN_POINT ( 'NONE',  ( 3.749999999999938716, 2.500000000000000000, 7.088010851410848190 ) ) ;
#32826 = ORIENTED_EDGE ( 'NONE', *, *, #14298, .T. ) ;
#32827 = VERTEX_POINT ( 'NONE', #67219 ) ;
#32828 = DIRECTION ( 'NONE',  ( -0.000000000000000000, -1.000000000000000000, -0.000000000000000000 ) ) ;
#32829 = CIRCLE ( 'NONE', #116421, 0.1000000000000000472 ) ;
#32830 = DIRECTION ( 'NONE',  ( 0.000000000000000000, 1.000000000000000000, 0.000000000000000000 ) ) ;
#32831 = AXIS2_PLACEMENT_3D ( 'NONE', #43850, #11126, #112578 ) ;
#32832 = DIRECTION ( 'NONE',  ( 0.000000000000000000, 0.000000000000000000, 1.000000000000000000 ) ) ;
#32833 = CIRCLE ( 'NONE', #110189, 0.06509327318403745899 ) ;
#32834 = DIRECTION ( 'NONE',  ( 0.000000000000000000, 1.000000000000000000, 0.000000000000000000 ) ) ;
#32835 = EDGE_CURVE ( 'NONE', #54227, #85597, #79582, .T. ) ;
#32836 = ORIENTED_EDGE ( 'NONE', *, *, #57723, .F. ) ;
#32837 = VECTOR ( 'NONE', #79365, 1000.000000000000000 ) ;
#32838 = EDGE_LOOP ( 'NONE', ( #54253, #3812, #58106, #61435 ) ) ;
#32839 = DIRECTION ( 'NONE',  ( 0.000000000000000000, 0.000000000000000000, 1.000000000000000000 ) ) ;
#32840 = DIRECTION ( 'NONE',  ( 0.000000000000000000, 1.000000000000000000, 0.000000000000000000 ) ) ;
#32841 = AXIS2_PLACEMENT_3D ( 'NONE', #2403, #43662, #84200 ) ;
#32842 = CARTESIAN_POINT ( 'NONE',  ( -5.650000000000019895, 12.50000000000000000, 6.906693963081109722 ) ) ;
#32844 = DIRECTION ( 'NONE',  ( -0.000000000000000000, 1.000000000000000000, -0.000000000000000000 ) ) ;
#32843 = CONICAL_SURFACE ( 'NONE', #36949, 0.1000000000000000472, 0.003490658503988666988 ) ;
#32845 = ORIENTED_EDGE ( 'NONE', *, *, #25165, .T. ) ;
#32846 = EDGE_CURVE ( 'NONE', #4275, #53990, #102549, .T. ) ;
#32847 = DIRECTION ( 'NONE',  ( 0.000000000000000000, 0.000000000000000000, 1.000000000000000000 ) ) ;
#32848 = AXIS2_PLACEMENT_3D ( 'NONE', #52436, #20410, #92351 ) ;
#32849 = DIRECTION ( 'NONE',  ( -0.000000000000000000, 1.000000000000000000, -0.000000000000000000 ) ) ;
#32850 = VERTEX_POINT ( 'NONE', #107828 ) ;
#32851 = EDGE_CURVE ( 'NONE', #59330, #34614, #123475, .T. ) ;
#32852 = DIRECTION ( 'NONE',  ( -4.274815082592931898E-19, -0.9999939076577903929, -0.003490651415223739937 ) ) ;
#32853 = AXIS2_PLACEMENT_3D ( 'NONE', #83760, #121740, #43857 ) ;
#32854 = ADVANCED_FACE ( 'NONE', ( #18149 ), #39884, .T. ) ;
#32855 = ORIENTED_EDGE ( 'NONE', *, *, #34163, .F. ) ;
#32857 = CARTESIAN_POINT ( 'NONE',  ( 6.649999999999927525, 2.500000000000000000, 2.265063509461097357 ) ) ;
#32856 = VECTOR ( 'NONE', #113322, 1000.000000000000000 ) ;
#32859 = CONICAL_SURFACE ( 'NONE', #9765, 0.1000000000000002554, 0.003490658503988666988 ) ;
#32858 = AXIS2_PLACEMENT_3D ( 'NONE', #82826, #23901, #121435 ) ;
#32860 = VERTEX_POINT ( 'NONE', #17497 ) ;
#32861 = DIRECTION ( 'NONE',  ( -0.000000000000000000, 1.000000000000000000, -0.000000000000000000 ) ) ;
#32862 = CARTESIAN_POINT ( 'NONE',  ( 11.24999999999994493, 2.500000000000000000, -2.165063509461101710 ) ) ;
#32863 = EDGE_CURVE ( 'NONE', #117732, #107019, #86235, .T. ) ;
#32864 = EDGE_LOOP ( 'NONE', ( #14613, #4845 ) ) ;
#32865 = ORIENTED_EDGE ( 'NONE', *, *, #24349, .F. ) ;
#32866 = ADVANCED_FACE ( 'NONE', ( #88159 ), #56573, .T. ) ;
#32867 = CARTESIAN_POINT ( 'NONE',  ( 185.8802083336747444, 4.367472073101515306, 7.564683531250000925 ) ) ;
#32868 = CARTESIAN_POINT ( 'NONE',  ( 129.5000000000000000, 0.000000000000000000, 0.000000000000000000 ) ) ;
#32869 = CARTESIAN_POINT ( 'NONE',  ( 187.3385416670080872, 6.551208109652274736, 3.782341765625001351 ) ) ;
#32870 = CARTESIAN_POINT ( 'NONE',  ( 183.9427083336747160, -6.551208109652278289, 3.782341765624995134 ) ) ;
#32871 = DIRECTION ( 'NONE',  ( 0.000000000000000000, 1.000000000000000000, 0.000000000000000000 ) ) ;
#32872 = DIRECTION ( 'NONE',  ( 0.000000000000000000, 0.000000000000000000, 1.000000000000000000 ) ) ;
#32873 = CARTESIAN_POINT ( 'NONE',  ( 4.199999999999941558, 2.500000000000000000, -4.230127018922201998 ) ) ;
#32874 = DIRECTION ( 'NONE',  ( 0.000000000000000000, -0.9999939076577903929, 0.003490651415223739937 ) ) ;
#32875 = DIRECTION ( 'NONE',  ( 0.000000000000000000, 0.000000000000000000, 1.000000000000000000 ) ) ;
#32876 = AXIS2_PLACEMENT_3D ( 'NONE', #6932, #8243, #87445 ) ;
#32877 = EDGE_LOOP ( 'NONE', ( #66824, #19876, #127185, #26777 ) ) ;
#32878 = ORIENTED_EDGE ( 'NONE', *, *, #83839, .T. ) ;
#32879 = DIRECTION ( 'NONE',  ( 0.000000000000000000, 0.000000000000000000, 1.000000000000000000 ) ) ;
#32880 = EDGE_LOOP ( 'NONE', ( #31650, #57813, #18195, #25338 ) ) ;
#32881 = CARTESIAN_POINT ( 'NONE',  ( 5.599999999999934808, 2.500000000000000000, -4.676537180435978769 ) ) ;
#32882 = DIRECTION ( 'NONE',  ( 0.000000000000000000, 1.000000000000000000, 0.000000000000000000 ) ) ;
#32883 = DIRECTION ( 'NONE',  ( 0.000000000000000000, -0.000000000000000000, 1.000000000000000000 ) ) ;
#32885 = ORIENTED_EDGE ( 'NONE', *, *, #89153, .T. ) ;
#32884 = ORIENTED_EDGE ( 'NONE', *, *, #119762, .F. ) ;
#32886 = FACE_BOUND ( 'NONE', #62678, .T. ) ;
#32887 = ORIENTED_EDGE ( 'NONE', *, *, #118594, .T. ) ;
#32888 = CARTESIAN_POINT ( 'NONE',  ( -4.150000000000025224, 12.50000000000000000, 7.253104124594885960 ) ) ;
#32889 = PLANE ( 'NONE',  #93748 ) ;
#32890 = CARTESIAN_POINT ( 'NONE',  ( 8.299999999999922551, 2.500000000000000000, 4.230127018922196669 ) ) ;
#32891 = LINE ( 'NONE', #91793, #82851 ) ;
#32892 = AXIS2_PLACEMENT_3D ( 'NONE', #65393, #73938, #15638 ) ;
#32893 = LINE ( 'NONE', #119966, #68071 ) ;
#32894 = CIRCLE ( 'NONE', #57923, 0.06509327318403745899 ) ;
#32895 = DIRECTION ( 'NONE',  ( 0.000000000000000000, 1.000000000000000000, 0.000000000000000000 ) ) ;
#32896 = DIRECTION ( 'NONE',  ( -0.000000000000000000, 1.000000000000000000, -0.000000000000000000 ) ) ;
#32897 = DIRECTION ( 'NONE',  ( 0.000000000000000000, 0.000000000000000000, 1.000000000000000000 ) ) ;
#32898 = DIRECTION ( 'NONE',  ( 0.000000000000000000, 0.000000000000000000, 1.000000000000000000 ) ) ;
#32899 = PLANE ( 'NONE',  #77699 ) ;
#32900 = CARTESIAN_POINT ( 'NONE',  ( 4.799999999999937650, 2.500000000000000000, -3.983716857408426293 ) ) ;
#32903 = ADVANCED_FACE ( 'NONE', ( #76441 ), #26693, .T. ) ;
#32902 = CONICAL_SURFACE ( 'NONE', #39168, 0.09999999999999999167, 0.003490658503988666988 ) ;
#32901 = AXIS2_PLACEMENT_3D ( 'NONE', #73858, #41843, #83686 ) ;
#32904 = EDGE_LOOP ( 'NONE', ( #71241, #34992, #74017, #128775 ) ) ;
#32905 = ORIENTED_EDGE ( 'NONE', *, *, #122973, .T. ) ;
#32906 = ORIENTED_EDGE ( 'NONE', *, *, #6711, .F. ) ;
#32907 = FACE_OUTER_BOUND ( 'NONE', #121237, .T. ) ;
#32908 = EDGE_LOOP ( 'NONE', ( #48406, #100602 ) ) ;
#32909 = ADVANCED_FACE ( 'NONE', ( #77083 ), #10590, .T. ) ;
#32910 = LINE ( 'NONE', #85680, #92510 ) ;
#32911 = ADVANCED_FACE ( 'NONE', ( #56767 ), #116983, .T. ) ;
#32913 = ORIENTED_EDGE ( 'NONE', *, *, #76601, .F. ) ;
#32912 = EDGE_LOOP ( 'NONE', ( #51241, #34248, #81656, #107889 ) ) ;
#32914 = VERTEX_POINT ( 'NONE', #68538 ) ;
#32915 = ADVANCED_FACE ( 'NONE', ( #108463 ), #18793, .T. ) ;
#32916 = DIRECTION ( 'NONE',  ( 0.000000000000000000, 1.000000000000000000, 0.000000000000000000 ) ) ;
#32919 = EDGE_CURVE ( 'NONE', #112155, #18602, #8449, .T. ) ;
#32918 = AXIS2_PLACEMENT_3D ( 'NONE', #85637, #44424, #5765 ) ;
#32917 = CIRCLE ( 'NONE', #20273, 0.1000000000000002554 ) ;
#32920 = VECTOR ( 'NONE', #51234, 1000.000000000000000 ) ;
#32921 = DIRECTION ( 'NONE',  ( 0.000000000000000000, 0.000000000000000000, 1.000000000000000000 ) ) ;
#32922 = DIRECTION ( 'NONE',  ( 0.000000000000000000, 0.000000000000000000, 1.000000000000000000 ) ) ;
#32923 = ADVANCED_FACE ( 'NONE', ( #1729 ), #50848, .T. ) ;
#32924 = CARTESIAN_POINT ( 'NONE',  ( 48.83367117136233304, -2.320420702487481002, -5.300559035864880641 ) ) ;
#32925 = DIRECTION ( 'NONE',  ( -4.274815082592931898E-19, -0.9999939076577903929, -0.003490651415223739937 ) ) ;
#32926 = FACE_OUTER_BOUND ( 'NONE', #76301, .T. ) ;
#32927 = VERTEX_POINT ( 'NONE', #50214 ) ;
#32929 = ADVANCED_FACE ( 'NONE', ( #90762 ), #29411, .T. ) ;
#32928 = FACE_OUTER_BOUND ( 'NONE', #8263, .T. ) ;
#32930 = VERTEX_POINT ( 'NONE', #31218 ) ;
#32931 = VECTOR ( 'NONE', #66345, 1000.000000000000000 ) ;
#32932 = ADVANCED_FACE ( 'NONE', ( #1091 ), #115056, .T. ) ;
#32933 = ORIENTED_EDGE ( 'NONE', *, *, #124967, .F. ) ;
#32934 = ORIENTED_EDGE ( 'NONE', *, *, #13021, .T. ) ;
#32935 = CARTESIAN_POINT ( 'NONE',  ( 5.199999999999935341, 12.50000000000000000, -0.2813168883297409439 ) ) ;
#32936 = EDGE_LOOP ( 'NONE', ( #115576, #9405, #90209, #17371 ) ) ;
#32937 = ORIENTED_EDGE ( 'NONE', *, *, #12471, .T. ) ;
#32938 = ORIENTED_EDGE ( 'NONE', *, *, #109582, .T. ) ;
#32940 =( NAMED_UNIT ( * ) SI_UNIT ( $, .STERADIAN. ) SOLID_ANGLE_UNIT ( ) );
#32939 = AXIS2_PLACEMENT_3D ( 'NONE', #77949, #72014, #60277 ) ;
#32941 = DIRECTION ( 'NONE',  ( -0.000000000000000000, -1.000000000000000000, -0.000000000000000000 ) ) ;
#32942 = DIRECTION ( 'NONE',  ( 0.000000000000000000, -0.9999939076577903929, 0.003490651415223739937 ) ) ;
#32943 = DIRECTION ( 'NONE',  ( -0.000000000000000000, -1.000000000000000000, -0.000000000000000000 ) ) ;
#32944 = LINE ( 'NONE', #82682, #79660 ) ;
#32945 = VECTOR ( 'NONE', #88723, 1000.000000000000000 ) ;
#32947 = VECTOR ( 'NONE', #66496, 1000.000000000000000 ) ;
#32946 = DIRECTION ( 'NONE',  ( 0.000000000000000000, 0.000000000000000000, 1.000000000000000000 ) ) ;
#32948 = ORIENTED_EDGE ( 'NONE', *, *, #104392, .F. ) ;
#32949 = CIRCLE ( 'NONE', #26666, 0.06509327318403745899 ) ;
#32950 = CARTESIAN_POINT ( 'NONE',  ( -1.450000000000035927, 2.500000000000000000, -6.148780366869526226 ) ) ;
#32951 = VERTEX_POINT ( 'NONE', #9626 ) ;
#32952 = FACE_OUTER_BOUND ( 'NONE', #33320, .T. ) ;
#32953 = ORIENTED_EDGE ( 'NONE', *, *, #129238, .F. ) ;
#32954 = FACE_OUTER_BOUND ( 'NONE', #33295, .T. ) ;
#32955 = AXIS2_PLACEMENT_3D ( 'NONE', #49657, #117065, #68624 ) ;
#32956 = EDGE_LOOP ( 'NONE', ( #125054, #71213 ) ) ;
#32957 = CARTESIAN_POINT ( 'NONE',  ( 8.749999999999957367, 12.50000000000000000, 2.230156782645134950 ) ) ;
#32959 = CIRCLE ( 'NONE', #70486, 0.09999999999999982514 ) ;
#32958 = AXIS2_PLACEMENT_3D ( 'NONE', #75554, #55286, #55920 ) ;
#32960 = CARTESIAN_POINT ( 'NONE',  ( -7.100000000000017408, 12.50000000000000000, 0.7579135962115869374 ) ) ;
#32961 = ORIENTED_EDGE ( 'NONE', *, *, #35227, .T. ) ;
#32962 = EDGE_LOOP ( 'NONE', ( #93691, #37121 ) ) ;
#32963 = DIRECTION ( 'NONE',  ( -0.000000000000000000, 1.000000000000000000, -0.000000000000000000 ) ) ;
#32964 = CARTESIAN_POINT ( 'NONE',  ( 2.500000000000002220, 1.500000000000000444, -9.999999999999998224 ) ) ;
#32965 = CARTESIAN_POINT ( 'NONE',  ( -9.600000000000006750, 2.500000000000000000, 3.637306695894644726 ) ) ;
#32966 = CARTESIAN_POINT ( 'NONE',  ( -8.550000000000009592, 12.50000000000000000, 6.841600689897072485 ) ) ;
#32968 = EDGE_CURVE ( 'NONE', #50143, #70524, #10776, .T. ) ;
#32967 = CARTESIAN_POINT ( 'NONE',  ( -3.750000000000025757, 12.50000000000000000, -2.922977105672691422 ) ) ;
#32969 = EDGE_LOOP ( 'NONE', ( #53336, #125778 ) ) ;
#32970 = CARTESIAN_POINT ( 'NONE',  ( 1.899999999999951283, 2.500000000000000000, -4.676537180435977881 ) ) ;
#32971 = AXIS2_PLACEMENT_3D ( 'NONE', #86950, #14953, #126886 ) ;
#32972 = ORIENTED_EDGE ( 'NONE', *, *, #26473, .F. ) ;
#32973 = CARTESIAN_POINT ( 'NONE',  ( -6.450000000000017941, 12.50000000000000000, -2.511473670974877948 ) ) ;
#32974 = DIRECTION ( 'NONE',  ( 0.000000000000000000, 0.000000000000000000, 1.000000000000000000 ) ) ;
#32975 = CARTESIAN_POINT ( 'NONE',  ( 187.1250000000000284, -8.891194145520236347, -1.633285867636356693E-15 ) ) ;
#32976 = LINE ( 'NONE', #91234, #15497 ) ;
#32977 = CARTESIAN_POINT ( 'NONE',  ( 2.099999999999950351, 2.500000000000000000, -5.122947341949753763 ) ) ;
#32978 = DIRECTION ( 'NONE',  ( -4.274815082592931898E-19, -0.9999939076577903929, -0.003490651415223739937 ) ) ;
#32979 = DIRECTION ( 'NONE',  ( 0.000000000000000000, -0.000000000000000000, 1.000000000000000000 ) ) ;
#32980 = ORIENTED_EDGE ( 'NONE', *, *, #116034, .F. ) ;
#32981 = CIRCLE ( 'NONE', #64256, 0.06509327318403745899 ) ;
#32982 = CARTESIAN_POINT ( 'NONE',  ( 7.099999999999928590, 12.50000000000000000, 4.330127018922196314 ) ) ;
#32983 = AXIS2_PLACEMENT_3D ( 'NONE', #118757, #108922, #19253 ) ;
#32984 = CARTESIAN_POINT ( 'NONE',  ( 2.499999999999947153, 2.500000000000000000, 3.537306695894645081 ) ) ;
#32985 = CARTESIAN_POINT ( 'NONE',  ( 7.899999999999923084, 12.50000000000000000, -0.6277270498435167934 ) ) ;
#32986 = EDGE_LOOP ( 'NONE', ( #8531, #129163, #44462, #26111 ) ) ;
#32987 = AXIS2_PLACEMENT_3D ( 'NONE', #78815, #53047, #102146 ) ;
#32988 = DIRECTION ( 'NONE',  ( 0.000000000000000000, 0.000000000000000000, -1.000000000000000000 ) ) ;
#32989 = AXIS2_PLACEMENT_3D ( 'NONE', #94384, #15821, #55119 ) ;
#32990 = AXIS2_PLACEMENT_3D ( 'NONE', #69343, #58264, #18315 ) ;
#32991 = ORIENTED_EDGE ( 'NONE', *, *, #92988, .T. ) ;
#32992 = EDGE_LOOP ( 'NONE', ( #54072, #28468 ) ) ;
#32993 = DIRECTION ( 'NONE',  ( 0.000000000000000000, 1.000000000000000000, 0.000000000000000000 ) ) ;
#32994 = ORIENTED_EDGE ( 'NONE', *, *, #17053, .F. ) ;
#32995 = DIRECTION ( 'NONE',  ( 0.000000000000000000, 1.000000000000000000, 0.000000000000000000 ) ) ;
#32996 = FACE_OUTER_BOUND ( 'NONE', #34471, .T. ) ;
#32997 = DIRECTION ( 'NONE',  ( 0.000000000000000000, 0.000000000000000000, 1.000000000000000000 ) ) ;
#32998 = ORIENTED_EDGE ( 'NONE', *, *, #38190, .T. ) ;
#33000 = ADVANCED_FACE ( 'NONE', ( #129434 ), #109097, .T. ) ;
#32999 = CIRCLE ( 'NONE', #122873, 0.1000000000000002554 ) ;
#33001 = DIRECTION ( 'NONE',  ( 0.000000000000000000, 1.000000000000000000, 0.000000000000000000 ) ) ;
#33002 = DIRECTION ( 'NONE',  ( 0.000000000000000000, 0.000000000000000000, 1.000000000000000000 ) ) ;
#33003 = CIRCLE ( 'NONE', #76899, 0.09999999999999999167 ) ;
#33004 = ADVANCED_FACE ( 'NONE', ( #10888 ), #132, .T. ) ;
#33005 = EDGE_CURVE ( 'NONE', #4024, #88048, #16840, .T. ) ;
#33006 = EDGE_LOOP ( 'NONE', ( #58878, #86698 ) ) ;
#33007 = AXIS2_PLACEMENT_3D ( 'NONE', #110727, #121838, #21057 ) ;
#33008 = ORIENTED_EDGE ( 'NONE', *, *, #77146, .T. ) ;
#33009 = EDGE_LOOP ( 'NONE', ( #122740, #48823, #95865, #108786 ) ) ;
#33010 = VECTOR ( 'NONE', #42896, 1000.000000000000000 ) ;
#33011 = PLANE ( 'NONE',  #79773 ) ;
#33012 = CARTESIAN_POINT ( 'NONE',  ( 13.74999999999989697, 12.50000000000000000, 2.792790559304612064 ) ) ;
#33013 = ADVANCED_FACE ( 'NONE', ( #31855 ), #58656, .T. ) ;
#33014 = ADVANCED_FACE ( 'NONE', ( #101881 ), #30580, .T. ) ;
#33015 = FACE_OUTER_BOUND ( 'NONE', #42591, .T. ) ;
#33016 = EDGE_CURVE ( 'NONE', #111375, #113182, #2196, .T. ) ;
#33017 = ORIENTED_EDGE ( 'NONE', *, *, #62618, .F. ) ;
#33018 = EDGE_CURVE ( 'NONE', #35370, #63286, #50332, .T. ) ;
#33019 = CIRCLE ( 'NONE', #110267, 0.06509327318403745899 ) ;
#33020 = PLANE ( 'NONE',  #46800 ) ;
#33021 = DIRECTION ( 'NONE',  ( 0.000000000000000000, -1.846105847067148515E-16, -1.000000000000000000 ) ) ;
#33022 = EDGE_LOOP ( 'NONE', ( #91261, #125566 ) ) ;
#33023 = DIRECTION ( 'NONE',  ( 0.000000000000000000, 1.000000000000000000, 0.000000000000000000 ) ) ;
#33024 = DIRECTION ( 'NONE',  ( -0.000000000000000000, 1.000000000000000000, -0.000000000000000000 ) ) ;
#33025 = AXIS2_PLACEMENT_3D ( 'NONE', #44732, #105575, #93822 ) ;
#33026 = DIRECTION ( 'NONE',  ( 0.000000000000000000, 0.000000000000000000, 1.000000000000000000 ) ) ;
#33027 = DIRECTION ( 'NONE',  ( 0.000000000000000000, 0.000000000000000000, 1.000000000000000000 ) ) ;
#33028 = LINE ( 'NONE', #2237, #96828 ) ;
#33029 = EDGE_CURVE ( 'NONE', #48343, #79731, #127684, .T. ) ;
#33030 = DIRECTION ( 'NONE',  ( -0.000000000000000000, -1.000000000000000000, -0.000000000000000000 ) ) ;
#33031 = AXIS2_PLACEMENT_3D ( 'NONE', #68925, #70871, #20487 ) ;
#33032 = LINE ( 'NONE', #41561, #71271 ) ;
#33033 = VECTOR ( 'NONE', #53964, 1000.000000000000000 ) ;
#33034 = VERTEX_POINT ( 'NONE', #99947 ) ;
#33035 = EDGE_LOOP ( 'NONE', ( #71128, #109016, #97990, #32629 ) ) ;
#33036 = ORIENTED_EDGE ( 'NONE', *, *, #127719, .T. ) ;
#33037 = ORIENTED_EDGE ( 'NONE', *, *, #98973, .T. ) ;
#33038 = LINE ( 'NONE', #40269, #30766 ) ;
#33039 = DIRECTION ( 'NONE',  ( 0.000000000000000000, -0.9999939076577903929, 0.003490651415223739937 ) ) ;
#33040 = CYLINDRICAL_SURFACE ( 'NONE', #103130, 0.5000000000000000000 ) ;
#33041 = CIRCLE ( 'NONE', #62276, 0.09999999999999982514 ) ;
#33042 = ORIENTED_EDGE ( 'NONE', *, *, #25035, .F. ) ;
#33043 = FACE_BOUND ( 'NONE', #56914, .T. ) ;
#33044 = FACE_OUTER_BOUND ( 'NONE', #116972, .T. ) ;
#33045 = DIRECTION ( 'NONE',  ( -0.000000000000000000, 1.000000000000000000, -0.000000000000000000 ) ) ;
#33046 = FACE_OUTER_BOUND ( 'NONE', #70472, .T. ) ;
#33048 = CIRCLE ( 'NONE', #114489, 0.1000000000000002554 ) ;
#33047 = CONICAL_SURFACE ( 'NONE', #74798, 0.1000000000000002554, 0.003490658503988666988 ) ;
#33049 = CARTESIAN_POINT ( 'NONE',  ( -1.900000000000034994, 12.50000000000000000, -4.676537180435978769 ) ) ;
#33050 = DIRECTION ( 'NONE',  ( 0.000000000000000000, 1.000000000000000000, 0.000000000000000000 ) ) ;
#33051 = DIRECTION ( 'NONE',  ( 0.000000000000000000, 1.000000000000000000, 0.000000000000000000 ) ) ;
#33052 = DIRECTION ( 'NONE',  ( 0.000000000000000000, 1.000000000000000000, 0.000000000000000000 ) ) ;
#33053 = DIRECTION ( 'NONE',  ( 0.000000000000000000, 1.000000000000000000, 0.000000000000000000 ) ) ;
#33054 = ADVANCED_FACE ( 'NONE', ( #431 ), #12188, .T. ) ;
#33055 = DIRECTION ( 'NONE',  ( -0.000000000000000000, -1.000000000000000000, -0.000000000000000000 ) ) ;
#33056 = EDGE_LOOP ( 'NONE', ( #26982, #15455 ) ) ;
#33057 = EDGE_LOOP ( 'NONE', ( #20720, #64276, #69575, #22572 ) ) ;
#33058 = ORIENTED_EDGE ( 'NONE', *, *, #18657, .T. ) ;
#33059 = VERTEX_POINT ( 'NONE', #69174 ) ;
#33060 = ORIENTED_EDGE ( 'NONE', *, *, #58136, .F. ) ;
#33061 = ORIENTED_EDGE ( 'NONE', *, *, #84597, .F. ) ;
#33062 = EDGE_CURVE ( 'NONE', #60396, #77451, #21069, .T. ) ;
#33063 = DIRECTION ( 'NONE',  ( 0.000000000000000000, -0.9999939076577903929, 0.003490651415223739937 ) ) ;
#33064 = EDGE_CURVE ( 'NONE', #59538, #890, #18919, .T. ) ;
#33065 = ORIENTED_EDGE ( 'NONE', *, *, #18396, .F. ) ;
#33066 = VERTEX_POINT ( 'NONE', #63240 ) ;
#33067 = EDGE_CURVE ( 'NONE', #70330, #408, #119272, .T. ) ;
#33068 = EDGE_CURVE ( 'NONE', #101913, #110045, #94238, .T. ) ;
#33070 = AXIS2_PLACEMENT_3D ( 'NONE', #100176, #109995, #79884 ) ;
#33069 = CARTESIAN_POINT ( 'NONE',  ( 13.51931942374044660, -2.499999999999746869, 8.074217332244989720 ) ) ;
#33071 = CARTESIAN_POINT ( 'NONE',  ( 3.949999999999938005, 12.50000000000000000, 6.776507416713035248 ) ) ;
#33072 = LINE ( 'NONE', #104365, #73962 ) ;
#33073 = AXIS2_PLACEMENT_3D ( 'NONE', #31274, #41745, #122229 ) ;
#33074 = ADVANCED_FACE ( 'NONE', ( #92703 ), #52386, .T. ) ;
#33075 = EDGE_LOOP ( 'NONE', ( #122941, #108393, #85105, #52283 ) ) ;
#33076 = DIRECTION ( 'NONE',  ( -0.000000000000000000, -1.000000000000000000, -0.000000000000000000 ) ) ;
#33077 = EDGE_CURVE ( 'NONE', #79983, #37437, #34442, .T. ) ;
#33079 = ADVANCED_FACE ( 'NONE', ( #13479 ), #14785, .T. ) ;
#33078 = AXIS2_PLACEMENT_3D ( 'NONE', #24372, #64287, #64923 ) ;
#33080 = ORIENTED_EDGE ( 'NONE', *, *, #7743, .F. ) ;
#33081 = AXIS2_PLACEMENT_3D ( 'NONE', #50502, #41358, #90415 ) ;
#33082 = EDGE_CURVE ( 'NONE', #15950, #79738, #69101, .T. ) ;
#33083 = EDGE_LOOP ( 'NONE', ( #94896, #34733 ) ) ;
#33084 = DIRECTION ( 'NONE',  ( 0.000000000000000000, 0.000000000000000000, 1.000000000000000000 ) ) ;
#33085 = DIRECTION ( 'NONE',  ( -0.000000000000000000, 1.000000000000000000, -0.000000000000000000 ) ) ;
#33086 = VERTEX_POINT ( 'NONE', #93989 ) ;
#33087 = ADVANCED_FACE ( 'NONE', ( #93348 ), #32517, .T. ) ;
#33089 = ORIENTED_EDGE ( 'NONE', *, *, #86931, .T. ) ;
#33088 = VECTOR ( 'NONE', #105916, 1000.000000000000000 ) ;
#33090 = DIRECTION ( 'NONE',  ( -0.000000000000000000, -1.000000000000000000, -0.000000000000000000 ) ) ;
#33091 = AXIS2_PLACEMENT_3D ( 'NONE', #71281, #82426, #2012 ) ;
#33092 = FACE_OUTER_BOUND ( 'NONE', #120097, .T. ) ;
#33093 = DIRECTION ( 'NONE',  ( 0.000000000000000000, 1.000000000000000000, 0.000000000000000000 ) ) ;
#33094 = CARTESIAN_POINT ( 'NONE',  ( -8.950000000000006395, 2.500000000000000000, 6.841600689897072485 ) ) ;
#33095 = CARTESIAN_POINT ( 'NONE',  ( 7.899999999999923084, 12.50000000000000000, 0.6277270498435120194 ) ) ;
#33096 = EDGE_LOOP ( 'NONE', ( #124831, #55410, #100557, #74610 ) ) ;
#33097 = DIRECTION ( 'NONE',  ( -0.000000000000000000, 1.000000000000000000, -0.000000000000000000 ) ) ;
#33098 = AXIS2_PLACEMENT_3D ( 'NONE', #70054, #20311, #129002 ) ;
#33099 = VERTEX_POINT ( 'NONE', #102517 ) ;
#33100 = CARTESIAN_POINT ( 'NONE',  ( 87.50000000000002842, 6.761363245278265488, 3.308765358479924146 ) ) ;
#33101 = ORIENTED_EDGE ( 'NONE', *, *, #68302, .F. ) ;
#33102 = LINE ( 'NONE', #23244, #83971 ) ;
#33103 = FACE_OUTER_BOUND ( 'NONE', #33875, .T. ) ;
#33104 = CIRCLE ( 'NONE', #28977, 0.06509327318403745899 ) ;
#33105 = CARTESIAN_POINT ( 'NONE',  ( 2.949999999999945111, 12.50000000000000000, 2.165063509461097713 ) ) ;
#33106 = DIRECTION ( 'NONE',  ( 0.000000000000000000, 0.000000000000000000, -1.000000000000000000 ) ) ;
#33107 = ORIENTED_EDGE ( 'NONE', *, *, #101456, .T. ) ;
#33109 = AXIS2_PLACEMENT_3D ( 'NONE', #99434, #77831, #128905 ) ;
#33108 = CARTESIAN_POINT ( 'NONE',  ( -5.850000000000021849, 2.500000000000000000, -7.088010851410853519 ) ) ;
#33110 = STYLED_ITEM ( 'NONE', ( #74118 ), #21197 ) ;
#33111 = DIRECTION ( 'NONE',  ( 0.000000000000000000, -0.9999939076577903929, 0.003490651415223739937 ) ) ;
#33112 = ORIENTED_EDGE ( 'NONE', *, *, #50466, .F. ) ;
#33113 = ORIENTED_EDGE ( 'NONE', *, *, #125996, .T. ) ;
#33114 = ORIENTED_EDGE ( 'NONE', *, *, #60573, .T. ) ;
#33115 = DIRECTION ( 'NONE',  ( 0.000000000000000000, 0.000000000000000000, -1.000000000000000000 ) ) ;
#33116 = DIRECTION ( 'NONE',  ( 0.000000000000000000, 1.000000000000000000, 0.000000000000000000 ) ) ;
#33117 = CARTESIAN_POINT ( 'NONE',  ( 186.3177083336747160, 4.367472073101515306, 7.564683531250000925 ) ) ;
#33118 = FACE_OUTER_BOUND ( 'NONE', #59, .T. ) ;
#33119 = PLANE ( 'NONE',  #40309 ) ;
#33121 = EDGE_CURVE ( 'NONE', #96527, #30923, #43618, .T. ) ;
#33120 = FACE_OUTER_BOUND ( 'NONE', #86075, .T. ) ;
#33122 = CARTESIAN_POINT ( 'NONE',  ( 4.999999999999969802, 2.500000000000000000, 4.330127018922196314 ) ) ;
#33123 = CARTESIAN_POINT ( 'NONE',  ( -8.300000000000011369, 2.500000000000000000, -2.276824562219559311E-15 ) ) ;
#33124 = ORIENTED_EDGE ( 'NONE', *, *, #84490, .F. ) ;
#33125 = DIRECTION ( 'NONE',  ( 0.000000000000000000, 0.000000000000000000, 1.000000000000000000 ) ) ;
#33126 = ADVANCED_FACE ( 'NONE', ( #42987 ), #233, .T. ) ;
#33127 = CARTESIAN_POINT ( 'NONE',  ( -5.600000000000020073, 2.500000000000000000, -0.2464101615137782308 ) ) ;
#33128 = DIRECTION ( 'NONE',  ( 0.000000000000000000, -0.000000000000000000, 1.000000000000000000 ) ) ;
#33129 = CARTESIAN_POINT ( 'NONE',  ( -5.650000000000023448, 2.500000000000000000, -6.148780366869526226 ) ) ;
#33130 = ORIENTED_EDGE ( 'NONE', *, *, #113486, .F. ) ;
#33131 = CARTESIAN_POINT ( 'NONE',  ( 4.549999999999935874, 2.500000000000000000, 6.495190528383297135 ) ) ;
#33132 = CONICAL_SURFACE ( 'NONE', #43699, 0.09999999999999982514, 0.003490658503988666988 ) ;
#33133 = DIRECTION ( 'NONE',  ( 0.000000000000000000, 0.000000000000000000, 1.000000000000000000 ) ) ;
#33135 = ORIENTED_EDGE ( 'NONE', *, *, #94944, .F. ) ;
#33134 = DIRECTION ( 'NONE',  ( 0.000000000000000000, 0.000000000000000000, 1.000000000000000000 ) ) ;
#33136 = VERTEX_POINT ( 'NONE', #82893 ) ;
#33137 = CARTESIAN_POINT ( 'NONE',  ( 13.09999999999990195, 2.500000000000000000, -4.676537180435978769 ) ) ;
#33138 = ORIENTED_EDGE ( 'NONE', *, *, #92410, .F. ) ;
#33139 = ORIENTED_EDGE ( 'NONE', *, *, #42241, .F. ) ;
#33140 = CARTESIAN_POINT ( 'NONE',  ( -7.500000000000015099, 12.50000000000000000, -4.957854068765716882 ) ) ;
#33141 = AXIS2_PLACEMENT_3D ( 'NONE', #17186, #97071, #111381 ) ;
#33142 = ORIENTED_EDGE ( 'NONE', *, *, #123623, .F. ) ;
#33143 = DIRECTION ( 'NONE',  ( 0.000000000000000000, -0.000000000000000000, 1.000000000000000000 ) ) ;
#33144 = DIRECTION ( 'NONE',  ( -0.000000000000000000, -1.000000000000000000, -0.000000000000000000 ) ) ;
#33145 = DIRECTION ( 'NONE',  ( 0.000000000000000000, 0.000000000000000000, 1.000000000000000000 ) ) ;
#33146 = VERTEX_POINT ( 'NONE', #124089 ) ;
#33147 = AXIS2_PLACEMENT_3D ( 'NONE', #19076, #119232, #120530 ) ;
#33148 = EDGE_CURVE ( 'NONE', #7115, #31484, #83535, .T. ) ;
#33149 = CIRCLE ( 'NONE', #64714, 0.1000000000000002554 ) ;
#33150 = VECTOR ( 'NONE', #96629, 1000.000000000000000 ) ;
#33151 = CARTESIAN_POINT ( 'NONE',  ( 8.549999999999918998, 2.500000000000000000, -1.718653347947326049 ) ) ;
#33153 = ORIENTED_EDGE ( 'NONE', *, *, #97032, .F. ) ;
#33152 = DIRECTION ( 'NONE',  ( 0.000000000000000000, 1.000000000000000000, 0.000000000000000000 ) ) ;
#33154 = DIRECTION ( 'NONE',  ( 0.000000000000000000, 0.000000000000000000, -1.000000000000000000 ) ) ;
#33155 = CARTESIAN_POINT ( 'NONE',  ( 186.2812500006828031, 0.000000000000000000, 7.700000000000000178 ) ) ;
#33156 = EDGE_CURVE ( 'NONE', #85507, #92060, #113631, .T. ) ;
#33157 = CONICAL_SURFACE ( 'NONE', #81268, 0.1000000000000002554, 0.003490658503988666988 ) ;
#33158 = ORIENTED_EDGE ( 'NONE', *, *, #119862, .F. ) ;
#33159 = AXIS2_PLACEMENT_3D ( 'NONE', #51114, #1344, #1987 ) ;
#33160 = AXIS2_PLACEMENT_3D ( 'NONE', #122906, #1823, #81679 ) ;
#33161 = ORIENTED_EDGE ( 'NONE', *, *, #115815, .T. ) ;
#33162 = ORIENTED_EDGE ( 'NONE', *, *, #81406, .T. ) ;
#33163 = VERTEX_POINT ( 'NONE', #4287 ) ;
#33164 = FACE_OUTER_BOUND ( 'NONE', #93605, .T. ) ;
#33165 = CARTESIAN_POINT ( 'NONE',  ( 11.75764115780555485, 2.499999999999999556, 7.679135278102248385 ) ) ;
#33166 = EDGE_CURVE ( 'NONE', #42431, #34783, #60878, .T. ) ;
#33167 = EDGE_CURVE ( 'NONE', #3107, #67445, #94315, .T. ) ;
#33168 = CARTESIAN_POINT ( 'NONE',  ( 9.999999999999912959, 12.50000000000000000, 3.637306695894644726 ) ) ;
#33169 = EDGE_CURVE ( 'NONE', #45268, #111304, #52464, .T. ) ;
#33170 = FACE_BOUND ( 'NONE', #87141, .T. ) ;
#33172 = EDGE_CURVE ( 'NONE', #69112, #5314, #16930, .T. ) ;
#33171 = VERTEX_POINT ( 'NONE', #121947 ) ;
#33173 = CARTESIAN_POINT ( 'NONE',  ( 184.4479166673494603, -6.668395609140176816, -3.850000000000003642 ) ) ;
#33174 = EDGE_CURVE ( 'NONE', #116569, #113123, #35755, .T. ) ;
#33175 = CONICAL_SURFACE ( 'NONE', #16502, 0.1000000000000000472, 0.003490658503988666988 ) ;
#33176 = CARTESIAN_POINT ( 'NONE',  ( -8.550000000000011369, 12.50000000000000000, -2.576566944158915184 ) ) ;
#33177 = DIRECTION ( 'NONE',  ( -4.274815082592931898E-19, -0.9999939076577903929, -0.003490651415223739937 ) ) ;
#33178 = CARTESIAN_POINT ( 'NONE',  ( -13.29999999999999005, 12.50000000000000000, -4.395220292106237103 ) ) ;
#33179 = CARTESIAN_POINT ( 'NONE',  ( 6.649999999999930189, 2.500000000000000000, -2.757883832488654097 ) ) ;
#33180 = EDGE_CURVE ( 'NONE', #97627, #51148, #64981, .T. ) ;
#33181 = DIRECTION ( 'NONE',  ( -0.000000000000000000, 1.000000000000000000, -0.000000000000000000 ) ) ;
#33182 = ADVANCED_FACE ( 'NONE', ( #81392 ), #125621, .T. ) ;
#33183 = AXIS2_PLACEMENT_3D ( 'NONE', #81012, #71181, #496 ) ;
#33184 = EDGE_CURVE ( 'NONE', #50067, #54857, #10059, .T. ) ;
#33185 = PLANE ( 'NONE',  #93335 ) ;
#33186 = ORIENTED_EDGE ( 'NONE', *, *, #1802, .T. ) ;
#33187 = VERTEX_POINT ( 'NONE', #31636 ) ;
#33188 = VERTEX_POINT ( 'NONE', #42101 ) ;
#33189 = CLOSED_SHELL ( 'NONE', ( #78152, #101719, #106871, #17906, #59315, #34332, #5997, #94137, #31525, #99429, #19275, #64468, #61554, #11467 ) ) ;
#33190 = ORIENTED_EDGE ( 'NONE', *, *, #35216, .F. ) ;
#33191 = ORIENTED_EDGE ( 'NONE', *, *, #77746, .T. ) ;
#33192 = CIRCLE ( 'NONE', #6052, 0.06509327318403743123 ) ;
#33193 = DIRECTION ( 'NONE',  ( 0.000000000000000000, -0.000000000000000000, 1.000000000000000000 ) ) ;
#33194 = CARTESIAN_POINT ( 'NONE',  ( 15.83209681635554666, 2.500000000000000000, 5.404881881984142211 ) ) ;
#33195 = ORIENTED_EDGE ( 'NONE', *, *, #11329, .F. ) ;
#33196 = FACE_BOUND ( 'NONE', #36864, .T. ) ;
#33197 = DIRECTION ( 'NONE',  ( -4.274815082592931898E-19, -0.9999939076577903929, -0.003490651415223739937 ) ) ;
#33198 = CIRCLE ( 'NONE', #5967, 0.06509327318403745899 ) ;
#33199 = STYLED_ITEM ( 'NONE', ( #70731 ), #108597 ) ;
#33200 = VERTEX_POINT ( 'NONE', #82013 ) ;
#33201 = DIRECTION ( 'NONE',  ( 0.000000000000000000, 0.000000000000000000, 1.000000000000000000 ) ) ;
#33202 = DIRECTION ( 'NONE',  ( -0.000000000000000000, -1.000000000000000000, -0.000000000000000000 ) ) ;
#33203 = DIRECTION ( 'NONE',  ( -0.000000000000000000, -1.000000000000000000, -0.000000000000000000 ) ) ;
#33204 = EDGE_LOOP ( 'NONE', ( #128404, #82221 ) ) ;
#33205 = CIRCLE ( 'NONE', #49930, 0.09999999999999982514 ) ;
#33206 = DIRECTION ( 'NONE',  ( -0.000000000000000000, -1.000000000000000000, -0.000000000000000000 ) ) ;
#33208 = ORIENTED_EDGE ( 'NONE', *, *, #29790, .F. ) ;
#33207 = CIRCLE ( 'NONE', #20676, 0.06509327318403745899 ) ;
#33209 = ORIENTED_EDGE ( 'NONE', *, *, #125068, .T. ) ;
#33210 = ORIENTED_EDGE ( 'NONE', *, *, #1085, .F. ) ;
#33211 = DIRECTION ( 'NONE',  ( 0.000000000000000000, 1.000000000000000000, 0.000000000000000000 ) ) ;
#33212 = CARTESIAN_POINT ( 'NONE',  ( -8.950000000000008171, 2.500000000000000000, -2.411473670974877859 ) ) ;
#33213 = DIRECTION ( 'NONE',  ( 0.000000000000000000, 0.000000000000000000, 1.000000000000000000 ) ) ;
#33214 = CONICAL_SURFACE ( 'NONE', #118874, 0.09999999999999982514, 0.003490658503988666988 ) ;
#33215 = ORIENTED_EDGE ( 'NONE', *, *, #83602, .T. ) ;
#33216 = FACE_OUTER_BOUND ( 'NONE', #112621, .T. ) ;
#33217 = CARTESIAN_POINT ( 'NONE',  ( -7.050000000000016698, 12.50000000000000000, -2.099970236277064473 ) ) ;
#33220 = AXIS2_PLACEMENT_3D ( 'NONE', #102057, #109947, #110579 ) ;
#33219 = DIRECTION ( 'NONE',  ( 0.000000000000000000, 1.000000000000000000, 0.000000000000000000 ) ) ;
#33218 = CIRCLE ( 'NONE', #3945, 0.06509327318403745899 ) ;
#33221 = CARTESIAN_POINT ( 'NONE',  ( 185.5729166673494319, 4.445597072760120838, -7.699999999999998401 ) ) ;
#33222 = ORIENTED_EDGE ( 'NONE', *, *, #65518, .T. ) ;
#33223 = CIRCLE ( 'NONE', #91694, 0.06509327318403745899 ) ;
#33224 = CARTESIAN_POINT ( 'NONE',  ( -4.600000000000028066, 12.50000000000000000, -5.022947341949754119 ) ) ;
#33225 = ADVANCED_FACE ( 'NONE', ( #51926 ), #59834, .T. ) ;
#33226 = EDGE_LOOP ( 'NONE', ( #9172, #109653, #69716, #103797 ) ) ;
#33227 = LINE ( 'NONE', #73132, #113990 ) ;
#33228 = ADVANCED_FACE ( 'NONE', ( #80743 ), #102640, .T. ) ;
#33229 = CIRCLE ( 'NONE', #93759, 0.09999999999999982514 ) ;
#33230 = EDGE_LOOP ( 'NONE', ( #14679, #90507 ) ) ;
#33231 = ADVANCED_FACE ( 'NONE', ( #91844 ), #42010, .T. ) ;
#33232 = ORIENTED_EDGE ( 'NONE', *, *, #81780, .T. ) ;
#33233 = DIRECTION ( 'NONE',  ( 0.000000000000000000, 0.000000000000000000, 1.000000000000000000 ) ) ;
#33234 = CARTESIAN_POINT ( 'NONE',  ( 14.59999999999989484, 2.500000000000000000, -0.6928203230275541413 ) ) ;
#33235 = FACE_OUTER_BOUND ( 'NONE', #91347, .T. ) ;
#33236 = CARTESIAN_POINT ( 'NONE',  ( 10.64999999999990976, 12.50000000000000000, 1.818653347947321475 ) ) ;
#33237 = DIRECTION ( 'NONE',  ( 0.000000000000000000, 0.000000000000000000, 1.000000000000000000 ) ) ;
#33238 = ORIENTED_EDGE ( 'NONE', *, *, #113676, .F. ) ;
#33239 = ADVANCED_FACE ( 'NONE', ( #19885 ), #104772, .T. ) ;
#33240 = EDGE_LOOP ( 'NONE', ( #118892, #51229, #37829, #36249 ) ) ;
#33241 = CARTESIAN_POINT ( 'NONE',  ( -6.900000000000019007, 12.50000000000000000, -4.676537180435978769 ) ) ;
#33242 = CARTESIAN_POINT ( 'NONE',  ( 0.000000000000000000, 0.5000000000000000000, 0.000000000000000000 ) ) ;
#33243 = DIRECTION ( 'NONE',  ( 0.000000000000000000, 1.000000000000000000, 0.000000000000000000 ) ) ;
#33244 = ORIENTED_EDGE ( 'NONE', *, *, #60280, .T. ) ;
#33245 = VERTEX_POINT ( 'NONE', #122593 ) ;
#33246 = DIRECTION ( 'NONE',  ( 0.000000000000000000, 0.000000000000000000, 1.000000000000000000 ) ) ;
#33247 = ORIENTED_EDGE ( 'NONE', *, *, #44592, .F. ) ;
#33248 = DIRECTION ( 'NONE',  ( 0.000000000000000000, -0.9999939076577903929, 0.003490651415223739937 ) ) ;
#33249 = CARTESIAN_POINT ( 'NONE',  ( -0.4000000000000396572, 2.500000000000000000, 3.637306695894644726 ) ) ;
#33250 = AXIS2_PLACEMENT_3D ( 'NONE', #47130, #74640, #46459 ) ;
#33252 = FACE_OUTER_BOUND ( 'NONE', #117543, .T. ) ;
#33251 = CIRCLE ( 'NONE', #26875, 0.06509327318403745899 ) ;
#33253 = ORIENTED_EDGE ( 'NONE', *, *, #50577, .F. ) ;
#33254 = CARTESIAN_POINT ( 'NONE',  ( -8.300000000000011369, 2.500000000000000000, -4.230127018922201998 ) ) ;
#33255 = CARTESIAN_POINT ( 'NONE',  ( 0.000000000000000000, 2.500000000000000000, 0.000000000000000000 ) ) ;
#33256 = DIRECTION ( 'NONE',  ( -0.000000000000000000, 1.000000000000000000, -0.000000000000000000 ) ) ;
#33257 = CARTESIAN_POINT ( 'NONE',  ( 10.84999999999990905, 2.500000000000000000, 2.065063509461097624 ) ) ;
#33258 = EDGE_CURVE ( 'NONE', #107723, #44898, #111470, .T. ) ;
#33259 = CARTESIAN_POINT ( 'NONE',  ( 5.599999999999931255, 12.50000000000000000, 3.983716857408420076 ) ) ;
#33260 = CIRCLE ( 'NONE', #18648, 0.06509327318403745899 ) ;
#33261 = ORIENTED_EDGE ( 'NONE', *, *, #117831, .T. ) ;
#33262 = VECTOR ( 'NONE', #128231, 1000.000000000000000 ) ;
#33264 = DIRECTION ( 'NONE',  ( 0.000000000000000000, 0.000000000000000000, 1.000000000000000000 ) ) ;
#33263 = AXIS2_PLACEMENT_3D ( 'NONE', #84569, #56384, #7927 ) ;
#33265 = CARTESIAN_POINT ( 'NONE',  ( 65.40459994265785326, -3.824478557808927093, 5.306485876512247124 ) ) ;
#33266 = ORIENTED_EDGE ( 'NONE', *, *, #64884, .T. ) ;
#33267 = EDGE_LOOP ( 'NONE', ( #95076, #66238 ) ) ;
#33268 = CARTESIAN_POINT ( 'NONE',  ( 187.0885416670080872, -6.551208109652273848, -3.782341765625003571 ) ) ;
#33269 = DIRECTION ( 'NONE',  ( 0.000000000000000000, 0.000000000000000000, 1.000000000000000000 ) ) ;
#33270 = DIRECTION ( 'NONE',  ( 0.000000000000000000, 0.000000000000000000, -1.000000000000000000 ) ) ;
#33271 = CIRCLE ( 'NONE', #114803, 0.09999999999999999167 ) ;
#33272 = DIRECTION ( 'NONE',  ( 0.000000000000000000, -0.9999939076577903929, 0.003490651415223739937 ) ) ;
#33273 = LINE ( 'NONE', #73807, #8795 ) ;
#33274 = AXIS2_PLACEMENT_3D ( 'NONE', #17632, #79164, #97493 ) ;
#33275 = CARTESIAN_POINT ( 'NONE',  ( 9.599999999999917932, 2.500000000000000000, 0.5928203230275495006 ) ) ;
#33277 = ADVANCED_FACE ( 'NONE', ( #92479 ), #10685, .T. ) ;
#33276 = DIRECTION ( 'NONE',  ( 0.000000000000000000, 0.000000000000000000, -1.000000000000000000 ) ) ;
#33278 = CARTESIAN_POINT ( 'NONE',  ( -2.950000000000033484, 2.500000000000000000, -6.395190528383301931 ) ) ;
#33279 = PLANE ( 'NONE',  #54019 ) ;
#33280 = DIRECTION ( 'NONE',  ( 0.000000000000000000, 0.000000000000000000, 1.000000000000000000 ) ) ;
#33281 = CIRCLE ( 'NONE', #39554, 0.06509327318403745899 ) ;
#33282 = ORIENTED_EDGE ( 'NONE', *, *, #123460, .T. ) ;
#33283 = ORIENTED_EDGE ( 'NONE', *, *, #118180, .T. ) ;
#33284 = ORIENTED_EDGE ( 'NONE', *, *, #91538, .F. ) ;
#33285 = CIRCLE ( 'NONE', #112687, 0.06509327318403745899 ) ;
#33286 = ORIENTED_EDGE ( 'NONE', *, *, #56487, .F. ) ;
#33287 = ADVANCED_FACE ( 'NONE', ( #21825 ), #46211, .T. ) ;
#33288 = DIRECTION ( 'NONE',  ( 0.000000000000000000, 1.000000000000000000, 0.000000000000000000 ) ) ;
#33289 = DIRECTION ( 'NONE',  ( 0.000000000000000000, 0.000000000000000000, -1.000000000000000000 ) ) ;
#33290 = ORIENTED_EDGE ( 'NONE', *, *, #114840, .F. ) ;
#33291 = CARTESIAN_POINT ( 'NONE',  ( 7.099999999999925926, 12.50000000000000000, 0.6928203230275494784 ) ) ;
#33292 = CIRCLE ( 'NONE', #106423, 0.06509327318403745899 ) ;
#33293 = CARTESIAN_POINT ( 'NONE',  ( 3.349999999999942801, 2.500000000000000000, 2.857883832488649301 ) ) ;
#33295 = EDGE_LOOP ( 'NONE', ( #28055, #128522 ) ) ;
#33294 = CARTESIAN_POINT ( 'NONE',  ( -12.04999999999999716, 12.50000000000000000, -6.495190528383298911 ) ) ;
#33296 = CARTESIAN_POINT ( 'NONE',  ( 15.39999999999989200, 2.500000000000000000, 0.6928203230275494784 ) ) ;
#33297 = PLANE ( 'NONE',  #91813 ) ;
#33298 = ORIENTED_EDGE ( 'NONE', *, *, #4889, .F. ) ;
#33299 = AXIS2_PLACEMENT_3D ( 'NONE', #95283, #46175, #84157 ) ;
#33300 = EDGE_LOOP ( 'NONE', ( #6787, #25094 ) ) ;
#33301 = ORIENTED_EDGE ( 'NONE', *, *, #30077, .F. ) ;
#33302 = ORIENTED_EDGE ( 'NONE', *, *, #55346, .F. ) ;
#33303 = DIRECTION ( 'NONE',  ( -4.274815082592931898E-19, -0.9999939076577903929, -0.003490651415223739937 ) ) ;
#33304 = CIRCLE ( 'NONE', #106440, 0.09999999999999999167 ) ;
#33305 = DIRECTION ( 'NONE',  ( -4.274815082592931898E-19, -0.9999939076577903929, -0.003490651415223739937 ) ) ;
#33306 = DIRECTION ( 'NONE',  ( 0.000000000000000000, 1.000000000000000000, 0.000000000000000000 ) ) ;
#33307 = CARTESIAN_POINT ( 'NONE',  ( 2.099999999999950351, 12.50000000000000000, -4.330127018922201643 ) ) ;
#33308 = VERTEX_POINT ( 'NONE', #42770 ) ;
#33309 = EDGE_CURVE ( 'NONE', #79506, #25742, #32944, .T. ) ;
#33311 = AXIS2_PLACEMENT_3D ( 'NONE', #120259, #30599, #41070 ) ;
#33310 = CIRCLE ( 'NONE', #85604, 0.09999999999999982514 ) ;
#33312 = FACE_OUTER_BOUND ( 'NONE', #32522, .T. ) ;
#33313 = VERTEX_POINT ( 'NONE', #60472 ) ;
#33314 = CARTESIAN_POINT ( 'NONE',  ( 179.5000000000000000, 0.6250000000000025535, -6.000000000000000888 ) ) ;
#33316 = AXIS2_PLACEMENT_3D ( 'NONE', #115583, #25941, #106422 ) ;
#33315 = CARTESIAN_POINT ( 'NONE',  ( 8.497934422629066731, -2.500000000000762057, -9.526046681109040293 ) ) ;
#33317 = DIRECTION ( 'NONE',  ( -4.274815082592931898E-19, -0.9999939076577903929, -0.003490651415223739937 ) ) ;
#33318 = DIRECTION ( 'NONE',  ( -0.000000000000000000, 1.000000000000000000, -0.000000000000000000 ) ) ;
#33319 = EDGE_CURVE ( 'NONE', #82277, #28259, #100374, .T. ) ;
#33320 = EDGE_LOOP ( 'NONE', ( #104265, #121178, #101241, #42370 ) ) ;
#33321 = AXIS2_PLACEMENT_3D ( 'NONE', #93345, #112978, #54061 ) ;
#33322 = ORIENTED_EDGE ( 'NONE', *, *, #39887, .T. ) ;
#33323 = ORIENTED_EDGE ( 'NONE', *, *, #86622, .T. ) ;
#33324 = FACE_OUTER_BOUND ( 'NONE', #3761, .T. ) ;
#33325 = DIRECTION ( 'NONE',  ( -0.000000000000000000, 1.000000000000000000, -0.000000000000000000 ) ) ;
#33326 = EDGE_CURVE ( 'NONE', #117920, #69856, #110823, .T. ) ;
#33327 = ADVANCED_FACE ( 'NONE', ( #96215 ), #65067, .T. ) ;
#33328 = LINE ( 'NONE', #111872, #92022 ) ;
#33329 = EDGE_CURVE ( 'NONE', #79083, #12477, #75451, .T. ) ;
#33330 = FACE_BOUND ( 'NONE', #75332, .T. ) ;
#33331 = ADVANCED_FACE ( 'NONE', ( #114570 ), #54608, .T. ) ;
#33332 = DIRECTION ( 'NONE',  ( -0.000000000000000000, -1.000000000000000000, -0.000000000000000000 ) ) ;
#33333 = LINE ( 'NONE', #73237, #71734 ) ;
#33334 = LINE ( 'NONE', #44416, #1887 ) ;
#33335 = ADVANCED_FACE ( 'NONE', ( #66759 ), #44559, .F. ) ;
#33336 = CIRCLE ( 'NONE', #104416, 0.1000000000000000472 ) ;
#33337 = FACE_OUTER_BOUND ( 'NONE', #17161, .T. ) ;
#33338 = ADVANCED_FACE ( 'NONE', ( #17663 ), #6521, .T. ) ;
#33339 = DIRECTION ( 'NONE',  ( 0.000000000000000000, 0.000000000000000000, 1.000000000000000000 ) ) ;
#33340 = ADVANCED_FACE ( 'NONE', ( #16983 ), #25537, .T. ) ;
#33341 = FACE_OUTER_BOUND ( 'NONE', #108887, .T. ) ;
#33342 = VERTEX_POINT ( 'NONE', #84485 ) ;
#33343 = ADVANCED_FACE ( 'NONE', ( #124410 ), #92176, .T. ) ;
#33344 = AXIS2_PLACEMENT_3D ( 'NONE', #35228, #124241, #26038 ) ;
#33345 = EDGE_CURVE ( 'NONE', #50751, #65093, #86399, .T. ) ;
#33346 = AXIS2_PLACEMENT_3D ( 'NONE', #18274, #66723, #9752 ) ;
#33347 = DIRECTION ( 'NONE',  ( 0.000000000000000000, 0.000000000000000000, 1.000000000000000000 ) ) ;
#33348 = ORIENTED_EDGE ( 'NONE', *, *, #120975, .T. ) ;
#33349 = ORIENTED_EDGE ( 'NONE', *, *, #73254, .T. ) ;
#33350 = DIRECTION ( 'NONE',  ( -0.000000000000000000, 1.000000000000000000, -0.000000000000000000 ) ) ;
#33351 = FACE_BOUND ( 'NONE', #102293, .T. ) ;
#33352 = EDGE_CURVE ( 'NONE', #110270, #57844, #126345, .T. ) ;
#33353 = DIRECTION ( 'NONE',  ( -0.000000000000000000, -1.000000000000000000, -0.000000000000000000 ) ) ;
#33354 = CIRCLE ( 'NONE', #64713, 0.06509327318403745899 ) ;
#33355 = AXIS2_PLACEMENT_3D ( 'NONE', #124196, #85552, #84257 ) ;
#33356 = CONICAL_SURFACE ( 'NONE', #58391, 0.1000000000000002554, 0.003490658503988666988 ) ;
#33357 = EDGE_LOOP ( 'NONE', ( #89369, #53830, #72467, #50305 ) ) ;
#33358 = CARTESIAN_POINT ( 'NONE',  ( 32.27111852103329426, 3.178312372602895675, 3.140919221358756452 ) ) ;
#33359 = CARTESIAN_POINT ( 'NONE',  ( -3.300000000000027800, 2.500000000000000000, -2.276824562219559311E-15 ) ) ;
#33360 = AXIS2_PLACEMENT_3D ( 'NONE', #73546, #63747, #13980 ) ;
#33361 = ORIENTED_EDGE ( 'NONE', *, *, #106189, .T. ) ;
#33362 = CARTESIAN_POINT ( 'NONE',  ( -3.350000000000031619, 2.500000000000000000, -7.288010851410854585 ) ) ;
#33363 = DIRECTION ( 'NONE',  ( 0.000000000000000000, 1.000000000000000000, 0.000000000000000000 ) ) ;
#33364 = CONICAL_SURFACE ( 'NONE', #127440, 0.1000000000000002554, 0.003490658503988666988 ) ;
#33365 = VECTOR ( 'NONE', #81908, 1000.000000000000000 ) ;
#33366 = ORIENTED_EDGE ( 'NONE', *, *, #41248, .F. ) ;
#33367 = DIRECTION ( 'NONE',  ( 0.000000000000000000, 0.000000000000000000, -1.000000000000000000 ) ) ;
#33368 = DIRECTION ( 'NONE',  ( 0.000000000000000000, 1.000000000000000000, 0.000000000000000000 ) ) ;
#33369 = EDGE_LOOP ( 'NONE', ( #97393, #51488, #119364, #118651 ) ) ;
#33370 = DIRECTION ( 'NONE',  ( 0.000000000000000000, 0.000000000000000000, -1.000000000000000000 ) ) ;
#33371 = DIRECTION ( 'NONE',  ( 0.000000000000000000, 0.000000000000000000, 1.000000000000000000 ) ) ;
#33372 = LINE ( 'NONE', #62184, #51433 ) ;
#33373 = AXIS2_PLACEMENT_3D ( 'NONE', #63651, #52530, #64277 ) ;
#33374 = EDGE_LOOP ( 'NONE', ( #90004, #73121 ) ) ;
#33375 = ORIENTED_EDGE ( 'NONE', *, *, #76870, .F. ) ;
#33376 = DIRECTION ( 'NONE',  ( 0.000000000000000000, 1.000000000000000000, 0.000000000000000000 ) ) ;
#33377 = EDGE_LOOP ( 'NONE', ( #111135, #92115, #80805, #78888 ) ) ;
#33378 = CARTESIAN_POINT ( 'NONE',  ( -14.99999999999998224, 2.500000000000000000, -0.7928203230275518987 ) ) ;
#33379 = DIRECTION ( 'NONE',  ( 0.000000000000000000, -0.000000000000000000, 1.000000000000000000 ) ) ;
#33380 = EDGE_CURVE ( 'NONE', #102542, #84188, #39962, .T. ) ;
#33381 = ORIENTED_EDGE ( 'NONE', *, *, #86315, .F. ) ;
#33383 = ADVANCED_FACE ( 'NONE', ( #85756 ), #10768, .T. ) ;
#33382 = CARTESIAN_POINT ( 'NONE',  ( -11.05000000000000071, 2.500000000000000000, -2.511473670974873951 ) ) ;
#33384 = DIRECTION ( 'NONE',  ( 0.000000000000000000, -0.9999939076577903929, 0.003490651415223739937 ) ) ;
#33385 = CARTESIAN_POINT ( 'NONE',  ( -7.900000000000014566, 2.500000000000000000, -3.737306695894649700 ) ) ;
#33386 =( BOUNDED_CURVE ( )  B_SPLINE_CURVE ( 2, ( #73452, #24367, #113380, #54462, #55117, #103581, #123834 ),
 .UNSPECIFIED., .F., .F. ) 
 B_SPLINE_CURVE_WITH_KNOTS ( ( 3, 2, 2, 3 ),
 ( 0.1428571428571429880, 0.1666666666666668239, 0.1904761904761906322, 0.2142857142857144681 ),
 .UNSPECIFIED. ) 
 CURVE ( )  GEOMETRIC_REPRESENTATION_ITEM ( )  RATIONAL_B_SPLINE_CURVE ( ( 0.9999999999999992228, 0.8660254037844394848, 1.000000000000000000, 0.8660254037844387076, 1.000000000000000000, 0.8660254037844375974, 1.000000000000001110 ) ) 
 REPRESENTATION_ITEM ( '' )  );
#33387 = FACE_OUTER_BOUND ( 'NONE', #75626, .T. ) ;
#33388 = CARTESIAN_POINT ( 'NONE',  ( 2.499999999999981792, 12.50000000000000000, 4.330127018922196314 ) ) ;
#33389 = EDGE_CURVE ( 'NONE', #110247, #16833, #47142, .T. ) ;
#33390 = VERTEX_POINT ( 'NONE', #87046 ) ;
#33391 = ORIENTED_EDGE ( 'NONE', *, *, #103819, .T. ) ;
#33392 = CARTESIAN_POINT ( 'NONE',  ( -0.6500000000000403233, 12.50000000000000000, 6.213873640053558134 ) ) ;
#33393 = ORIENTED_EDGE ( 'NONE', *, *, #60748, .F. ) ;
#33394 = CARTESIAN_POINT ( 'NONE',  ( 103.0671989394255945, 7.656491474633341454, -0.8341323537259196508 ) ) ;
#33396 = ORIENTED_EDGE ( 'NONE', *, *, #121136, .F. ) ;
#33395 = ORIENTED_EDGE ( 'NONE', *, *, #120350, .T. ) ;
#33397 = ORIENTED_EDGE ( 'NONE', *, *, #29686, .T. ) ;
#33398 = AXIS2_PLACEMENT_3D ( 'NONE', #76848, #116751, #7441 ) ;
#33399 = DIRECTION ( 'NONE',  ( 0.000000000000000000, 1.000000000000000000, 0.000000000000000000 ) ) ;
#33400 = DIRECTION ( 'NONE',  ( -0.000000000000000000, 1.000000000000000000, -0.000000000000000000 ) ) ;
#33401 = CARTESIAN_POINT ( 'NONE',  ( 12.29999999999990479, 12.50000000000000000, -3.983716857408426293 ) ) ;
#33402 =( NAMED_UNIT ( * ) PLANE_ANGLE_UNIT ( ) SI_UNIT ( $, .RADIAN. ) );
#33404 = AXIS2_PLACEMENT_3D ( 'NONE', #52790, #107028, #15425 ) ;
#33403 = AXIS2_PLACEMENT_3D ( 'NONE', #125355, #45523, #83515 ) ;
#33405 = DIRECTION ( 'NONE',  ( -0.000000000000000000, -1.000000000000000000, -0.000000000000000000 ) ) ;
#33406 = DIRECTION ( 'NONE',  ( 0.000000000000000000, 0.000000000000000000, 1.000000000000000000 ) ) ;
#33407 = FACE_OUTER_BOUND ( 'NONE', #5592, .T. ) ;
#33408 = DIRECTION ( 'NONE',  ( 0.000000000000000000, 0.000000000000000000, 1.000000000000000000 ) ) ;
#33409 = CARTESIAN_POINT ( 'NONE',  ( 1.049999999999954969, 2.500000000000000000, -6.741600689897077281 ) ) ;
#33410 = AXIS2_PLACEMENT_3D ( 'NONE', #84696, #52653, #92590 ) ;
#33411 = PLANE ( 'NONE',  #58206 ) ;
#33413 = AXIS2_PLACEMENT_3D ( 'NONE', #91736, #121190, #11227 ) ;
#33412 = CIRCLE ( 'NONE', #106541, 0.06509327318403745899 ) ;
#33414 = ORIENTED_EDGE ( 'NONE', *, *, #104583, .T. ) ;
#33415 = CARTESIAN_POINT ( 'NONE',  ( -6.850000000000013856, 12.50000000000000000, 6.148780366869520897 ) ) ;
#33416 = VERTEX_POINT ( 'NONE', #37331 ) ;
#33417 = ORIENTED_EDGE ( 'NONE', *, *, #66418, .F. ) ;
#33418 = CARTESIAN_POINT ( 'NONE',  ( 3.749999999999944045, 12.50000000000000000, -7.253104124594891289 ) ) ;
#33419 = DIRECTION ( 'NONE',  ( -4.274815082592931898E-19, -0.9999939076577903929, -0.003490651415223739937 ) ) ;
#33420 = CARTESIAN_POINT ( 'NONE',  ( -6.650000000000019007, 2.500000000000000000, -1.472243186433550122 ) ) ;
#33421 = EDGE_CURVE ( 'NONE', #115634, #77218, #108981, .T. ) ;
#33422 = DIRECTION ( 'NONE',  ( -0.000000000000000000, 0.000000000000000000, -1.000000000000000000 ) ) ;
#33423 = CARTESIAN_POINT ( 'NONE',  ( -10.40000000000000213, 2.500000000000000000, 0.09999999999999772959 ) ) ;
#33424 = DIRECTION ( 'NONE',  ( -4.274815082592931898E-19, -0.9999939076577903929, -0.003490651415223739937 ) ) ;
#33425 = CARTESIAN_POINT ( 'NONE',  ( -8.750000000000008882, 12.50000000000000000, 1.472243186433545459 ) ) ;
#33426 = ORIENTED_EDGE ( 'NONE', *, *, #11738, .T. ) ;
#33427 = DIRECTION ( 'NONE',  ( -0.000000000000000000, -1.000000000000000000, -0.000000000000000000 ) ) ;
#33428 = DIRECTION ( 'NONE',  ( 0.000000000000000000, 0.000000000000000000, 1.000000000000000000 ) ) ;
#33429 = VERTEX_POINT ( 'NONE', #117136 ) ;
#33430 = AXIS2_PLACEMENT_3D ( 'NONE', #54520, #23140, #74178 ) ;
#33432 = ORIENTED_EDGE ( 'NONE', *, *, #89424, .F. ) ;
#33431 = AXIS2_PLACEMENT_3D ( 'NONE', #28599, #116954, #38434 ) ;
#33433 = ORIENTED_EDGE ( 'NONE', *, *, #66831, .T. ) ;
#33434 = EDGE_CURVE ( 'NONE', #75499, #129204, #113190, .T. ) ;
#33436 = VERTEX_POINT ( 'NONE', #75298 ) ;
#33435 = EDGE_CURVE ( 'NONE', #117286, #72026, #88131, .T. ) ;
#33437 = DIRECTION ( 'NONE',  ( 0.000000000000000000, 1.000000000000000000, 0.000000000000000000 ) ) ;
#33438 = DIRECTION ( 'NONE',  ( 0.000000000000000000, 0.000000000000000000, -1.000000000000000000 ) ) ;
#33440 = AXIS2_PLACEMENT_3D ( 'NONE', #119192, #50445, #9882 ) ;
#33439 = CIRCLE ( 'NONE', #6209, 0.1000000000000000472 ) ;
#33441 = DIRECTION ( 'NONE',  ( -0.000000000000000000, -1.000000000000000000, -0.000000000000000000 ) ) ;
#33442 = DIRECTION ( 'NONE',  ( -0.000000000000000000, -1.000000000000000000, -0.000000000000000000 ) ) ;
#33443 = DIRECTION ( 'NONE',  ( 0.000000000000000000, 0.000000000000000000, -1.000000000000000000 ) ) ;
#33444 = ORIENTED_EDGE ( 'NONE', *, *, #22473, .F. ) ;
#33445 = LINE ( 'NONE', #114550, #99613 ) ;
#33446 = ADVANCED_FACE ( 'NONE', ( #115195 ), #45850, .F. ) ;
#33447 = CARTESIAN_POINT ( 'NONE',  ( -2.300000000000033573, 2.500000000000000000, 0.3464101615137735735 ) ) ;
#33448 = CARTESIAN_POINT ( 'NONE',  ( -8.100000000000010303, 2.500000000000000000, 4.776537180435972196 ) ) ;
#33449 = CARTESIAN_POINT ( 'NONE',  ( 187.1562500006828316, 8.891194145520236347, 5.444286225454521982E-16 ) ) ;
#33450 = CIRCLE ( 'NONE', #85657, 0.09999999999999982514 ) ;
#33451 = EDGE_LOOP ( 'NONE', ( #23721, #35786, #107268, #50136 ) ) ;
#33452 = AXIS2_PLACEMENT_3D ( 'NONE', #53112, #55678, #64206 ) ;
#33453 = VERTEX_POINT ( 'NONE', #70007 ) ;
#33454 = ORIENTED_EDGE ( 'NONE', *, *, #92132, .F. ) ;
#33455 = FACE_OUTER_BOUND ( 'NONE', #114301, .T. ) ;
#33456 = VECTOR ( 'NONE', #58332, 1000.000000000000000 ) ;
#33457 = AXIS2_PLACEMENT_3D ( 'NONE', #45680, #86217, #46972 ) ;
#33458 = CARTESIAN_POINT ( 'NONE',  ( 7.099999999999927702, 2.500000000000000000, 5.122947341949749323 ) ) ;
#33459 = DIRECTION ( 'NONE',  ( 0.000000000000000000, 1.000000000000000000, 0.000000000000000000 ) ) ;
#33460 = CONICAL_SURFACE ( 'NONE', #119218, 0.1000000000000002554, 0.003490658503988666988 ) ;
#33461 = ORIENTED_EDGE ( 'NONE', *, *, #7085, .T. ) ;
#33462 = LINE ( 'NONE', #22357, #101745 ) ;
#33463 = LINE ( 'NONE', #104122, #20407 ) ;
#33464 = FACE_OUTER_BOUND ( 'NONE', #25258, .T. ) ;
#33465 = DIRECTION ( 'NONE',  ( -4.274815082592931898E-19, -0.9999939076577903929, -0.003490651415223739937 ) ) ;
#33466 = ADVANCED_FACE ( 'NONE', ( #79190 ), #119730, .T. ) ;
#33467 = CARTESIAN_POINT ( 'NONE',  ( 11.24999999999994316, 12.50000000000000000, -6.495190528383302464 ) ) ;
#33468 = VERTEX_POINT ( 'NONE', #28794 ) ;
#33469 = VERTEX_POINT ( 'NONE', #68701 ) ;
#33470 = ADVANCED_FACE ( 'NONE', ( #99472 ), #83947, .T. ) ;
#33471 = CARTESIAN_POINT ( 'NONE',  ( 0.5999999999999547917, 2.500000000000000000, 4.083716857408420609 ) ) ;
#33472 = CARTESIAN_POINT ( 'NONE',  ( -13.74999999999998934, 12.50000000000000000, 2.857883832488652853 ) ) ;
#33473 = ADVANCED_FACE ( 'NONE', ( #18308 ), #119452, .T. ) ;
#33474 = DIRECTION ( 'NONE',  ( -0.000000000000000000, 1.000000000000000000, -0.000000000000000000 ) ) ;
#33475 = PLANE ( 'NONE',  #63222 ) ;
#33476 = DIRECTION ( 'NONE',  ( 0.000000000000000000, 0.000000000000000000, -1.000000000000000000 ) ) ;
#33477 = ORIENTED_EDGE ( 'NONE', *, *, #82971, .F. ) ;
#33478 = EDGE_CURVE ( 'NONE', #37568, #76503, #123646, .T. ) ;
#33479 = EDGE_CURVE ( 'NONE', #48393, #29366, #48452, .T. ) ;
#33480 = VERTEX_POINT ( 'NONE', #10428 ) ;
#33482 = AXIS2_PLACEMENT_3D ( 'NONE', #47716, #69261, #120319 ) ;
#33481 = CARTESIAN_POINT ( 'NONE',  ( -4.600000000000024514, 2.500000000000000000, 5.022947341949748790 ) ) ;
#33483 = DIRECTION ( 'NONE',  ( 0.000000000000000000, 1.000000000000000000, 0.000000000000000000 ) ) ;
#33484 = EDGE_CURVE ( 'NONE', #126271, #98359, #98798, .T. ) ;
#33485 = DIRECTION ( 'NONE',  ( 0.000000000000000000, 1.000000000000000000, 0.000000000000000000 ) ) ;
#33486 = LINE ( 'NONE', #15586, #64375 ) ;
#33487 = CARTESIAN_POINT ( 'NONE',  ( -5.850000000000022737, 2.500000000000000000, -2.065063509461102065 ) ) ;
#33488 = ORIENTED_EDGE ( 'NONE', *, *, #55189, .F. ) ;
#33489 = PLANE ( 'NONE',  #2966 ) ;
#33492 = EDGE_CURVE ( 'NONE', #116919, #22551, #29437, .T. ) ;
#33491 = CIRCLE ( 'NONE', #106628, 0.09999999999999982514 ) ;
#33490 = CIRCLE ( 'NONE', #85780, 0.06509327318403741736 ) ;
#33493 = DIRECTION ( 'NONE',  ( 0.000000000000000000, 0.000000000000000000, 1.000000000000000000 ) ) ;
#33494 = EDGE_LOOP ( 'NONE', ( #68866, #32905 ) ) ;
#33495 = DIRECTION ( 'NONE',  ( 0.000000000000000000, 0.000000000000000000, 1.000000000000000000 ) ) ;
#33496 = ORIENTED_EDGE ( 'NONE', *, *, #7799, .F. ) ;
#33497 = EDGE_CURVE ( 'NONE', #19146, #125479, #52565, .T. ) ;
#33498 = FACE_OUTER_BOUND ( 'NONE', #106778, .T. ) ;
#33499 = CIRCLE ( 'NONE', #8337, 0.06509327318403745899 ) ;
#33500 = ORIENTED_EDGE ( 'NONE', *, *, #114910, .T. ) ;
#33501 = CARTESIAN_POINT ( 'NONE',  ( 5.599999999999934808, 12.50000000000000000, -3.983716857408426293 ) ) ;
#33502 = FACE_OUTER_BOUND ( 'NONE', #38657, .T. ) ;
#33503 = ORIENTED_EDGE ( 'NONE', *, *, #127988, .T. ) ;
#33504 = ORIENTED_EDGE ( 'NONE', *, *, #27658, .F. ) ;
#33505 = CARTESIAN_POINT ( 'NONE',  ( 184.9218750003414016, 0.000000000000000000, 7.564683531250000925 ) ) ;
#33506 = FACE_OUTER_BOUND ( 'NONE', #31939, .T. ) ;
#33507 = CARTESIAN_POINT ( 'NONE',  ( 186.3385416670080872, 6.551208109652274736, 3.782341765625001351 ) ) ;
#33508 = CARTESIAN_POINT ( 'NONE',  ( 185.9427083336747160, -6.551208109652278289, 3.782341765624995134 ) ) ;
#33509 = DIRECTION ( 'NONE',  ( 0.000000000000000000, 0.000000000000000000, 1.000000000000000000 ) ) ;
#33510 = DIRECTION ( 'NONE',  ( -0.000000000000000000, 1.000000000000000000, -0.000000000000000000 ) ) ;
#33511 = DIRECTION ( 'NONE',  ( 0.000000000000000000, -0.000000000000000000, 1.000000000000000000 ) ) ;
#33512 = LINE ( 'NONE', #80676, #127906 ) ;
#33513 = CIRCLE ( 'NONE', #12648, 0.06509327318403745899 ) ;
#33514 = AXIS2_PLACEMENT_3D ( 'NONE', #63792, #25136, #65048 ) ;
#33515 = ORIENTED_EDGE ( 'NONE', *, *, #115871, .T. ) ;
#33516 = EDGE_LOOP ( 'NONE', ( #38244, #110882, #76451, #23820 ) ) ;
#33517 = DIRECTION ( 'NONE',  ( 0.000000000000000000, -0.9999939076577903929, 0.003490651415223739937 ) ) ;
#33518 = ORIENTED_EDGE ( 'NONE', *, *, #71669, .T. ) ;
#33519 = DIRECTION ( 'NONE',  ( 0.000000000000000000, 0.000000000000000000, 1.000000000000000000 ) ) ;
#33520 = CARTESIAN_POINT ( 'NONE',  ( -1.850000000000033840, 12.50000000000000000, 1.883746621131358934 ) ) ;
#33521 = DIRECTION ( 'NONE',  ( -4.274815082592931898E-19, -0.9999939076577903929, -0.003490651415223739937 ) ) ;
#33523 = VERTEX_POINT ( 'NONE', #87691 ) ;
#33522 = ORIENTED_EDGE ( 'NONE', *, *, #16974, .F. ) ;
#33524 = FACE_BOUND ( 'NONE', #115516, .T. ) ;
#33525 = ORIENTED_EDGE ( 'NONE', *, *, #73303, .T. ) ;
#33526 = DIRECTION ( 'NONE',  ( 0.000000000000000000, 0.000000000000000000, 1.000000000000000000 ) ) ;
#33527 = LINE ( 'NONE', #53790, #104482 ) ;
#33528 = AXIS2_PLACEMENT_3D ( 'NONE', #24120, #64041, #103971 ) ;
#33529 = FACE_OUTER_BOUND ( 'NONE', #125506, .T. ) ;
#33530 = DIRECTION ( 'NONE',  ( -0.000000000000000000, 1.000000000000000000, -0.000000000000000000 ) ) ;
#33531 = EDGE_CURVE ( 'NONE', #109159, #69422, #125701, .T. ) ;
#33532 = CARTESIAN_POINT ( 'NONE',  ( -8.950000000000008171, 2.500000000000000000, -2.511473670974877948 ) ) ;
#33533 = CARTESIAN_POINT ( 'NONE',  ( 2.499999999999947153, 12.50000000000000000, 0.6928203230275494784 ) ) ;
#33534 = DIRECTION ( 'NONE',  ( -0.000000000000000000, 1.000000000000000000, -0.000000000000000000 ) ) ;
#33535 = CARTESIAN_POINT ( 'NONE',  ( 187.5000000000000000, 9.429780353434619030E-16, -7.700000000000000178 ) ) ;
#33536 = CARTESIAN_POINT ( 'NONE',  ( 4.149999999999938183, 2.500000000000000000, 5.702370205355745014 ) ) ;
#33537 = DIRECTION ( 'NONE',  ( 0.000000000000000000, 0.000000000000000000, -1.000000000000000000 ) ) ;
#33538 = AXIS2_PLACEMENT_3D ( 'NONE', #70509, #51536, #43025 ) ;
#33539 = DIRECTION ( 'NONE',  ( -0.000000000000000000, 1.000000000000000000, -0.000000000000000000 ) ) ;
#33540 = EDGE_CURVE ( 'NONE', #55389, #56667, #109269, .T. ) ;
#33541 = CONICAL_SURFACE ( 'NONE', #123399, 0.09999999999999982514, 0.003490658503988666988 ) ;
#33542 = ORIENTED_EDGE ( 'NONE', *, *, #99780, .T. ) ;
#33543 = ORIENTED_EDGE ( 'NONE', *, *, #7721, .T. ) ;
#33544 = VECTOR ( 'NONE', #26065, 1000.000000000000000 ) ;
#33545 = ORIENTED_EDGE ( 'NONE', *, *, #96812, .T. ) ;
#33546 = DIRECTION ( 'NONE',  ( 0.000000000000000000, 1.000000000000000000, 0.000000000000000000 ) ) ;
#33547 = EDGE_LOOP ( 'NONE', ( #56693, #85440, #112923, #114681 ) ) ;
#33548 = LINE ( 'NONE', #45776, #67439 ) ;
#33550 = VERTEX_POINT ( 'NONE', #97515 ) ;
#33549 = ORIENTED_EDGE ( 'NONE', *, *, #104056, .F. ) ;
#33551 = ORIENTED_EDGE ( 'NONE', *, *, #26493, .T. ) ;
#33552 = DIRECTION ( 'NONE',  ( 0.000000000000000000, 0.000000000000000000, 1.000000000000000000 ) ) ;
#33553 = VECTOR ( 'NONE', #55670, 1000.000000000000000 ) ;
#33554 = FACE_OUTER_BOUND ( 'NONE', #53552, .T. ) ;
#33555 = DIRECTION ( 'NONE',  ( 0.000000000000000000, 0.000000000000000000, -1.000000000000000000 ) ) ;
#33556 = AXIS2_PLACEMENT_3D ( 'NONE', #630, #51051, #40602 ) ;
#33557 = LINE ( 'NONE', #53822, #74859 ) ;
#33558 = CARTESIAN_POINT ( 'NONE',  ( 9.149999999999920419, 2.500000000000000000, 2.857883832488649301 ) ) ;
#33559 = ORIENTED_EDGE ( 'NONE', *, *, #68202, .T. ) ;
#33560 = DIRECTION ( 'NONE',  ( -0.000000000000000000, 1.000000000000000000, -0.000000000000000000 ) ) ;
#33561 = ORIENTED_EDGE ( 'NONE', *, *, #54930, .F. ) ;
#33562 = EDGE_LOOP ( 'NONE', ( #120291, #124667, #73285, #26592 ) ) ;
#33563 = ORIENTED_EDGE ( 'NONE', *, *, #68480, .T. ) ;
#33564 = DIRECTION ( 'NONE',  ( 0.000000000000000000, 1.000000000000000000, 0.000000000000000000 ) ) ;
#33565 = ORIENTED_EDGE ( 'NONE', *, *, #19870, .T. ) ;
#33566 = EDGE_LOOP ( 'NONE', ( #68091, #70742 ) ) ;
#33567 = VERTEX_POINT ( 'NONE', #110563 ) ;
#33568 = CARTESIAN_POINT ( 'NONE',  ( -1.450000000000036371, 2.500000000000000000, 6.941600689897073018 ) ) ;
#33569 = ADVANCED_FACE ( 'NONE', ( #58257 ), #96463, .T. ) ;
#33570 = DIRECTION ( 'NONE',  ( 0.000000000000000000, -0.9999939076577903929, 0.003490651415223739937 ) ) ;
#33571 = DIRECTION ( 'NONE',  ( 0.000000000000000000, -0.000000000000000000, 1.000000000000000000 ) ) ;
#33572 = CARTESIAN_POINT ( 'NONE',  ( -5.400000000000023448, 2.500000000000000000, -5.022947341949754119 ) ) ;
#33573 = DIRECTION ( 'NONE',  ( 0.000000000000000000, 0.000000000000000000, -1.000000000000000000 ) ) ;
#33574 = CIRCLE ( 'NONE', #94109, 0.06509327318403745899 ) ;
#33575 = DIRECTION ( 'NONE',  ( 0.000000000000000000, 1.000000000000000000, 0.000000000000000000 ) ) ;
#33576 = CONICAL_SURFACE ( 'NONE', #48143, 0.09999999999999982514, 0.003490658503988666988 ) ;
#33577 = DIRECTION ( 'NONE',  ( 0.000000000000000000, 1.000000000000000000, 0.000000000000000000 ) ) ;
#33578 = ADVANCED_FACE ( 'NONE', ( #20254 ), #75537, .T. ) ;
#33579 = EDGE_LOOP ( 'NONE', ( #39934, #24717 ) ) ;
#33580 = CARTESIAN_POINT ( 'NONE',  ( 11.44999999999991047, 2.500000000000000000, 6.048780366869520364 ) ) ;
#33581 = AXIS2_PLACEMENT_3D ( 'NONE', #11378, #12018, #259 ) ;
#33582 = ORIENTED_EDGE ( 'NONE', *, *, #8577, .T. ) ;
#33583 = CARTESIAN_POINT ( 'NONE',  ( -1.850000000000033840, 12.50000000000000000, 6.148780366869520897 ) ) ;
#33584 = VERTEX_POINT ( 'NONE', #68056 ) ;
#33585 = EDGE_CURVE ( 'NONE', #32548, #63751, #129590, .T. ) ;
#33586 = EDGE_CURVE ( 'NONE', #100700, #37856, #104871, .T. ) ;
#33587 = ORIENTED_EDGE ( 'NONE', *, *, #41637, .F. ) ;
#33588 = DIRECTION ( 'NONE',  ( 0.000000000000000000, 0.000000000000000000, 1.000000000000000000 ) ) ;
#33589 = DIRECTION ( 'NONE',  ( 0.000000000000000000, 0.000000000000000000, -1.000000000000000000 ) ) ;
#33590 = ADVANCED_FACE ( 'NONE', ( #77868 ), #94412, .T. ) ;
#33591 = DIRECTION ( 'NONE',  ( -0.000000000000000000, 1.000000000000000000, -0.000000000000000000 ) ) ;
#33592 = EDGE_LOOP ( 'NONE', ( #103117, #91828 ) ) ;
#33593 = EDGE_LOOP ( 'NONE', ( #74915, #51920 ) ) ;
#33594 = CARTESIAN_POINT ( 'NONE',  ( -12.89999999999999147, 12.50000000000000000, 1.843143693225357538E-15 ) ) ;
#33595 = CARTESIAN_POINT ( 'NONE',  ( 2.500000000000002220, -0.5000000000000000000, -9.999999999999998224 ) ) ;
#33596 = ADVANCED_FACE ( 'NONE', ( #128289 ), #14965, .T. ) ;
#33597 = DIRECTION ( 'NONE',  ( 0.000000000000000000, 1.000000000000000000, 0.000000000000000000 ) ) ;
#33598 = DIRECTION ( 'NONE',  ( -0.000000000000000000, -1.000000000000000000, -0.000000000000000000 ) ) ;
#33599 = DIRECTION ( 'NONE',  ( 0.000000000000000000, 1.000000000000000000, 0.000000000000000000 ) ) ;
#33600 = ORIENTED_EDGE ( 'NONE', *, *, #44319, .T. ) ;
#33601 = ORIENTED_EDGE ( 'NONE', *, *, #103920, .T. ) ;
#33602 = DIRECTION ( 'NONE',  ( 0.000000000000000000, 1.000000000000000000, 0.000000000000000000 ) ) ;
#33603 = CIRCLE ( 'NONE', #106735, 0.1000000000000002554 ) ;
#33604 = FACE_OUTER_BOUND ( 'NONE', #4357, .T. ) ;
#33605 = VECTOR ( 'NONE', #41788, 1000.000000000000000 ) ;
#33606 = CARTESIAN_POINT ( 'NONE',  ( 186.9166666666666856, 6.668395609140176816, 3.850000000000000977 ) ) ;
#33607 = DIRECTION ( 'NONE',  ( -0.000000000000000000, 1.000000000000000000, -0.000000000000000000 ) ) ;
#33608 = FACE_OUTER_BOUND ( 'NONE', #12244, .T. ) ;
#33609 = DIRECTION ( 'NONE',  ( 0.000000000000000000, 1.000000000000000000, 0.000000000000000000 ) ) ;
#33610 = DIRECTION ( 'NONE',  ( -0.000000000000000000, -1.000000000000000000, -0.000000000000000000 ) ) ;
#33611 = ORIENTED_EDGE ( 'NONE', *, *, #20141, .F. ) ;
#33612 = AXIS2_PLACEMENT_3D ( 'NONE', #8968, #48924, #88828 ) ;
#33613 = CARTESIAN_POINT ( 'NONE',  ( 6.449999999999931788, 12.50000000000000000, -2.576566944158915184 ) ) ;
#33614 = ADVANCED_FACE ( 'NONE', ( #71947 ), #111193, .T. ) ;
#33615 = CARTESIAN_POINT ( 'NONE',  ( -4.600000000000025402, 2.500000000000000000, 4.230127018922196669 ) ) ;
#33616 = CARTESIAN_POINT ( 'NONE',  ( 10.44999999999991047, 2.500000000000000000, 2.165063509461097713 ) ) ;
#33617 = ORIENTED_EDGE ( 'NONE', *, *, #60539, .T. ) ;
#33618 = EDGE_CURVE ( 'NONE', #118696, #62991, #92261, .T. ) ;
#33619 = DIRECTION ( 'NONE',  ( 0.000000000000000000, 1.000000000000000000, 0.000000000000000000 ) ) ;
#33620 = CONICAL_SURFACE ( 'NONE', #16854, 0.1000000000000002554, 0.003490658503988666988 ) ;
#33621 = ORIENTED_EDGE ( 'NONE', *, *, #39935, .F. ) ;
#33622 = PRODUCT ( 'Brush Head Assembly', 'Brush Head Assembly', '', ( #26784 ) ) ;
#33623 = DIRECTION ( 'NONE',  ( 0.000000000000000000, 1.000000000000000000, 0.000000000000000000 ) ) ;
#33624 = EDGE_CURVE ( 'NONE', #40211, #59797, #35847, .T. ) ;
#33625 = ORIENTED_EDGE ( 'NONE', *, *, #45133, .F. ) ;
#33626 = DIRECTION ( 'NONE',  ( 0.000000000000000000, -0.000000000000000000, 1.000000000000000000 ) ) ;
#33627 = DIRECTION ( 'NONE',  ( 0.000000000000000000, 0.000000000000000000, 1.000000000000000000 ) ) ;
#33628 = EDGE_CURVE ( 'NONE', #129270, #77431, #17014, .T. ) ;
#33629 = PLANE ( 'NONE',  #84093 ) ;
#33631 = ADVANCED_FACE ( 'NONE', ( #83055 ), #12826, .T. ) ;
#33630 = AXIS2_PLACEMENT_3D ( 'NONE', #37815, #69859, #18811 ) ;
#33632 = ORIENTED_EDGE ( 'NONE', *, *, #35070, .T. ) ;
#33633 = LINE ( 'NONE', #113471, #76028 ) ;
#33634 = ADVANCED_FACE ( 'NONE', ( #111866 ), #85994, .T. ) ;
#33635 = DIRECTION ( 'NONE',  ( -0.000000000000000000, 1.000000000000000000, -0.000000000000000000 ) ) ;
#33636 = CIRCLE ( 'NONE', #121355, 0.06509327318403745899 ) ;
#33637 = VERTEX_POINT ( 'NONE', #32028 ) ;
#33638 = ADVANCED_FACE ( 'NONE', ( #63404 ), #113797, .T. ) ;
#33639 = ADVANCED_FACE ( 'NONE', ( #60828 ), #21258, .T. ) ;
#33640 = EDGE_LOOP ( 'NONE', ( #975, #46832 ) ) ;
#33641 = VERTEX_POINT ( 'NONE', #72587 ) ;
#33642 = DIRECTION ( 'NONE',  ( -0.000000000000000000, -1.000000000000000000, -0.000000000000000000 ) ) ;
#33643 = FACE_OUTER_BOUND ( 'NONE', #33579, .T. ) ;
#33644 = DIRECTION ( 'NONE',  ( 0.000000000000000000, 1.000000000000000000, 0.000000000000000000 ) ) ;
#33645 = ORIENTED_EDGE ( 'NONE', *, *, #80297, .T. ) ;
#33646 = FACE_OUTER_BOUND ( 'NONE', #2266, .T. ) ;
#33647 = DIRECTION ( 'NONE',  ( 0.000000000000000000, 0.000000000000000000, -1.000000000000000000 ) ) ;
#33648 = ORIENTED_EDGE ( 'NONE', *, *, #47928, .F. ) ;
#33649 = DIRECTION ( 'NONE',  ( 0.000000000000000000, 0.000000000000000000, 1.000000000000000000 ) ) ;
#33650 = CARTESIAN_POINT ( 'NONE',  ( -1.250000000000035749, 2.500000000000000000, -2.957883832488653830 ) ) ;
#33652 = DIRECTION ( 'NONE',  ( -0.000000000000000000, -1.000000000000000000, -0.000000000000000000 ) ) ;
#33651 = VECTOR ( 'NONE', #94246, 1000.000000000000000 ) ;
#33653 = CARTESIAN_POINT ( 'NONE',  ( 187.5000000000000000, 0.000000000000000000, 0.000000000000000000 ) ) ;
#33654 = DIRECTION ( 'NONE',  ( 0.000000000000000000, -0.000000000000000000, 1.000000000000000000 ) ) ;
#33655 = CIRCLE ( 'NONE', #123523, 0.1000000000000002554 ) ;
#33656 = AXIS2_PLACEMENT_3D ( 'NONE', #39699, #79594, #119504 ) ;
#33657 = DIRECTION ( 'NONE',  ( 0.000000000000000000, 0.000000000000000000, 1.000000000000000000 ) ) ;
#33658 = DIRECTION ( 'NONE',  ( 0.000000000000000000, 0.000000000000000000, -1.000000000000000000 ) ) ;
#33659 = AXIS2_PLACEMENT_3D ( 'NONE', #38786, #100885, #91075 ) ;
#33660 = ORIENTED_EDGE ( 'NONE', *, *, #10409, .F. ) ;
#33661 = ORIENTED_EDGE ( 'NONE', *, *, #23881, .T. ) ;
#33662 = ORIENTED_EDGE ( 'NONE', *, *, #41680, .F. ) ;
#33663 = VERTEX_POINT ( 'NONE', #22856 ) ;
#33664 = CARTESIAN_POINT ( 'NONE',  ( 3.949999999999941558, 2.500000000000000000, -1.718653347947326049 ) ) ;
#33665 = CARTESIAN_POINT ( 'NONE',  ( 0.6499999999999561684, 12.50000000000000000, 1.818653347947321475 ) ) ;
#33666 = AXIS2_PLACEMENT_3D ( 'NONE', #53354, #21296, #12750 ) ;
#33667 = DIRECTION ( 'NONE',  ( -4.274815082592931898E-19, -0.9999939076577903929, -0.003490651415223739937 ) ) ;
#33668 = ORIENTED_EDGE ( 'NONE', *, *, #123557, .T. ) ;
#33669 = FACE_BOUND ( 'NONE', #84031, .T. ) ;
#33670 = DIRECTION ( 'NONE',  ( -0.000000000000000000, -1.000000000000000000, -0.000000000000000000 ) ) ;
#33671 = CARTESIAN_POINT ( 'NONE',  ( 3.549999999999942979, 12.50000000000000000, 1.883746621131358934 ) ) ;
#33672 = CARTESIAN_POINT ( 'NONE',  ( 10.59999999999991260, 12.50000000000000000, -0.3464101615137783474 ) ) ;
#33673 = ADVANCED_FACE ( 'NONE', ( #62768 ), #50503, .T. ) ;
#33674 = CARTESIAN_POINT ( 'NONE',  ( 8.349999999999923261, 2.500000000000000000, -5.802370205355749988 ) ) ;
#33675 = PLANE ( 'NONE',  #32631 ) ;
#33676 = DIRECTION ( 'NONE',  ( 0.000000000000000000, 0.000000000000000000, 1.000000000000000000 ) ) ;
#33677 = FACE_OUTER_BOUND ( 'NONE', #41190, .T. ) ;
#33678 = CARTESIAN_POINT ( 'NONE',  ( -1.850000000000033840, 12.50000000000000000, 6.148780366869520897 ) ) ;
#33679 = CARTESIAN_POINT ( 'NONE',  ( 14.34999999999989662, 12.50000000000000000, 2.446380397790835826 ) ) ;
#33680 = FACE_OUTER_BOUND ( 'NONE', #44230, .T. ) ;
#33681 = EDGE_LOOP ( 'NONE', ( #122256, #103792, #30286, #24965 ) ) ;
#33682 = EDGE_CURVE ( 'NONE', #102865, #85037, #106930, .T. ) ;
#33683 = AXIS2_PLACEMENT_3D ( 'NONE', #37246, #88231, #106604 ) ;
#33684 = ORIENTED_EDGE ( 'NONE', *, *, #68210, .F. ) ;
#33685 = ORIENTED_EDGE ( 'NONE', *, *, #68890, .F. ) ;
#33686 = ORIENTED_EDGE ( 'NONE', *, *, #28330, .F. ) ;
#33687 = ORIENTED_EDGE ( 'NONE', *, *, #37719, .T. ) ;
#33688 = ORIENTED_EDGE ( 'NONE', *, *, #31412, .T. ) ;
#33689 = DIRECTION ( 'NONE',  ( 0.000000000000000000, 0.000000000000000000, -1.000000000000000000 ) ) ;
#33690 = EDGE_LOOP ( 'NONE', ( #23147, #53986 ) ) ;
#33691 = VERTEX_POINT ( 'NONE', #51664 ) ;
#33692 = AXIS2_PLACEMENT_3D ( 'NONE', #21516, #90231, #80442 ) ;
#33693 = CARTESIAN_POINT ( 'NONE',  ( 15.40585131749378967, -2.500000000000000444, 5.817868756321115775 ) ) ;
#33694 = DIRECTION ( 'NONE',  ( -0.000000000000000000, 1.000000000000000000, -0.000000000000000000 ) ) ;
#33695 = FACE_OUTER_BOUND ( 'NONE', #10719, .T. ) ;
#33696 = VERTEX_POINT ( 'NONE', #102671 ) ;
#33697 = CARTESIAN_POINT ( 'NONE',  ( -6.450000000000017941, 2.500000000000000000, -6.841600689897077814 ) ) ;
#33698 = AXIS2_PLACEMENT_3D ( 'NONE', #20530, #30362, #71548 ) ;
#33699 = ORIENTED_EDGE ( 'NONE', *, *, #126795, .T. ) ;
#33700 = EDGE_LOOP ( 'NONE', ( #119316, #119799 ) ) ;
#33701 = DIRECTION ( 'NONE',  ( 0.000000000000000000, 1.000000000000000000, 0.000000000000000000 ) ) ;
#33702 = LINE ( 'NONE', #73615, #83917 ) ;
#33703 = ORIENTED_EDGE ( 'NONE', *, *, #118878, .F. ) ;
#33704 = ORIENTED_EDGE ( 'NONE', *, *, #41419, .T. ) ;
#33705 = CIRCLE ( 'NONE', #60891, 0.06509327318403745899 ) ;
#33706 = CARTESIAN_POINT ( 'NONE',  ( 129.5000000000000000, 0.000000000000000000, 0.000000000000000000 ) ) ;
#33707 = VECTOR ( 'NONE', #37018, 1000.000000000000000 ) ;
#33708 = PLANE ( 'NONE',  #101805 ) ;
#33709 = CARTESIAN_POINT ( 'NONE',  ( 7.949999999999922018, 2.500000000000000000, 6.495190528383297135 ) ) ;
#33710 = DIRECTION ( 'NONE',  ( 0.000000000000000000, -0.000000000000000000, -1.000000000000000000 ) ) ;
#33711 = DIRECTION ( 'NONE',  ( 0.000000000000000000, 0.000000000000000000, 1.000000000000000000 ) ) ;
#33712 = CIRCLE ( 'NONE', #106853, 0.06509327318403743123 ) ;
#33713 = ORIENTED_EDGE ( 'NONE', *, *, #99772, .F. ) ;
#33714 = FACE_OUTER_BOUND ( 'NONE', #88250, .T. ) ;
#33715 = ADVANCED_FACE ( 'NONE', ( #12988 ), #52941, .T. ) ;
#33716 = ORIENTED_EDGE ( 'NONE', *, *, #103507, .F. ) ;
#33717 = CARTESIAN_POINT ( 'NONE',  ( 17.50000000000000000, 2.499999999999999556, 1.666666666666669849 ) ) ;
#33718 = ORIENTED_EDGE ( 'NONE', *, *, #28255, .T. ) ;
#33719 = DIRECTION ( 'NONE',  ( -0.000000000000000000, -1.000000000000000000, -0.000000000000000000 ) ) ;
#33720 = CIRCLE ( 'NONE', #83796, 0.1000000000000002554 ) ;
#33721 = AXIS2_PLACEMENT_3D ( 'NONE', #3138, #114363, #13578 ) ;
#33722 = DIRECTION ( 'NONE',  ( 0.000000000000000000, 0.000000000000000000, 1.000000000000000000 ) ) ;
#33724 = EDGE_CURVE ( 'NONE', #11464, #75789, #19187, .T. ) ;
#33723 = DIRECTION ( 'NONE',  ( 0.000000000000000000, 0.000000000000000000, 1.000000000000000000 ) ) ;
#33725 = DIRECTION ( 'NONE',  ( 1.000000000000000000, 0.000000000000000000, 0.000000000000000000 ) ) ;
#33726 = EDGE_CURVE ( 'NONE', #24379, #99999, #73861, .T. ) ;
#33727 = EDGE_LOOP ( 'NONE', ( #91395, #123213, #57864, #95921 ) ) ;
#33728 = EDGE_CURVE ( 'NONE', #74675, #92671, #67284, .T. ) ;
#33729 = CARTESIAN_POINT ( 'NONE',  ( -1.250000000000001110, 12.50000000000000000, -6.560283801567339701 ) ) ;
#33730 = VERTEX_POINT ( 'NONE', #91571 ) ;
#33731 = ADVANCED_FACE ( 'NONE', ( #81740 ), #28406, .T. ) ;
#33732 = ORIENTED_EDGE ( 'NONE', *, *, #53835, .T. ) ;
#33733 = EDGE_LOOP ( 'NONE', ( #64446, #2153 ) ) ;
#33734 = DIRECTION ( 'NONE',  ( 0.000000000000000000, -0.000000000000000000, 1.000000000000000000 ) ) ;
#33735 = DIRECTION ( 'NONE',  ( -0.000000000000000000, -1.000000000000000000, -0.000000000000000000 ) ) ;
#33736 = EDGE_CURVE ( 'NONE', #83877, #14873, #124260, .T. ) ;
#33737 = CARTESIAN_POINT ( 'NONE',  ( 185.0677083336747160, -4.367472073101514418, -7.564683531250002702 ) ) ;
#33738 = DIRECTION ( 'NONE',  ( 0.000000000000000000, -0.000000000000000000, 1.000000000000000000 ) ) ;
#33739 = DIRECTION ( 'NONE',  ( 1.000000000000000000, 0.000000000000000000, 0.000000000000000000 ) ) ;
#33740 = DIRECTION ( 'NONE',  ( 0.000000000000000000, 1.000000000000000000, 0.000000000000000000 ) ) ;
#33741 = AXIS2_PLACEMENT_3D ( 'NONE', #75894, #67330, #16936 ) ;
#33742 = VECTOR ( 'NONE', #68825, 1000.000000000000000 ) ;
#33743 = AXIS2_PLACEMENT_3D ( 'NONE', #47410, #48054, #88613 ) ;
#33744 = ORIENTED_EDGE ( 'NONE', *, *, #25692, .F. ) ;
#33745 = CARTESIAN_POINT ( 'NONE',  ( -1.650000000000034328, 2.500000000000000000, -2.265063509461101798 ) ) ;
#33746 = VECTOR ( 'NONE', #13789, 1000.000000000000000 ) ;
#33747 = AXIS2_PLACEMENT_3D ( 'NONE', #66519, #75691, #25294 ) ;
#33748 = VERTEX_POINT ( 'NONE', #103976 ) ;
#33749 = DIRECTION ( 'NONE',  ( 0.000000000000000000, -0.000000000000000000, 1.000000000000000000 ) ) ;
#33750 = CONICAL_SURFACE ( 'NONE', #115190, 0.1000000000000002554, 0.003490658503988666988 ) ;
#33751 = LINE ( 'NONE', #4266, #74465 ) ;
#33752 = FACE_OUTER_BOUND ( 'NONE', #34322, .T. ) ;
#33753 = DIRECTION ( 'NONE',  ( 0.000000000000000000, 0.000000000000000000, -1.000000000000000000 ) ) ;
#33754 = ORIENTED_EDGE ( 'NONE', *, *, #99567, .T. ) ;
#33755 = CARTESIAN_POINT ( 'NONE',  ( 2.299999999999948752, 2.500000000000000000, 0.2464101615137735679 ) ) ;
#33757 = ORIENTED_EDGE ( 'NONE', *, *, #36573, .T. ) ;
#33756 = DIRECTION ( 'NONE',  ( -0.000000000000000000, -1.000000000000000000, -0.000000000000000000 ) ) ;
#33758 = ORIENTED_EDGE ( 'NONE', *, *, #53586, .T. ) ;
#33759 = DIRECTION ( 'NONE',  ( 0.000000000000000000, 0.000000000000000000, 1.000000000000000000 ) ) ;
#33760 = EDGE_LOOP ( 'NONE', ( #30905, #80490, #110088, #64501 ) ) ;
#33761 = ORIENTED_EDGE ( 'NONE', *, *, #51797, .F. ) ;
#33762 = DIRECTION ( 'NONE',  ( -0.000000000000000000, -1.000000000000000000, -0.000000000000000000 ) ) ;
#33763 = ADVANCED_FACE ( 'NONE', ( #34612 ), #95443, .T. ) ;
#33764 = EDGE_CURVE ( 'NONE', #58977, #77164, #104605, .T. ) ;
#33765 = ORIENTED_EDGE ( 'NONE', *, *, #124792, .T. ) ;
#33766 = CARTESIAN_POINT ( 'NONE',  ( 15.86953761860682910, 2.463355995079617333, -3.896699429476665699 ) ) ;
#33768 = EDGE_CURVE ( 'NONE', #108142, #62304, #65976, .T. ) ;
#33767 = CARTESIAN_POINT ( 'NONE',  ( -4.600000000000024514, 12.50000000000000000, 0.6928203230275494784 ) ) ;
#33769 = LINE ( 'NONE', #4283, #8154 ) ;
#33770 = CIRCLE ( 'NONE', #83936, 0.1000000000000000056 ) ;
#33771 = ORIENTED_EDGE ( 'NONE', *, *, #123260, .F. ) ;
#33772 = ADVANCED_FACE ( 'NONE', ( #96711 ), #44336, .T. ) ;
#33773 = DIRECTION ( 'NONE',  ( 0.000000000000000000, 0.000000000000000000, -1.000000000000000000 ) ) ;
#33775 = ORIENTED_EDGE ( 'NONE', *, *, #16275, .F. ) ;
#33774 = DIRECTION ( 'NONE',  ( 0.000000000000000000, 0.000000000000000000, 1.000000000000000000 ) ) ;
#33776 = ADVANCED_FACE ( 'NONE', ( #124901 ), #98604, .T. ) ;
#33777 = DIRECTION ( 'NONE',  ( -4.274815082592931898E-19, -0.9999939076577903929, -0.003490651415223739937 ) ) ;
#33778 = EDGE_CURVE ( 'NONE', #29034, #67278, #31825, .T. ) ;
#33779 = CARTESIAN_POINT ( 'NONE',  ( 10.59999999999990905, 2.500000000000000000, -4.676537180435978769 ) ) ;
#33780 = EDGE_LOOP ( 'NONE', ( #56773, #124817, #93411, #40649 ) ) ;
#33781 = TOROIDAL_SURFACE ( 'NONE', #12828, 3.500000000000000000, 0.5000000000000000000 ) ;
#33782 = ADVANCED_FACE ( 'NONE', ( #8334 ), #38470, .T. ) ;
#33783 = EDGE_CURVE ( 'NONE', #50249, #124819, #21352, .T. ) ;
#33784 = AXIS2_PLACEMENT_3D ( 'NONE', #27293, #59374, #69813 ) ;
#33785 = ORIENTED_EDGE ( 'NONE', *, *, #14444, .F. ) ;
#33786 = ORIENTED_EDGE ( 'NONE', *, *, #112362, .T. ) ;
#33787 = EDGE_LOOP ( 'NONE', ( #38540, #7121 ) ) ;
#33788 = CARTESIAN_POINT ( 'NONE',  ( 4.149999999999941735, 2.500000000000000000, -1.472243186433550122 ) ) ;
#33789 = CARTESIAN_POINT ( 'NONE',  ( 3.709550432145489740, 2.499999999999999556, 9.999999999907080550 ) ) ;
#33790 = DIRECTION ( 'NONE',  ( -0.000000000000000000, 1.000000000000000000, -0.000000000000000000 ) ) ;
#33791 = FACE_BOUND ( 'NONE', #4132, .T. ) ;
#33792 = EDGE_LOOP ( 'NONE', ( #99049, #72117, #19293, #64945 ) ) ;
#33793 = CARTESIAN_POINT ( 'NONE',  ( 187.3177083336747444, 4.367472073101515306, 7.564683531250000925 ) ) ;
#33794 = EDGE_CURVE ( 'NONE', #97645, #46755, #79034, .T. ) ;
#33795 = CARTESIAN_POINT ( 'NONE',  ( -6.900000000000019007, 2.500000000000000000, -0.4464101615137783252 ) ) ;
#33796 = DIRECTION ( 'NONE',  ( -0.000000000000000000, -1.000000000000000000, -0.000000000000000000 ) ) ;
#33797 = VECTOR ( 'NONE', #92044, 1000.000000000000000 ) ;
#33798 = ORIENTED_EDGE ( 'NONE', *, *, #38536, .F. ) ;
#33799 = CIRCLE ( 'NONE', #75557, 0.1000000000000000472 ) ;
#33800 = DIRECTION ( 'NONE',  ( 0.000000000000000000, 1.000000000000000000, 0.000000000000000000 ) ) ;
#33801 = PLANE ( 'NONE',  #92842 ) ;
#33802 = CARTESIAN_POINT ( 'NONE',  ( 13.29999999999990301, 12.50000000000000000, -4.330127018922201643 ) ) ;
#33803 = CONICAL_SURFACE ( 'NONE', #109005, 0.1000000000000000472, 0.003490658503988666988 ) ;
#33804 = CARTESIAN_POINT ( 'NONE',  ( -4.800000000000028244, 2.500000000000000000, -3.883716857408426648 ) ) ;
#33805 = ORIENTED_EDGE ( 'NONE', *, *, #30758, .F. ) ;
#33806 = AXIS2_PLACEMENT_3D ( 'NONE', #105622, #7394, #125255 ) ;
#33807 = AXIS2_PLACEMENT_3D ( 'NONE', #10219, #51450, #30527 ) ;
#33808 = ORIENTED_EDGE ( 'NONE', *, *, #21646, .T. ) ;
#33809 = ORIENTED_EDGE ( 'NONE', *, *, #39436, .F. ) ;
#33810 = ORIENTED_EDGE ( 'NONE', *, *, #69256, .F. ) ;
#33811 = ORIENTED_EDGE ( 'NONE', *, *, #1527, .F. ) ;
#33812 = CARTESIAN_POINT ( 'NONE',  ( -9.350000000000006750, 12.50000000000000000, 1.818653347947321475 ) ) ;
#33813 = CARTESIAN_POINT ( 'NONE',  ( 11.64999999999990443, 2.500000000000000000, -7.288010851410854585 ) ) ;
#33814 = VERTEX_POINT ( 'NONE', #49573 ) ;
#33815 = FACE_BOUND ( 'NONE', #80859, .T. ) ;
#33816 = CARTESIAN_POINT ( 'NONE',  ( 2.899999999999946620, 12.50000000000000000, -0.6928203230275542523 ) ) ;
#33817 = ORIENTED_EDGE ( 'NONE', *, *, #57256, .T. ) ;
#33818 = DIRECTION ( 'NONE',  ( -0.000000000000000000, 1.000000000000000000, -0.000000000000000000 ) ) ;
#33819 = CARTESIAN_POINT ( 'NONE',  ( 2.299999999999949640, 12.50000000000000000, -4.676537180435977881 ) ) ;
#33820 = FACE_OUTER_BOUND ( 'NONE', #100910, .T. ) ;
#33821 = EDGE_LOOP ( 'NONE', ( #49057, #13272, #1917, #126046 ) ) ;
#33822 = CARTESIAN_POINT ( 'NONE',  ( -11.05000000000000249, 12.50000000000000000, -1.818653347947322141 ) ) ;
#33823 = EDGE_LOOP ( 'NONE', ( #60738, #79566 ) ) ;
#33824 = ADVANCED_FACE ( 'NONE', ( #29928 ), #98699, .T. ) ;
#33825 = ORIENTED_EDGE ( 'NONE', *, *, #121965, .F. ) ;
#33826 = CIRCLE ( 'NONE', #81845, 0.1000000000000000472 ) ;
#33827 = ORIENTED_EDGE ( 'NONE', *, *, #127498, .T. ) ;
#33828 = VECTOR ( 'NONE', #39731, 1000.000000000000000 ) ;
#33829 = CARTESIAN_POINT ( 'NONE',  ( -4.800000000000022915, 2.500000000000000000, 4.083716857408420609 ) ) ;
#33830 = CARTESIAN_POINT ( 'NONE',  ( 5.849999999999933920, 2.500000000000000000, 6.595190528383296780 ) ) ;
#33831 = CARTESIAN_POINT ( 'NONE',  ( -0.2000000000000339284, 2.500000000000000000, -0.2464101615137759549 ) ) ;
#33832 = VERTEX_POINT ( 'NONE', #98005 ) ;
#33833 = DIRECTION ( 'NONE',  ( 0.000000000000000000, 0.000000000000000000, -1.000000000000000000 ) ) ;
#33834 = DIRECTION ( 'NONE',  ( 0.000000000000000000, 0.000000000000000000, 1.000000000000000000 ) ) ;
#33835 = CIRCLE ( 'NONE', #58888, 0.1000000000000002554 ) ;
#33836 = AXIS2_PLACEMENT_3D ( 'NONE', #17076, #57697, #124005 ) ;
#33837 = CARTESIAN_POINT ( 'NONE',  ( -1.450000000000035927, 2.500000000000000000, -6.248780366869526759 ) ) ;
#33838 = CARTESIAN_POINT ( 'NONE',  ( 185.5312500006828031, 9.429780353434619030E-16, -7.700000000000000178 ) ) ;
#33839 = ORIENTED_EDGE ( 'NONE', *, *, #98433, .T. ) ;
#33840 = AXIS2_PLACEMENT_3D ( 'NONE', #52048, #335, #101790 ) ;
#33841 = AXIS2_PLACEMENT_3D ( 'NONE', #122638, #53898, #13308 ) ;
#33842 = FACE_OUTER_BOUND ( 'NONE', #21141, .T. ) ;
#33843 = ORIENTED_EDGE ( 'NONE', *, *, #37923, .F. ) ;
#33844 = FACE_OUTER_BOUND ( 'NONE', #530, .T. ) ;
#33845 = CONICAL_SURFACE ( 'NONE', #73541, 0.1000000000000002554, 0.003490658503988666988 ) ;
#33846 = EDGE_LOOP ( 'NONE', ( #86977, #47355, #64084, #26060 ) ) ;
#33847 = ORIENTED_EDGE ( 'NONE', *, *, #16615, .F. ) ;
#33848 = CARTESIAN_POINT ( 'NONE',  ( 6.849999999999929479, 2.500000000000000000, 6.148780366869520009 ) ) ;
#33849 = FACE_OUTER_BOUND ( 'NONE', #63865, .T. ) ;
#33850 = FACE_OUTER_BOUND ( 'NONE', #62983, .T. ) ;
#33851 = CARTESIAN_POINT ( 'NONE',  ( 3.299999999999944755, 12.50000000000000000, -4.330127018922201643 ) ) ;
#33852 = DIRECTION ( 'NONE',  ( 0.000000000000000000, -0.9999939076577903929, 0.003490651415223739937 ) ) ;
#33853 = ORIENTED_EDGE ( 'NONE', *, *, #77695, .F. ) ;
#33854 = VERTEX_POINT ( 'NONE', #28640 ) ;
#33855 = CARTESIAN_POINT ( 'NONE',  ( -6.250000000000017764, 2.500000000000000000, 2.857883832488649301 ) ) ;
#33856 = FACE_BOUND ( 'NONE', #23103, .T. ) ;
#33857 = DIRECTION ( 'NONE',  ( 0.000000000000000000, 0.000000000000000000, 1.000000000000000000 ) ) ;
#33858 = ORIENTED_EDGE ( 'NONE', *, *, #20768, .F. ) ;
#33859 = ORIENTED_EDGE ( 'NONE', *, *, #96525, .F. ) ;
#33860 = DIRECTION ( 'NONE',  ( 0.000000000000000000, 0.000000000000000000, -1.000000000000000000 ) ) ;
#33862 = ORIENTED_EDGE ( 'NONE', *, *, #23228, .T. ) ;
#33861 = VECTOR ( 'NONE', #51473, 1000.000000000000000 ) ;
#33863 = FACE_OUTER_BOUND ( 'NONE', #106769, .T. ) ;
#33864 = AXIS2_PLACEMENT_3D ( 'NONE', #57058, #104866, #44684 ) ;
#33865 = ADVANCED_FACE ( 'NONE', ( #117624 ), #69372, .T. ) ;
#33866 = DIRECTION ( 'NONE',  ( 0.000000000000000000, 0.000000000000000000, 1.000000000000000000 ) ) ;
#33867 = VERTEX_POINT ( 'NONE', #90104 ) ;
#33868 = CARTESIAN_POINT ( 'NONE',  ( 10.79999999999991012, 12.50000000000000000, 4.330127018922196314 ) ) ;
#33869 = DIRECTION ( 'NONE',  ( -0.000000000000000000, 1.000000000000000000, -0.000000000000000000 ) ) ;
#33870 = DIRECTION ( 'NONE',  ( 0.000000000000000000, 1.000000000000000000, 0.000000000000000000 ) ) ;
#33871 = EDGE_CURVE ( 'NONE', #56128, #47717, #15058, .T. ) ;
#33873 = AXIS2_PLACEMENT_3D ( 'NONE', #60045, #39764, #108469 ) ;
#33872 = DIRECTION ( 'NONE',  ( 0.000000000000000000, 0.000000000000000000, 1.000000000000000000 ) ) ;
#33874 = EDGE_CURVE ( 'NONE', #117143, #79361, #99309, .T. ) ;
#33875 = EDGE_LOOP ( 'NONE', ( #59175, #99892 ) ) ;
#33876 = AXIS2_PLACEMENT_3D ( 'NONE', #84083, #54621, #55919 ) ;
#33877 = CIRCLE ( 'NONE', #10865, 0.06509327318403745899 ) ;
#33878 = CARTESIAN_POINT ( 'NONE',  ( 14.34999999999989306, 2.500000000000000000, -1.718653347947326049 ) ) ;
#33879 = CONICAL_SURFACE ( 'NONE', #88228, 0.1000000000000002554, 0.003490658503988666988 ) ;
#33880 = CARTESIAN_POINT ( 'NONE',  ( 32.27111852103835332, -3.178312372601638902, 3.140919221367066694 ) ) ;
#33881 = ADVANCED_FACE ( 'NONE', ( #434 ), #127481, .T. ) ;
#33882 = VERTEX_POINT ( 'NONE', #29284 ) ;
#33883 = EDGE_CURVE ( 'NONE', #47772, #21032, #406, .T. ) ;
#33884 = ORIENTED_EDGE ( 'NONE', *, *, #62875, .T. ) ;
#33885 = ADVANCED_FACE ( 'NONE', ( #116988 ), #109064, .T. ) ;
#33886 = CARTESIAN_POINT ( 'NONE',  ( 184.4010416670080872, -4.367472073101519747, 7.564683531249999149 ) ) ;
#33888 = EDGE_CURVE ( 'NONE', #96407, #35702, #50597, .T. ) ;
#33887 = DIRECTION ( 'NONE',  ( 0.000000000000000000, 0.000000000000000000, -1.000000000000000000 ) ) ;
#33889 = ADVANCED_FACE ( 'NONE', ( #39125 ), #115322, .T. ) ;
#33890 = DIRECTION ( 'NONE',  ( 0.000000000000000000, 0.000000000000000000, -1.000000000000000000 ) ) ;
#33891 = AXIS2_PLACEMENT_3D ( 'NONE', #5273, #125687, #16367 ) ;
#33892 = DIRECTION ( 'NONE',  ( -0.000000000000000000, -1.000000000000000000, -0.000000000000000000 ) ) ;
#33893 = DIRECTION ( 'NONE',  ( -0.000000000000000000, -1.000000000000000000, -0.000000000000000000 ) ) ;
#33894 = AXIS2_PLACEMENT_3D ( 'NONE', #74052, #72764, #113977 ) ;
#33895 = DIRECTION ( 'NONE',  ( -0.000000000000000000, -1.000000000000000000, -0.000000000000000000 ) ) ;
#33896 = CARTESIAN_POINT ( 'NONE',  ( 9.399999999999918643, 2.500000000000000000, 0.3464101615137736845 ) ) ;
#33897 = CONICAL_SURFACE ( 'NONE', #107033, 0.09999999999999982514, 0.003490658503988666988 ) ;
#33898 = CARTESIAN_POINT ( 'NONE',  ( 1.249999999999950262, 12.50000000000000000, 7.253104124594885960 ) ) ;
#33899 = AXIS2_PLACEMENT_3D ( 'NONE', #40819, #80731, #121288 ) ;
#33900 = CARTESIAN_POINT ( 'NONE',  ( 179.5000000000000000, 1.375000000000000222, 6.000000000000000000 ) ) ;
#33901 = VECTOR ( 'NONE', #74096, 1000.000000000000000 ) ;
#33902 = CARTESIAN_POINT ( 'NONE',  ( 4.199999999999939782, 12.50000000000000000, -0.06509327318403970719 ) ) ;
#33903 = ADVANCED_FACE ( 'NONE', ( #107179 ), #69845, .T. ) ;
#33904 = CARTESIAN_POINT ( 'NONE',  ( 13.54999999999989591, 2.500000000000000000, -1.818653347947326138 ) ) ;
#33905 = ORIENTED_EDGE ( 'NONE', *, *, #83952, .F. ) ;
#33906 = EDGE_CURVE ( 'NONE', #51386, #44872, #12927, .T. ) ;
#33907 = ORIENTED_EDGE ( 'NONE', *, *, #322, .F. ) ;
#33908 = CONICAL_SURFACE ( 'NONE', #54723, 0.1000000000000002554, 0.003490658503988666988 ) ;
#33909 = ORIENTED_EDGE ( 'NONE', *, *, #37309, .F. ) ;
#33910 = EDGE_LOOP ( 'NONE', ( #80048, #3964, #64613, #38394 ) ) ;
#33911 = DIRECTION ( 'NONE',  ( -0.000000000000000000, -1.000000000000000000, -0.000000000000000000 ) ) ;
#33912 = CARTESIAN_POINT ( 'NONE',  ( -3.350000000000028511, 12.50000000000000000, -1.537336459617587581 ) ) ;
#33913 = ORIENTED_EDGE ( 'NONE', *, *, #19009, .T. ) ;
#33914 = CARTESIAN_POINT ( 'NONE',  ( -3.350000000000028511, 2.500000000000000000, -2.757883832488654097 ) ) ;
#33915 = PLANE ( 'NONE',  #5415 ) ;
#33917 = VERTEX_POINT ( 'NONE', #87539 ) ;
#33916 = DIRECTION ( 'NONE',  ( 0.000000000000000000, 0.000000000000000000, 1.000000000000000000 ) ) ;
#33918 = DIRECTION ( 'NONE',  ( 0.000000000000000000, 0.000000000000000000, 1.000000000000000000 ) ) ;
#33919 = DIRECTION ( 'NONE',  ( -4.274815082592931898E-19, -0.9999939076577903929, -0.003490651415223739937 ) ) ;
#33920 = EDGE_LOOP ( 'NONE', ( #54497, #39197, #54856, #27292 ) ) ;
#33921 = ORIENTED_EDGE ( 'NONE', *, *, #122605, .F. ) ;
#33922 = ORIENTED_EDGE ( 'NONE', *, *, #100074, .F. ) ;
#33923 = VECTOR ( 'NONE', #3063, 1000.000000000000000 ) ;
#33924 = VERTEX_POINT ( 'NONE', #67903 ) ;
#33925 = DIRECTION ( 'NONE',  ( 0.000000000000000000, 0.000000000000000000, -1.000000000000000000 ) ) ;
#33926 = AXIS2_PLACEMENT_3D ( 'NONE', #55828, #65643, #16525 ) ;
#33928 = ADVANCED_FACE ( 'NONE', ( #107833 ), #18154, .T. ) ;
#33927 = CIRCLE ( 'NONE', #27639, 0.06509327318403741736 ) ;
#33929 = ADVANCED_FACE ( 'NONE', ( #100576 ), #20743, .F. ) ;
#33930 = DIRECTION ( 'NONE',  ( -0.000000000000000000, -1.000000000000000000, -0.000000000000000000 ) ) ;
#33932 = EDGE_CURVE ( 'NONE', #76503, #37568, #29679, .T. ) ;
#33931 = CARTESIAN_POINT ( 'NONE',  ( 13.34999999999989662, 12.50000000000000000, -2.099970236277064473 ) ) ;
#33933 = DIRECTION ( 'NONE',  ( 0.000000000000000000, 0.000000000000000000, -1.000000000000000000 ) ) ;
#33935 = EDGE_LOOP ( 'NONE', ( #59005, #47633 ) ) ;
#33934 = CONICAL_SURFACE ( 'NONE', #88185, 0.1000000000000002554, 0.003490658503988666988 ) ;
#33936 = AXIS2_PLACEMENT_3D ( 'NONE', #42618, #94266, #43902 ) ;
#33937 = EDGE_CURVE ( 'NONE', #124362, #127904, #88486, .T. ) ;
#33938 = AXIS2_PLACEMENT_3D ( 'NONE', #100812, #109359, #39994 ) ;
#33939 = DIRECTION ( 'NONE',  ( 0.000000000000000000, 0.000000000000000000, 1.000000000000000000 ) ) ;
#33941 = ORIENTED_EDGE ( 'NONE', *, *, #46970, .T. ) ;
#33940 = CIRCLE ( 'NONE', #12982, 0.06509327318403743123 ) ;
#33942 = CARTESIAN_POINT ( 'NONE',  ( 9.549999999999918998, 12.50000000000000000, -6.430097255199264339 ) ) ;
#33943 = CARTESIAN_POINT ( 'NONE',  ( 10.87377556642347010, -1.500000000000192513, -8.986829606637039447 ) ) ;
#33944 = CIRCLE ( 'NONE', #46447, 0.1000000000000002554 ) ;
#33945 = CARTESIAN_POINT ( 'NONE',  ( 11.64999999999990266, 12.50000000000000000, 2.099970236277060032 ) ) ;
#33946 = CARTESIAN_POINT ( 'NONE',  ( -1.250000000000037526, 12.50000000000000000, -5.802370205355749988 ) ) ;
#33947 = EDGE_CURVE ( 'NONE', #460, #25156, #100756, .T. ) ;
#33948 = AXIS2_PLACEMENT_3D ( 'NONE', #53544, #92828, #50976 ) ;
#33949 = ADVANCED_FACE ( 'NONE', ( #103169 ), #92050, .T. ) ;
#33950 = EDGE_LOOP ( 'NONE', ( #68110, #38341 ) ) ;
#33951 = EDGE_CURVE ( 'NONE', #54777, #109103, #102814, .T. ) ;
#33952 = ORIENTED_EDGE ( 'NONE', *, *, #111281, .F. ) ;
#33953 = ORIENTED_EDGE ( 'NONE', *, *, #97437, .T. ) ;
#33954 = DIRECTION ( 'NONE',  ( -0.000000000000000000, -1.000000000000000000, -0.000000000000000000 ) ) ;
#33955 = DIRECTION ( 'NONE',  ( 0.000000000000000000, 0.000000000000000000, 1.000000000000000000 ) ) ;
#33956 = DIRECTION ( 'NONE',  ( 0.000000000000000000, 1.000000000000000000, 0.000000000000000000 ) ) ;
#33957 = FACE_BOUND ( 'NONE', #116548, .T. ) ;
#33958 = LINE ( 'NONE', #22222, #116171 ) ;
#33959 = CARTESIAN_POINT ( 'NONE',  ( 5.199999999999935341, 2.500000000000000000, -3.883716857408426648 ) ) ;
#33960 = EDGE_CURVE ( 'NONE', #128018, #92934, #46381, .T. ) ;
#33961 = CARTESIAN_POINT ( 'NONE',  ( 5.849999999999932143, 2.500000000000000000, 1.472243186433545459 ) ) ;
#33962 = CIRCLE ( 'NONE', #113655, 0.1000000000000002554 ) ;
#33963 = CARTESIAN_POINT ( 'NONE',  ( -9.400000000000009237, 2.500000000000000000, -3.983716857408421852 ) ) ;
#33964 = CARTESIAN_POINT ( 'NONE',  ( -11.24999999999996447, 12.50000000000000000, -2.165063509461097713 ) ) ;
#33965 = DIRECTION ( 'NONE',  ( -0.000000000000000000, 1.000000000000000000, -0.000000000000000000 ) ) ;
#33966 = ORIENTED_EDGE ( 'NONE', *, *, #102227, .F. ) ;
#33967 = AXIS2_PLACEMENT_3D ( 'NONE', #37636, #97822, #105722 ) ;
#33968 = CONICAL_SURFACE ( 'NONE', #73960, 0.09999999999999999167, 0.003490658503988666988 ) ;
#33969 = CARTESIAN_POINT ( 'NONE',  ( 10.84999999999991260, 2.500000000000000000, -2.065063509461102065 ) ) ;
#33970 = VERTEX_POINT ( 'NONE', #1731 ) ;
#33971 = EDGE_LOOP ( 'NONE', ( #9444, #67582, #56358, #31533 ) ) ;
#33972 = EDGE_LOOP ( 'NONE', ( #15480, #69240, #68935, #118863 ) ) ;
#33973 = VERTEX_POINT ( 'NONE', #41691 ) ;
#33974 = CARTESIAN_POINT ( 'NONE',  ( 9.149999999999918643, 12.50000000000000000, 2.099970236277060032 ) ) ;
#33975 = EDGE_CURVE ( 'NONE', #122222, #83264, #63243, .T. ) ;
#33976 = FACE_BOUND ( 'NONE', #26646, .T. ) ;
#33977 = AXIS2_PLACEMENT_3D ( 'NONE', #103818, #6230, #113635 ) ;
#33978 = DIRECTION ( 'NONE',  ( 0.000000000000000000, 1.000000000000000000, 0.000000000000000000 ) ) ;
#33979 = CIRCLE ( 'NONE', #90386, 0.1000000000000002554 ) ;
#33980 = ORIENTED_EDGE ( 'NONE', *, *, #47504, .F. ) ;
#33981 = CARTESIAN_POINT ( 'NONE',  ( 21.23528140090950700, 2.699413673072311060, 2.293764360948887138 ) ) ;
#33982 = CARTESIAN_POINT ( 'NONE',  ( -2.900000000000029221, 2.500000000000000000, -4.230127018922201998 ) ) ;
#33983 = ORIENTED_EDGE ( 'NONE', *, *, #42167, .F. ) ;
#33985 = DIRECTION ( 'NONE',  ( 0.000000000000000000, 0.000000000000000000, -1.000000000000000000 ) ) ;
#33984 = CIRCLE ( 'NONE', #75826, 0.1000000000000000472 ) ;
#33986 = FACE_OUTER_BOUND ( 'NONE', #126921, .T. ) ;
#33987 = CONICAL_SURFACE ( 'NONE', #125998, 0.1000000000000000472, 0.003490658503988666988 ) ;
#33988 = ADVANCED_FACE ( 'NONE', ( #31857 ), #73571, .T. ) ;
#33989 = AXIS2_PLACEMENT_3D ( 'NONE', #34033, #4535, #13730 ) ;
#33990 = AXIS2_PLACEMENT_3D ( 'NONE', #25489, #54325, #115141 ) ;
#33991 = AXIS2_PLACEMENT_3D ( 'NONE', #35312, #83755, #115116 ) ;
#33992 = EDGE_LOOP ( 'NONE', ( #68376, #128564, #77335, #65646 ) ) ;
#33993 = DIRECTION ( 'NONE',  ( 0.000000000000000000, 1.000000000000000000, 0.000000000000000000 ) ) ;
#33994 = CARTESIAN_POINT ( 'NONE',  ( 10.39999999999990976, 12.50000000000000000, 4.330127018922196314 ) ) ;
#33995 = VECTOR ( 'NONE', #95468, 1000.000000000000000 ) ;
#33996 = ORIENTED_EDGE ( 'NONE', *, *, #37368, .F. ) ;
#33997 = DIRECTION ( 'NONE',  ( 0.000000000000000000, 0.000000000000000000, -1.000000000000000000 ) ) ;
#33998 = CONICAL_SURFACE ( 'NONE', #75750, 0.09999999999999982514, 0.003490658503988666988 ) ;
#33999 = CARTESIAN_POINT ( 'NONE',  ( 186.9479166673494603, -6.668395609140176816, -3.850000000000003642 ) ) ;
#34000 = DIRECTION ( 'NONE',  ( 0.000000000000000000, 0.000000000000000000, -1.000000000000000000 ) ) ;
#34001 = ORIENTED_EDGE ( 'NONE', *, *, #61518, .F. ) ;
#34002 = ORIENTED_EDGE ( 'NONE', *, *, #61515, .T. ) ;
#34003 = EDGE_CURVE ( 'NONE', #125076, #885, #56831, .T. ) ;
#34004 = CARTESIAN_POINT ( 'NONE',  ( -0.6000000000000388356, 2.500000000000000000, 4.776537180435972196 ) ) ;
#34005 = ORIENTED_EDGE ( 'NONE', *, *, #123477, .F. ) ;
#34006 = DIRECTION ( 'NONE',  ( 0.000000000000000000, 1.000000000000000000, 0.000000000000000000 ) ) ;
#34007 = DIRECTION ( 'NONE',  ( 0.000000000000000000, 0.000000000000000000, 1.000000000000000000 ) ) ;
#34008 = EDGE_LOOP ( 'NONE', ( #80612, #124042 ) ) ;
#34009 = DIRECTION ( 'NONE',  ( 0.000000000000000000, 0.000000000000000000, -1.000000000000000000 ) ) ;
#34010 = CARTESIAN_POINT ( 'NONE',  ( -4.999999999999986677, 2.500000000000000000, 4.330127018922196314 ) ) ;
#34011 = DIRECTION ( 'NONE',  ( 0.000000000000000000, 1.000000000000000000, 0.000000000000000000 ) ) ;
#34012 = DIRECTION ( 'NONE',  ( -0.000000000000000000, -1.000000000000000000, -0.000000000000000000 ) ) ;
#34013 = AXIS2_PLACEMENT_3D ( 'NONE', #17790, #59021, #57743 ) ;
#34014 = CARTESIAN_POINT ( 'NONE',  ( -3.749999999999991562, 12.50000000000000000, 6.495190528383297135 ) ) ;
#34015 = VERTEX_POINT ( 'NONE', #22693 ) ;
#34016 = ORIENTED_EDGE ( 'NONE', *, *, #101145, .T. ) ;
#34017 = CARTESIAN_POINT ( 'NONE',  ( 9.199999999999915801, 12.50000000000000000, -4.330127018922201643 ) ) ;
#34018 = CONICAL_SURFACE ( 'NONE', #19330, 0.1000000000000002554, 0.003490658503988666988 ) ;
#34019 = CARTESIAN_POINT ( 'NONE',  ( 103.0416120702864475, 7.673033776031224384, -0.6654386271658147001 ) ) ;
#34020 = CONICAL_SURFACE ( 'NONE', #90426, 0.1000000000000002554, 0.003490658503988666988 ) ;
#34022 = EDGE_LOOP ( 'NONE', ( #34184, #124683 ) ) ;
#34021 = ORIENTED_EDGE ( 'NONE', *, *, #100245, .F. ) ;
#34023 = ORIENTED_EDGE ( 'NONE', *, *, #1160, .T. ) ;
#34024 = DIRECTION ( 'NONE',  ( -0.000000000000000000, 1.000000000000000000, -0.000000000000000000 ) ) ;
#34025 = DIRECTION ( 'NONE',  ( 0.000000000000000000, 1.000000000000000000, 0.000000000000000000 ) ) ;
#34026 = AXIS2_PLACEMENT_3D ( 'NONE', #102768, #81221, #13093 ) ;
#34028 = CARTESIAN_POINT ( 'NONE',  ( -6.700000000000019718, 12.50000000000000000, -4.330127018922201643 ) ) ;
#34027 = AXIS2_PLACEMENT_3D ( 'NONE', #69979, #79789, #78528 ) ;
#34029 = EDGE_CURVE ( 'NONE', #27373, #57931, #90764, .T. ) ;
#34030 = DIRECTION ( 'NONE',  ( 0.000000000000000000, 0.000000000000000000, 1.000000000000000000 ) ) ;
#34031 = LINE ( 'NONE', #113219, #39001 ) ;
#34032 = CARTESIAN_POINT ( 'NONE',  ( -13.09999999999999254, 2.500000000000000000, 0.3464101615137777923 ) ) ;
#34033 = CARTESIAN_POINT ( 'NONE',  ( 12.89999999999990266, 12.50000000000000000, -5.022947341949754119 ) ) ;
#34034 = DIRECTION ( 'NONE',  ( 0.000000000000000000, 0.000000000000000000, 1.000000000000000000 ) ) ;
#34035 = DIRECTION ( 'NONE',  ( -0.000000000000000000, 1.000000000000000000, -0.000000000000000000 ) ) ;
#34036 = AXIS2_PLACEMENT_3D ( 'NONE', #79530, #119433, #295 ) ;
#34037 = CIRCLE ( 'NONE', #57303, 0.06509327318403745899 ) ;
#34038 = LINE ( 'NONE', #125620, #129319 ) ;
#34039 = EDGE_CURVE ( 'NONE', #98092, #63695, #19280, .T. ) ;
#34040 = ORIENTED_EDGE ( 'NONE', *, *, #41972, .T. ) ;
#34041 = CARTESIAN_POINT ( 'NONE',  ( -5.450000000000019718, 2.500000000000000000, 6.495190528383297135 ) ) ;
#34042 = EDGE_CURVE ( 'NONE', #41518, #10631, #79935, .T. ) ;
#34043 = ORIENTED_EDGE ( 'NONE', *, *, #66010, .F. ) ;
#34044 = EDGE_CURVE ( 'NONE', #62494, #117214, #123442, .T. ) ;
#34045 = ORIENTED_EDGE ( 'NONE', *, *, #6599, .T. ) ;
#34046 = ADVANCED_FACE ( 'NONE', ( #54068 ), #95285, .T. ) ;
#34047 = CARTESIAN_POINT ( 'NONE',  ( -8.550000000000013145, 2.500000000000000000, -1.818653347947326138 ) ) ;
#34049 = ADVANCED_FACE ( 'NONE', ( #46178 ), #75619, .T. ) ;
#34048 = CARTESIAN_POINT ( 'NONE',  ( 6.649999999999928413, 2.500000000000000000, 1.472243186433545459 ) ) ;
#34050 = DIRECTION ( 'NONE',  ( 0.000000000000000000, 0.000000000000000000, -1.000000000000000000 ) ) ;
#34051 = CIRCLE ( 'NONE', #69537, 0.1000000000000002554 ) ;
#34052 = CARTESIAN_POINT ( 'NONE',  ( -6.450000000000016165, 12.50000000000000000, 2.511473670974873507 ) ) ;
#34053 = DIRECTION ( 'NONE',  ( 0.000000000000000000, 0.000000000000000000, -1.000000000000000000 ) ) ;
#34054 = ADVANCED_FACE ( 'NONE', ( #55987 ), #92456, .T. ) ;
#34055 = CARTESIAN_POINT ( 'NONE',  ( -11.64999999999999680, 12.50000000000000000, 1.472243186433545459 ) ) ;
#34056 = DIRECTION ( 'NONE',  ( -0.000000000000000000, -1.000000000000000000, -0.000000000000000000 ) ) ;
#34057 = VERTEX_POINT ( 'NONE', #14754 ) ;
#34058 = CARTESIAN_POINT ( 'NONE',  ( 186.7812500006828031, 0.000000000000000000, 7.700000000000000178 ) ) ;
#34059 = EDGE_CURVE ( 'NONE', #18421, #68242, #121782, .T. ) ;
#34060 = AXIS2_PLACEMENT_3D ( 'NONE', #91880, #2192, #74174 ) ;
#34063 = EDGE_CURVE ( 'NONE', #776, #90572, #109164, .T. ) ;
#34062 = CONICAL_SURFACE ( 'NONE', #98792, 0.1000000000000002554, 0.003490658503988666988 ) ;
#34061 = CARTESIAN_POINT ( 'NONE',  ( -7.500000000000015099, 2.500000000000000000, -0.6928203230275541413 ) ) ;
#34064 = VERTEX_POINT ( 'NONE', #24612 ) ;
#34065 = CIRCLE ( 'NONE', #82079, 0.06509327318403745899 ) ;
#34066 = EDGE_CURVE ( 'NONE', #123447, #10798, #36028, .T. ) ;
#34067 = EDGE_LOOP ( 'NONE', ( #25216, #95832 ) ) ;
#34068 = ORIENTED_EDGE ( 'NONE', *, *, #58639, .T. ) ;
#34069 = EDGE_LOOP ( 'NONE', ( #73043, #125853, #124220, #6470 ) ) ;
#34071 = ADVANCED_FACE ( 'NONE', ( #105082 ), #86173, .T. ) ;
#34070 = AXIS2_PLACEMENT_3D ( 'NONE', #89962, #40229, #282 ) ;
#34072 = CARTESIAN_POINT ( 'NONE',  ( 2.299999999999949640, 2.500000000000000000, -0.4464101615137782142 ) ) ;
#34073 = CARTESIAN_POINT ( 'NONE',  ( 6.899999999999928413, 2.500000000000000000, 4.776537180435972196 ) ) ;
#34074 = VECTOR ( 'NONE', #28088, 1000.000000000000000 ) ;
#34075 = AXIS2_PLACEMENT_3D ( 'NONE', #19011, #31439, #58328 ) ;
#34076 = CARTESIAN_POINT ( 'NONE',  ( -2.050000000000032685, 2.500000000000000000, -6.595190528383302109 ) ) ;
#34077 = DIRECTION ( 'NONE',  ( 0.000000000000000000, 0.000000000000000000, -1.000000000000000000 ) ) ;
#34078 = DIRECTION ( 'NONE',  ( -0.000000000000000000, 1.000000000000000000, -0.000000000000000000 ) ) ;
#34079 = VERTEX_POINT ( 'NONE', #124093 ) ;
#34080 = DIRECTION ( 'NONE',  ( 0.000000000000000000, -0.9999939076577903929, 0.003490651415223739937 ) ) ;
#34081 = DIRECTION ( 'NONE',  ( -4.274815082592931898E-19, -0.9999939076577903929, -0.003490651415223739937 ) ) ;
#34082 = AXIS2_PLACEMENT_3D ( 'NONE', #104615, #84341, #77103 ) ;
#34083 = AXIS2_PLACEMENT_3D ( 'NONE', #91379, #1701, #81563 ) ;
#34084 = CARTESIAN_POINT ( 'NONE',  ( -4.150000000000028777, 2.500000000000000000, -5.802370205355749988 ) ) ;
#34085 = ORIENTED_EDGE ( 'NONE', *, *, #126087, .T. ) ;
#34086 = CIRCLE ( 'NONE', #21560, 0.06509327318403743123 ) ;
#34087 = CONICAL_SURFACE ( 'NONE', #121806, 0.09999999999999982514, 0.003490658503988666988 ) ;
#34088 = CONICAL_SURFACE ( 'NONE', #23716, 0.09999999999999982514, 0.003490658503988666988 ) ;
#34089 = VERTEX_POINT ( 'NONE', #55359 ) ;
#34090 = ORIENTED_EDGE ( 'NONE', *, *, #123160, .F. ) ;
#34091 = FACE_OUTER_BOUND ( 'NONE', #2039, .T. ) ;
#34092 = CONICAL_SURFACE ( 'NONE', #69587, 0.1000000000000002554, 0.003490658503988666988 ) ;
#34093 = DIRECTION ( 'NONE',  ( -0.000000000000000000, -1.000000000000000000, -0.000000000000000000 ) ) ;
#34094 = DIRECTION ( 'NONE',  ( 0.000000000000000000, 0.000000000000000000, 1.000000000000000000 ) ) ;
#34095 = AXIS2_PLACEMENT_3D ( 'NONE', #56819, #58154, #98057 ) ;
#34096 = EDGE_LOOP ( 'NONE', ( #55695, #93011, #95463, #104196 ) ) ;
#34097 = DIRECTION ( 'NONE',  ( 0.000000000000000000, 0.000000000000000000, 1.000000000000000000 ) ) ;
#34098 = DIRECTION ( 'NONE',  ( -0.000000000000000000, -1.000000000000000000, -0.000000000000000000 ) ) ;
#34099 = CARTESIAN_POINT ( 'NONE',  ( 2.949999999999945111, 12.50000000000000000, 2.165063509461097713 ) ) ;
#34100 = DIRECTION ( 'NONE',  ( -0.000000000000000000, -1.000000000000000000, -0.000000000000000000 ) ) ;
#34101 = EDGE_CURVE ( 'NONE', #65379, #126646, #48644, .T. ) ;
#34102 = CARTESIAN_POINT ( 'NONE',  ( -14.59999999999998366, 2.500000000000000000, -0.6928203230275520319 ) ) ;
#34103 = EDGE_CURVE ( 'NONE', #99278, #90531, #116196, .T. ) ;
#34104 = ORIENTED_EDGE ( 'NONE', *, *, #12811, .T. ) ;
#34105 = CONICAL_SURFACE ( 'NONE', #107255, 0.1000000000000002554, 0.003490658503988666988 ) ;
#34106 = ORIENTED_EDGE ( 'NONE', *, *, #24167, .F. ) ;
#34107 = CONICAL_SURFACE ( 'NONE', #67528, 0.09999999999999982514, 0.003490658503988666988 ) ;
#34108 = LINE ( 'NONE', #2688, #50186 ) ;
#34109 = FACE_OUTER_BOUND ( 'NONE', #31887, .T. ) ;
#34110 = DIRECTION ( 'NONE',  ( -0.000000000000000000, 1.000000000000000000, -0.000000000000000000 ) ) ;
#34111 = DIRECTION ( 'NONE',  ( -0.000000000000000000, -1.000000000000000000, -0.000000000000000000 ) ) ;
#34112 = EDGE_CURVE ( 'NONE', #76479, #16894, #56926, .T. ) ;
#34113 = DIRECTION ( 'NONE',  ( 0.000000000000000000, 1.000000000000000000, 0.000000000000000000 ) ) ;
#34114 = ORIENTED_EDGE ( 'NONE', *, *, #65949, .T. ) ;
#34115 = AXIS2_PLACEMENT_3D ( 'NONE', #64509, #94611, #24595 ) ;
#34116 = CIRCLE ( 'NONE', #73811, 0.06509327318403745899 ) ;
#34117 = AXIS2_PLACEMENT_3D ( 'NONE', #122249, #120940, #32596 ) ;
#34118 = AXIS2_PLACEMENT_3D ( 'NONE', #56574, #93947, #106339 ) ;
#34119 = ORIENTED_EDGE ( 'NONE', *, *, #76568, .F. ) ;
#34120 = DIRECTION ( 'NONE',  ( 0.000000000000000000, 0.000000000000000000, -1.000000000000000000 ) ) ;
#34121 = CARTESIAN_POINT ( 'NONE',  ( 1.699999999999950218, 12.50000000000000000, 4.330127018922196314 ) ) ;
#34122 = CARTESIAN_POINT ( 'NONE',  ( 17.50982738792208693, -2.500000000000000000, -4.074750937467086054 ) ) ;
#34123 = CARTESIAN_POINT ( 'NONE',  ( -9.400000000000007461, 2.500000000000000000, 0.3464101615137735735 ) ) ;
#34124 = VERTEX_POINT ( 'NONE', #45550 ) ;
#34126 = LINE ( 'NONE', #15747, #78286 ) ;
#34125 = CIRCLE ( 'NONE', #40391, 0.06509327318403741736 ) ;
#34127 = AXIS2_PLACEMENT_3D ( 'NONE', #107149, #94764, #76422 ) ;
#34128 = CIRCLE ( 'NONE', #15317, 0.06509327318403745899 ) ;
#34129 = CARTESIAN_POINT ( 'NONE',  ( 1.249999999999952482, 2.500000000000000000, -5.902370205355750521 ) ) ;
#34130 = CONICAL_SURFACE ( 'NONE', #78032, 0.1000000000000002554, 0.003490658503988666988 ) ;
#34131 = ORIENTED_EDGE ( 'NONE', *, *, #114243, .T. ) ;
#34132 = DIRECTION ( 'NONE',  ( 0.000000000000000000, 0.000000000000000000, -1.000000000000000000 ) ) ;
#34133 = ORIENTED_EDGE ( 'NONE', *, *, #7482, .F. ) ;
#34134 = CIRCLE ( 'NONE', #96810, 0.1000000000000000472 ) ;
#34135 = LINE ( 'NONE', #113974, #49301 ) ;
#34136 = ORIENTED_EDGE ( 'NONE', *, *, #12413, .F. ) ;
#34137 = DIRECTION ( 'NONE',  ( 0.000000000000000000, 0.000000000000000000, 1.000000000000000000 ) ) ;
#34138 = CARTESIAN_POINT ( 'NONE',  ( 9.349999999999919709, 12.50000000000000000, 2.576566944158910744 ) ) ;
#34139 = ORIENTED_EDGE ( 'NONE', *, *, #106779, .T. ) ;
#34140 = ORIENTED_EDGE ( 'NONE', *, *, #96858, .F. ) ;
#34141 = CARTESIAN_POINT ( 'NONE',  ( 186.5885416670080872, -6.551208109652273848, -3.782341765625003571 ) ) ;
#34142 = CARTESIAN_POINT ( 'NONE',  ( -9.150000000000005684, 2.500000000000000000, 5.802370205355744659 ) ) ;
#34143 = CARTESIAN_POINT ( 'NONE',  ( 185.0468750003414300, -8.734944146203032389, -1.604583208406767949E-15 ) ) ;
#34144 = CARTESIAN_POINT ( 'NONE',  ( 127.5000000000000000, 1.500000000000000000, -6.000000000000000000 ) ) ;
#34145 = DIRECTION ( 'NONE',  ( 0.000000000000000000, 1.000000000000000000, 0.000000000000000000 ) ) ;
#34146 = DIRECTION ( 'NONE',  ( 0.000000000000000000, 1.000000000000000000, 0.000000000000000000 ) ) ;
#34147 = CARTESIAN_POINT ( 'NONE',  ( 10.79999999999991367, 2.500000000000000000, -2.385244779468109755E-15 ) ) ;
#34148 = DIRECTION ( 'NONE',  ( -0.000000000000000000, -1.000000000000000000, -0.000000000000000000 ) ) ;
#34149 = CONICAL_SURFACE ( 'NONE', #126073, 0.1000000000000002554, 0.003490658503988666988 ) ;
#34150 = AXIS2_PLACEMENT_3D ( 'NONE', #75492, #113493, #23841 ) ;
#34151 = AXIS2_PLACEMENT_3D ( 'NONE', #28196, #27525, #18997 ) ;
#34152 = ORIENTED_EDGE ( 'NONE', *, *, #116007, .F. ) ;
#34153 = ORIENTED_EDGE ( 'NONE', *, *, #109904, .F. ) ;
#34154 = DIRECTION ( 'NONE',  ( -0.000000000000000000, -1.000000000000000000, -0.000000000000000000 ) ) ;
#34155 = CARTESIAN_POINT ( 'NONE',  ( -1.050000000000037792, 2.500000000000000000, 6.048780366869520364 ) ) ;
#34156 = DIRECTION ( 'NONE',  ( 0.000000000000000000, -0.9999939076577903929, 0.003490651415223739937 ) ) ;
#34157 = EDGE_CURVE ( 'NONE', #124875, #8330, #65347, .T. ) ;
#34158 = DIRECTION ( 'NONE',  ( 0.000000000000000000, 0.000000000000000000, 1.000000000000000000 ) ) ;
#34160 = ORIENTED_EDGE ( 'NONE', *, *, #65210, .T. ) ;
#34159 = ORIENTED_EDGE ( 'NONE', *, *, #105596, .T. ) ;
#34161 = FACE_BOUND ( 'NONE', #49684, .T. ) ;
#34162 = EDGE_LOOP ( 'NONE', ( #54645, #105797 ) ) ;
#34163 = EDGE_CURVE ( 'NONE', #100499, #41901, #115541, .T. ) ;
#34164 = AXIS2_PLACEMENT_3D ( 'NONE', #81758, #121684, #32049 ) ;
#34165 = CARTESIAN_POINT ( 'NONE',  ( 0.4499999999999573785, 2.500000000000000000, -6.595190528383302109 ) ) ;
#34166 = CARTESIAN_POINT ( 'NONE',  ( 19.95908882845278853, -2.629614671951212568, 2.273431397254419117 ) ) ;
#34167 = CIRCLE ( 'NONE', #67586, 0.06509327318403741736 ) ;
#34168 = VERTEX_POINT ( 'NONE', #16052 ) ;
#34170 = DIRECTION ( 'NONE',  ( -4.274815082592931898E-19, -0.9999939076577903929, -0.003490651415223739937 ) ) ;
#34169 = CIRCLE ( 'NONE', #29967, 0.1000000000000000472 ) ;
#34171 = DIRECTION ( 'NONE',  ( 0.000000000000000000, 1.000000000000000000, 0.000000000000000000 ) ) ;
#34172 = CONICAL_SURFACE ( 'NONE', #126089, 0.1000000000000002554, 0.003490658503988666988 ) ;
#34173 = DIRECTION ( 'NONE',  ( 0.000000000000000000, 1.000000000000000000, 0.000000000000000000 ) ) ;
#34174 = FACE_OUTER_BOUND ( 'NONE', #6721, .T. ) ;
#34175 = CARTESIAN_POINT ( 'NONE',  ( 6.049999999999934097, 12.50000000000000000, -6.083687093685488989 ) ) ;
#34176 = DIRECTION ( 'NONE',  ( -0.000000000000000000, -1.000000000000000000, -0.000000000000000000 ) ) ;
#34177 = EDGE_CURVE ( 'NONE', #70324, #104908, #66456, .T. ) ;
#34178 = FACE_OUTER_BOUND ( 'NONE', #51136, .T. ) ;
#34179 = DIRECTION ( 'NONE',  ( 0.000000000000000000, -0.9999939076577903929, 0.003490651415223739937 ) ) ;
#34180 = AXIS2_PLACEMENT_3D ( 'NONE', #19000, #69397, #28199 ) ;
#34181 = DIRECTION ( 'NONE',  ( 0.000000000000000000, 0.000000000000000000, -1.000000000000000000 ) ) ;
#34182 = VERTEX_POINT ( 'NONE', #14125 ) ;
#34183 = ORIENTED_EDGE ( 'NONE', *, *, #85471, .F. ) ;
#34184 = ORIENTED_EDGE ( 'NONE', *, *, #80140, .T. ) ;
#34185 = CARTESIAN_POINT ( 'NONE',  ( 11.04999999999991012, 12.50000000000000000, 6.841600689897072485 ) ) ;
#34187 = ORIENTED_EDGE ( 'NONE', *, *, #115542, .T. ) ;
#34186 = AXIS2_PLACEMENT_3D ( 'NONE', #108311, #78231, #945 ) ;
#34188 = AXIS2_PLACEMENT_3D ( 'NONE', #118078, #107623, #49372 ) ;
#34189 = CIRCLE ( 'NONE', #117768, 0.09999999999999982514 ) ;
#34191 = ORIENTED_EDGE ( 'NONE', *, *, #125283, .T. ) ;
#34190 = ORIENTED_EDGE ( 'NONE', *, *, #9310, .F. ) ;
#34192 = VERTEX_POINT ( 'NONE', #84160 ) ;
#34193 = AXIS2_PLACEMENT_3D ( 'NONE', #20630, #77590, #49460 ) ;
#34194 = DIRECTION ( 'NONE',  ( 0.000000000000000000, -0.000000000000000000, 1.000000000000000000 ) ) ;
#34195 = LINE ( 'NONE', #91815, #107364 ) ;
#34196 = EDGE_CURVE ( 'NONE', #24753, #26449, #25900, .T. ) ;
#34197 =( NAMED_UNIT ( * ) SI_UNIT ( $, .STERADIAN. ) SOLID_ANGLE_UNIT ( ) );
#34198 = FACE_OUTER_BOUND ( 'NONE', #30082, .T. ) ;
#34199 = CARTESIAN_POINT ( 'NONE',  ( 6.849999999999930367, 12.50000000000000000, -6.148780366869526226 ) ) ;
#34200 = DIRECTION ( 'NONE',  ( 0.000000000000000000, -0.9999939076577903929, 0.003490651415223739937 ) ) ;
#34201 = ORIENTED_EDGE ( 'NONE', *, *, #98229, .T. ) ;
#34202 = CARTESIAN_POINT ( 'NONE',  ( 12.04999999999990479, 2.500000000000000000, -6.495190528383302464 ) ) ;
#34203 = VERTEX_POINT ( 'NONE', #74350 ) ;
#34204 = EDGE_CURVE ( 'NONE', #117086, #103811, #114270, .T. ) ;
#34205 = ORIENTED_EDGE ( 'NONE', *, *, #62571, .T. ) ;
#34206 = ORIENTED_EDGE ( 'NONE', *, *, #117219, .F. ) ;
#34207 = DIRECTION ( 'NONE',  ( 0.000000000000000000, 0.000000000000000000, -1.000000000000000000 ) ) ;
#34208 = CONICAL_SURFACE ( 'NONE', #61391, 0.1000000000000002554, 0.003490658503988666988 ) ;
#34209 = EDGE_CURVE ( 'NONE', #28566, #36792, #25644, .T. ) ;
#34210 = CIRCLE ( 'NONE', #113611, 0.09999999999999982514 ) ;
#34211 = EDGE_LOOP ( 'NONE', ( #3726, #53333, #92426, #107596 ) ) ;
#34212 = ADVANCED_FACE ( 'NONE', ( #116838 ), #88009, .T. ) ;
#34213 = ORIENTED_EDGE ( 'NONE', *, *, #116734, .T. ) ;
#34214 = ADVANCED_FACE ( 'NONE', ( #109622 ), #42386, .T. ) ;
#34215 = ORIENTED_EDGE ( 'NONE', *, *, #47711, .F. ) ;
#34216 = ADVANCED_FACE ( 'NONE', ( #68390 ), #61159, .T. ) ;
#34217 = DIRECTION ( 'NONE',  ( 0.000000000000000000, 1.000000000000000000, 0.000000000000000000 ) ) ;
#34219 = CARTESIAN_POINT ( 'NONE',  ( -2.900000000000030553, 2.500000000000000000, 5.022947341949748790 ) ) ;
#34218 = CONICAL_SURFACE ( 'NONE', #15392, 0.09999999999999999167, 0.003490658503988666988 ) ;
#34220 = CONICAL_SURFACE ( 'NONE', #15393, 0.1000000000000002554, 0.003490658503988666988 ) ;
#34221 = LINE ( 'NONE', #83317, #70935 ) ;
#34222 = DIRECTION ( 'NONE',  ( 0.000000000000000000, 0.000000000000000000, 1.000000000000000000 ) ) ;
#34223 = CARTESIAN_POINT ( 'NONE',  ( 0.8499999999999557909, 12.50000000000000000, -6.430097255199264339 ) ) ;
#34224 = EDGE_CURVE ( 'NONE', #40462, #32144, #125892, .T. ) ;
#34225 = VECTOR ( 'NONE', #2829, 1000.000000000000000 ) ;
#34226 = FACE_OUTER_BOUND ( 'NONE', #92690, .T. ) ;
#34227 = EDGE_CURVE ( 'NONE', #74400, #70390, #7530, .T. ) ;
#34228 = DIRECTION ( 'NONE',  ( -0.000000000000000000, -1.000000000000000000, -0.000000000000000000 ) ) ;
#34229 = CONICAL_SURFACE ( 'NONE', #65497, 0.1000000000000000472, 0.003490658503988666988 ) ;
#34230 = EDGE_CURVE ( 'NONE', #128842, #128031, #99159, .T. ) ;
#34232 = ORIENTED_EDGE ( 'NONE', *, *, #86402, .T. ) ;
#34231 = CIRCLE ( 'NONE', #90639, 0.1000000000000002554 ) ;
#34233 = CARTESIAN_POINT ( 'NONE',  ( 3.349999999999944578, 2.500000000000000000, -5.802370205355749988 ) ) ;
#34234 = VECTOR ( 'NONE', #13346, 1000.000000000000000 ) ;
#34235 = EDGE_CURVE ( 'NONE', #116290, #84812, #73665, .T. ) ;
#34236 = VERTEX_POINT ( 'NONE', #29760 ) ;
#34237 = DIRECTION ( 'NONE',  ( 0.000000000000000000, 1.000000000000000000, 0.000000000000000000 ) ) ;
#34238 = VERTEX_POINT ( 'NONE', #17998 ) ;
#34239 = CIRCLE ( 'NONE', #19645, 0.06509327318403745899 ) ;
#34240 = ADVANCED_FACE ( 'NONE', ( #118138 ), #107682, .T. ) ;
#34241 = ORIENTED_EDGE ( 'NONE', *, *, #85591, .T. ) ;
#34242 = EDGE_CURVE ( 'NONE', #5682, #19872, #77869, .T. ) ;
#34243 = DIRECTION ( 'NONE',  ( 0.000000000000000000, 0.000000000000000000, 1.000000000000000000 ) ) ;
#34244 = CARTESIAN_POINT ( 'NONE',  ( 184.4843750003414016, -8.734944146203032389, -1.604583208406768146E-15 ) ) ;
#34245 = DIRECTION ( 'NONE',  ( 0.000000000000000000, 0.000000000000000000, 1.000000000000000000 ) ) ;
#34246 = VERTEX_POINT ( 'NONE', #127959 ) ;
#34247 = CARTESIAN_POINT ( 'NONE',  ( 9.599999999999917932, 2.500000000000000000, -0.6928203230275541413 ) ) ;
#34248 = ORIENTED_EDGE ( 'NONE', *, *, #23892, .T. ) ;
#34249 = FACE_OUTER_BOUND ( 'NONE', #46866, .T. ) ;
#34250 = DIRECTION ( 'NONE',  ( 0.000000000000000000, 0.000000000000000000, -1.000000000000000000 ) ) ;
#34251 = DIRECTION ( 'NONE',  ( 0.000000000000000000, -0.000000000000000000, 1.000000000000000000 ) ) ;
#34252 = CARTESIAN_POINT ( 'NONE',  ( -10.85000000000000142, 12.50000000000000000, -5.802370205355746435 ) ) ;
#34253 = CIRCLE ( 'NONE', #25823, 0.06509327318403745899 ) ;
#34254 = CARTESIAN_POINT ( 'NONE',  ( 5.849999999999932143, 2.500000000000000000, 1.372243186433545370 ) ) ;
#34255 = ORIENTED_EDGE ( 'NONE', *, *, #88282, .F. ) ;
#34256 = AXIS2_PLACEMENT_3D ( 'NONE', #126670, #87370, #57284 ) ;
#34257 = ORIENTED_EDGE ( 'NONE', *, *, #16119, .F. ) ;
#34258 = AXIS2_PLACEMENT_3D ( 'NONE', #69542, #87243, #48629 ) ;
#34259 = DIRECTION ( 'NONE',  ( -4.274815082592931898E-19, -0.9999939076577903929, -0.003490651415223739937 ) ) ;
#34260 = CARTESIAN_POINT ( 'NONE',  ( 187.5000000000000000, 0.000000000000000000, 0.000000000000000000 ) ) ;
#34261 = AXIS2_PLACEMENT_3D ( 'NONE', #64524, #96547, #85455 ) ;
#34262 = CARTESIAN_POINT ( 'NONE',  ( 185.4218750003414016, 0.000000000000000000, 7.564683531250000925 ) ) ;
#34263 = DIRECTION ( 'NONE',  ( -4.274815082592931898E-19, -0.9999939076577903929, -0.003490651415223739937 ) ) ;
#34264 = DIRECTION ( 'NONE',  ( -0.000000000000000000, -1.000000000000000000, -0.000000000000000000 ) ) ;
#34265 = CARTESIAN_POINT ( 'NONE',  ( 187.5000000000000000, 0.000000000000000000, -5.200000000000000178 ) ) ;
#34266 = AXIS2_PLACEMENT_3D ( 'NONE', #89503, #20121, #48293 ) ;
#34268 = CONICAL_SURFACE ( 'NONE', #115712, 0.1000000000000002554, 0.003490658503988666988 ) ;
#34267 = CARTESIAN_POINT ( 'NONE',  ( 187.5000000000000000, 0.000000000000000000, 0.000000000000000000 ) ) ;
#34269 = EDGE_LOOP ( 'NONE', ( #14418, #39641 ) ) ;
#34270 = CIRCLE ( 'NONE', #7034, 0.06509327318403741736 ) ;
#34271 = CONICAL_SURFACE ( 'NONE', #61460, 0.1000000000000000472, 0.003490658503988666988 ) ;
#34273 = EDGE_CURVE ( 'NONE', #27243, #110807, #78235, .T. ) ;
#34272 = DIRECTION ( 'NONE',  ( -0.000000000000000000, -1.000000000000000000, -0.000000000000000000 ) ) ;
#34274 = CARTESIAN_POINT ( 'NONE',  ( 13.94999999999989804, 2.500000000000000000, 1.718653347947321386 ) ) ;
#34275 = DIRECTION ( 'NONE',  ( -0.000000000000000000, 1.000000000000000000, -0.000000000000000000 ) ) ;
#34276 = ADVANCED_FACE ( 'NONE', ( #6867 ), #48771, .T. ) ;
#34277 = EDGE_LOOP ( 'NONE', ( #3820, #3836, #47819, #69036 ) ) ;
#34278 = CIRCLE ( 'NONE', #7046, 0.06509327318403745899 ) ;
#34279 = CARTESIAN_POINT ( 'NONE',  ( -7.050000000000016698, 2.500000000000000000, -2.265063509461101798 ) ) ;
#34280 = ORIENTED_EDGE ( 'NONE', *, *, #11522, .F. ) ;
#34281 = CIRCLE ( 'NONE', #59333, 0.1000000000000002554 ) ;
#34282 = CIRCLE ( 'NONE', #32141, 0.1000000000000000056 ) ;
#34283 = AXIS2_PLACEMENT_3D ( 'NONE', #17177, #57129, #87225 ) ;
#34284 = CARTESIAN_POINT ( 'NONE',  ( 9.549999999999918998, 2.500000000000000000, -6.595190528383302109 ) ) ;
#34286 = ORIENTED_EDGE ( 'NONE', *, *, #109024, .F. ) ;
#34285 = VECTOR ( 'NONE', #95163, 1000.000000000000000 ) ;
#34287 = DIRECTION ( 'NONE',  ( 0.000000000000000000, 0.000000000000000000, -1.000000000000000000 ) ) ;
#34288 = DIRECTION ( 'NONE',  ( -0.000000000000000000, 1.000000000000000000, -0.000000000000000000 ) ) ;
#34289 = DIRECTION ( 'NONE',  ( 0.000000000000000000, 0.000000000000000000, 1.000000000000000000 ) ) ;
#34290 = CIRCLE ( 'NONE', #63525, 0.06509327318403745899 ) ;
#34291 = ORIENTED_EDGE ( 'NONE', *, *, #52228, .F. ) ;
#34292 = DIRECTION ( 'NONE',  ( -0.000000000000000000, 1.000000000000000000, -0.000000000000000000 ) ) ;
#34293 = PLANE ( 'NONE',  #83014 ) ;
#34294 = ORIENTED_EDGE ( 'NONE', *, *, #125216, .T. ) ;
#34295 = LINE ( 'NONE', #81603, #89178 ) ;
#34296 = EDGE_LOOP ( 'NONE', ( #31000, #89529, #88097, #105867 ) ) ;
#34297 = ORIENTED_EDGE ( 'NONE', *, *, #127978, .F. ) ;
#34298 = DIRECTION ( 'NONE',  ( 0.000000000000000000, 0.000000000000000000, 1.000000000000000000 ) ) ;
#34299 = DIRECTION ( 'NONE',  ( 0.000000000000000000, -0.9999939076577903929, 0.003490651415223739937 ) ) ;
#34301 = DIRECTION ( 'NONE',  ( 0.000000000000000000, 0.000000000000000000, 1.000000000000000000 ) ) ;
#34300 = CIRCLE ( 'NONE', #36361, 0.06509327318403745899 ) ;
#34302 = AXIS2_PLACEMENT_3D ( 'NONE', #76501, #86295, #125577 ) ;
#34303 = ORIENTED_EDGE ( 'NONE', *, *, #9276, .T. ) ;
#34304 = CARTESIAN_POINT ( 'NONE',  ( -7.050000000000013145, 2.500000000000000000, 6.495190528383297135 ) ) ;
#34305 = DIRECTION ( 'NONE',  ( -0.000000000000000000, 1.000000000000000000, -0.000000000000000000 ) ) ;
#34306 = EDGE_LOOP ( 'NONE', ( #27535, #20791 ) ) ;
#34308 = EDGE_CURVE ( 'NONE', #49236, #59553, #115514, .T. ) ;
#34307 = DIRECTION ( 'NONE',  ( -0.000000000000000000, 1.000000000000000000, -0.000000000000000000 ) ) ;
#34310 = CARTESIAN_POINT ( 'NONE',  ( 3.749999999999976907, 12.50000000000000000, 2.230156782645134950 ) ) ;
#34309 = VECTOR ( 'NONE', #85290, 1000.000000000000000 ) ;
#34311 = CONICAL_SURFACE ( 'NONE', #111665, 0.1000000000000002554, 0.003490658503988666988 ) ;
#34312 = VECTOR ( 'NONE', #67712, 1000.000000000000000 ) ;
#34313 = VECTOR ( 'NONE', #111618, 1000.000000000000000 ) ;
#34314 = FACE_OUTER_BOUND ( 'NONE', #60316, .T. ) ;
#34315 = CARTESIAN_POINT ( 'NONE',  ( 2.500000000000002220, 0.4999999999999993339, 10.00000000000000178 ) ) ;
#34316 = CARTESIAN_POINT ( 'NONE',  ( -12.09999999999999432, 2.500000000000000000, 3.637306695894644726 ) ) ;
#34317 = PLANE ( 'NONE',  #103665 ) ;
#34318 = CARTESIAN_POINT ( 'NONE',  ( -11.64999999999999680, 2.500000000000000000, 6.495190528383297135 ) ) ;
#34319 = CONICAL_SURFACE ( 'NONE', #105311, 0.1000000000000002554, 0.003490658503988666988 ) ;
#34320 = CONICAL_SURFACE ( 'NONE', #19640, 0.09999999999999982514, 0.003490658503988666988 ) ;
#34321 = CIRCLE ( 'NONE', #107462, 0.06509327318403745899 ) ;
#34322 = EDGE_LOOP ( 'NONE', ( #94375, #24067 ) ) ;
#34323 = VERTEX_POINT ( 'NONE', #37013 ) ;
#34324 = EDGE_LOOP ( 'NONE', ( #40903, #62774 ) ) ;
#34325 = ORIENTED_EDGE ( 'NONE', *, *, #88728, .F. ) ;
#34326 = CARTESIAN_POINT ( 'NONE',  ( -3.750000000000027534, 2.500000000000000000, -1.472243186433550122 ) ) ;
#34327 = DIRECTION ( 'NONE',  ( 0.000000000000000000, 0.000000000000000000, -1.000000000000000000 ) ) ;
#34328 = ADVANCED_FACE ( 'NONE', ( #67075 ), #46476, .T. ) ;
#34329 = CARTESIAN_POINT ( 'NONE',  ( 8.149999999999923972, 12.50000000000000000, 1.818653347947321475 ) ) ;
#34330 = ORIENTED_EDGE ( 'NONE', *, *, #55153, .F. ) ;
#34331 = FACE_BOUND ( 'NONE', #80032, .T. ) ;
#34332 = ADVANCED_FACE ( 'NONE', ( #17339 ), #29136, .T. ) ;
#34333 = DIRECTION ( 'NONE',  ( 0.000000000000000000, 0.000000000000000000, -1.000000000000000000 ) ) ;
#34334 = DIRECTION ( 'NONE',  ( -0.000000000000000000, 1.000000000000000000, -0.000000000000000000 ) ) ;
#34335 = DIRECTION ( 'NONE',  ( -0.000000000000000000, -1.000000000000000000, -0.000000000000000000 ) ) ;
#34336 = CARTESIAN_POINT ( 'NONE',  ( 0.6499999999999561684, 2.500000000000000000, -2.511473670974877948 ) ) ;
#34337 = LINE ( 'NONE', #14650, #107809 ) ;
#34338 = CONICAL_SURFACE ( 'NONE', #11334, 0.1000000000000000472, 0.003490658503988666988 ) ;
#34339 = CARTESIAN_POINT ( 'NONE',  ( 14.79999999999989413, 12.50000000000000000, -0.3464101615137782364 ) ) ;
#34340 = CARTESIAN_POINT ( 'NONE',  ( 0.8499999999999557909, 12.50000000000000000, -6.495190528383302464 ) ) ;
#34341 = DIRECTION ( 'NONE',  ( 0.000000000000000000, 1.000000000000000000, 0.000000000000000000 ) ) ;
#34342 = EDGE_CURVE ( 'NONE', #80247, #16543, #96641, .T. ) ;
#34343 = CARTESIAN_POINT ( 'NONE',  ( -11.44999999999999751, 2.500000000000000000, 1.818653347947321475 ) ) ;
#34344 = CIRCLE ( 'NONE', #86547, 0.09999999999999982514 ) ;
#34345 = CARTESIAN_POINT ( 'NONE',  ( 8.949999999999915801, 12.50000000000000000, 6.776507416713035248 ) ) ;
#34346 = ORIENTED_EDGE ( 'NONE', *, *, #11627, .T. ) ;
#34347 = VERTEX_POINT ( 'NONE', #127331 ) ;
#34348 = ORIENTED_EDGE ( 'NONE', *, *, #95197, .F. ) ;
#34349 = VERTEX_POINT ( 'NONE', #37663 ) ;
#34350 = EDGE_LOOP ( 'NONE', ( #39642, #20580, #124664, #96789 ) ) ;
#34351 = CARTESIAN_POINT ( 'NONE',  ( 4.599999999999938360, 2.500000000000000000, -0.6928203230275541413 ) ) ;
#34352 = ORIENTED_EDGE ( 'NONE', *, *, #19166, .T. ) ;
#34353 = ORIENTED_EDGE ( 'NONE', *, *, #14169, .T. ) ;
#34354 = AXIS2_PLACEMENT_3D ( 'NONE', #79698, #90144, #120913 ) ;
#34355 = DIRECTION ( 'NONE',  ( -0.000000000000000000, -1.000000000000000000, -0.000000000000000000 ) ) ;
#34356 = DIRECTION ( 'NONE',  ( 0.000000000000000000, 0.000000000000000000, 1.000000000000000000 ) ) ;
#34357 = LINE ( 'NONE', #106299, #76110 ) ;
#34358 = CARTESIAN_POINT ( 'NONE',  ( 8.149999999999923972, 2.500000000000000000, -6.148780366869526226 ) ) ;
#34359 = ORIENTED_EDGE ( 'NONE', *, *, #35425, .T. ) ;
#34360 = CARTESIAN_POINT ( 'NONE',  ( -5.400000000000020783, 2.500000000000000000, 0.5928203230275495006 ) ) ;
#34361 = ORIENTED_EDGE ( 'NONE', *, *, #33258, .F. ) ;
#34362 = AXIS2_PLACEMENT_3D ( 'NONE', #2867, #53267, #32988 ) ;
#34363 = EDGE_CURVE ( 'NONE', #21550, #63883, #128064, .T. ) ;
#34364 = ORIENTED_EDGE ( 'NONE', *, *, #106305, .F. ) ;
#34366 = ORIENTED_EDGE ( 'NONE', *, *, #124911, .F. ) ;
#34365 = CARTESIAN_POINT ( 'NONE',  ( 3.099999999999944134, 2.500000000000000000, 4.676537180435972552 ) ) ;
#34367 = LINE ( 'NONE', #76216, #10735 ) ;
#34368 = ORIENTED_EDGE ( 'NONE', *, *, #79558, .T. ) ;
#34369 = ADVANCED_FACE ( 'NONE', ( #20591 ), #73755, .T. ) ;
#34370 = VERTEX_POINT ( 'NONE', #21224 ) ;
#34371 = ADVANCED_FACE ( 'NONE', ( #73380 ), #59387, .T. ) ;
#34372 = FACE_OUTER_BOUND ( 'NONE', #118359, .T. ) ;
#34374 = AXIS2_PLACEMENT_3D ( 'NONE', #89664, #26873, #56955 ) ;
#34373 = CARTESIAN_POINT ( 'NONE',  ( 10.59999999999990905, 12.50000000000000000, 4.611443907251934426 ) ) ;
#34375 = FACE_OUTER_BOUND ( 'NONE', #119674, .T. ) ;
#34376 = CIRCLE ( 'NONE', #82489, 0.06509327318403745899 ) ;
#34377 = DIRECTION ( 'NONE',  ( 0.000000000000000000, 0.000000000000000000, 1.000000000000000000 ) ) ;
#34378 = ADVANCED_FACE ( 'NONE', ( #80808 ), #13158, .T. ) ;
#34379 = ADVANCED_FACE ( 'NONE', ( #53115 ), #100436, .T. ) ;
#34380 = CARTESIAN_POINT ( 'NONE',  ( -10.40000000000000213, 12.50000000000000000, -2.276824562219559311E-15 ) ) ;
#34381 = AXIS2_PLACEMENT_3D ( 'NONE', #2746, #81952, #32883 ) ;
#34382 = EDGE_CURVE ( 'NONE', #100479, #93758, #115614, .T. ) ;
#34383 = EDGE_CURVE ( 'NONE', #55744, #113395, #14450, .T. ) ;
#34384 = VERTEX_POINT ( 'NONE', #10127 ) ;
#34385 = CONICAL_SURFACE ( 'NONE', #71940, 0.09999999999999982514, 0.003490658503988666988 ) ;
#34386 = DIRECTION ( 'NONE',  ( -4.274815082592931898E-19, -0.9999939076577903929, -0.003490651415223739937 ) ) ;
#34387 = ORIENTED_EDGE ( 'NONE', *, *, #79974, .T. ) ;
#34388 = CARTESIAN_POINT ( 'NONE',  ( -3.550000000000028244, 2.500000000000000000, 2.411473670974873862 ) ) ;
#34389 = ADVANCED_FACE ( 'NONE', ( #24293 ), #86271, .T. ) ;
#34390 = ORIENTED_EDGE ( 'NONE', *, *, #51772, .T. ) ;
#34391 = DIRECTION ( 'NONE',  ( 0.000000000000000000, 0.000000000000000000, 1.000000000000000000 ) ) ;
#34392 = DIRECTION ( 'NONE',  ( 0.000000000000000000, 0.000000000000000000, 1.000000000000000000 ) ) ;
#34393 = CARTESIAN_POINT ( 'NONE',  ( -7.100000000000017408, 2.500000000000000000, -3.537306695894649966 ) ) ;
#34394 = PLANE ( 'NONE',  #79405 ) ;
#34395 = EDGE_LOOP ( 'NONE', ( #115180, #75181 ) ) ;
#34396 = EDGE_CURVE ( 'NONE', #85672, #21815, #17303, .T. ) ;
#34397 = FILL_AREA_STYLE_COLOUR ( '', #19369 ) ;
#34398 = AXIS2_PLACEMENT_3D ( 'NONE', #111295, #59674, #21658 ) ;
#34400 = DIRECTION ( 'NONE',  ( 0.000000000000000000, 1.000000000000000000, 0.000000000000000000 ) ) ;
#34399 = CONICAL_SURFACE ( 'NONE', #7171, 0.1000000000000002554, 0.003490658503988666988 ) ;
#34401 = ORIENTED_EDGE ( 'NONE', *, *, #120349, .F. ) ;
#34402 = ORIENTED_EDGE ( 'NONE', *, *, #85379, .F. ) ;
#34403 = AXIS2_PLACEMENT_3D ( 'NONE', #32470, #83485, #1039 ) ;
#34404 = AXIS2_PLACEMENT_3D ( 'NONE', #25962, #45610, #113039 ) ;
#34405 = ORIENTED_EDGE ( 'NONE', *, *, #53414, .F. ) ;
#34406 = PLANE ( 'NONE',  #35336 ) ;
#34407 = DIRECTION ( 'NONE',  ( -0.000000000000000000, 1.000000000000000000, -0.000000000000000000 ) ) ;
#34408 = CARTESIAN_POINT ( 'NONE',  ( 184.6510416670080588, 4.367472073101518859, -7.564683531249999149 ) ) ;
#34409 = FACE_OUTER_BOUND ( 'NONE', #36314, .T. ) ;
#34410 = CIRCLE ( 'NONE', #67827, 0.06509327318403741736 ) ;
#34411 = CARTESIAN_POINT ( 'NONE',  ( 7.099999999999927702, 2.500000000000000000, 5.122947341949749323 ) ) ;
#34412 = CIRCLE ( 'NONE', #122223, 2.250000000000001776 ) ;
#34413 = VECTOR ( 'NONE', #25067, 1000.000000000000000 ) ;
#34414 = CARTESIAN_POINT ( 'NONE',  ( 11.24999999999994493, 2.500000000000000000, -2.265063509461101798 ) ) ;
#34415 = EDGE_LOOP ( 'NONE', ( #50223, #38169 ) ) ;
#34416 = AXIS2_PLACEMENT_3D ( 'NONE', #31973, #61438, #3152 ) ;
#34417 = LINE ( 'NONE', #63207, #52658 ) ;
#34418 = CONICAL_SURFACE ( 'NONE', #61602, 0.1000000000000000472, 0.003490658503988666988 ) ;
#34419 = VERTEX_POINT ( 'NONE', #63579 ) ;
#34420 = AXIS2_PLACEMENT_3D ( 'NONE', #37763, #76408, #27286 ) ;
#34421 = DIRECTION ( 'NONE',  ( -0.000000000000000000, 1.000000000000000000, -0.000000000000000000 ) ) ;
#34422 = CARTESIAN_POINT ( 'NONE',  ( -2.100000000000033396, 2.500000000000000000, -0.6928203230275542523 ) ) ;
#34423 = DIRECTION ( 'NONE',  ( 0.000000000000000000, 0.000000000000000000, -1.000000000000000000 ) ) ;
#34424 = ORIENTED_EDGE ( 'NONE', *, *, #30396, .T. ) ;
#34425 = EDGE_CURVE ( 'NONE', #80466, #93509, #48744, .T. ) ;
#34426 = FACE_OUTER_BOUND ( 'NONE', #104073, .T. ) ;
#34427 = CARTESIAN_POINT ( 'NONE',  ( -10.00000000000000533, 2.500000000000000000, 5.122947341949749323 ) ) ;
#34428 = AXIS2_PLACEMENT_3D ( 'NONE', #31181, #99907, #118895 ) ;
#34429 = ORIENTED_EDGE ( 'NONE', *, *, #48269, .T. ) ;
#34430 = DIRECTION ( 'NONE',  ( 0.000000000000000000, 0.000000000000000000, 1.000000000000000000 ) ) ;
#34431 = EDGE_CURVE ( 'NONE', #38354, #33550, #82186, .T. ) ;
#34432 = VERTEX_POINT ( 'NONE', #34775 ) ;
#34433 = EDGE_LOOP ( 'NONE', ( #59984, #54763 ) ) ;
#34434 = DIRECTION ( 'NONE',  ( -4.274815082592931898E-19, -0.9999939076577903929, -0.003490651415223739937 ) ) ;
#34435 = ORIENTED_EDGE ( 'NONE', *, *, #104993, .F. ) ;
#34436 = CARTESIAN_POINT ( 'NONE',  ( 17.17539648375908357, 2.541523116374457825, -5.507477068181845681 ) ) ;
#34437 = DIRECTION ( 'NONE',  ( -0.000000000000000000, -1.000000000000000000, -0.000000000000000000 ) ) ;
#34438 = AXIS2_PLACEMENT_3D ( 'NONE', #25271, #76333, #74393 ) ;
#34439 = CARTESIAN_POINT ( 'NONE',  ( 10.59999999999990905, 12.50000000000000000, 4.676537180435972552 ) ) ;
#34440 = AXIS2_PLACEMENT_3D ( 'NONE', #10448, #108647, #110583 ) ;
#34441 = ORIENTED_EDGE ( 'NONE', *, *, #79304, .T. ) ;
#34442 = LINE ( 'NONE', #14750, #121335 ) ;
#34444 = ORIENTED_EDGE ( 'NONE', *, *, #70093, .T. ) ;
#34443 = DIRECTION ( 'NONE',  ( -0.000000000000000000, 1.000000000000000000, -0.000000000000000000 ) ) ;
#34445 = CARTESIAN_POINT ( 'NONE',  ( 7.699999999999923794, 12.50000000000000000, -0.3464101615137783474 ) ) ;
#34446 = FACE_OUTER_BOUND ( 'NONE', #47370, .T. ) ;
#34447 = ORIENTED_EDGE ( 'NONE', *, *, #115661, .F. ) ;
#34448 = CONICAL_SURFACE ( 'NONE', #105546, 0.09999999999999982514, 0.003490658503988666988 ) ;
#34449 = ORIENTED_EDGE ( 'NONE', *, *, #85576, .F. ) ;
#34450 = CIRCLE ( 'NONE', #987, 0.06509327318403745899 ) ;
#34451 = ORIENTED_EDGE ( 'NONE', *, *, #33628, .T. ) ;
#34452 = DIRECTION ( 'NONE',  ( 0.000000000000000000, -0.000000000000000000, 1.000000000000000000 ) ) ;
#34453 = DIRECTION ( 'NONE',  ( -0.000000000000000000, 1.000000000000000000, -0.000000000000000000 ) ) ;
#34454 = CARTESIAN_POINT ( 'NONE',  ( 2.299999999999948752, 12.50000000000000000, -3.918623584224389056 ) ) ;
#34455 = FACE_BOUND ( 'NONE', #62240, .T. ) ;
#34456 = VERTEX_POINT ( 'NONE', #44580 ) ;
#34457 = CARTESIAN_POINT ( 'NONE',  ( 186.9427083336747160, -6.551208109652278289, 3.782341765624995134 ) ) ;
#34458 = DIRECTION ( 'NONE',  ( -0.000000000000000000, -1.000000000000000000, -0.000000000000000000 ) ) ;
#34459 = CARTESIAN_POINT ( 'NONE',  ( -11.69999999999999929, 2.500000000000000000, -4.230127018922199333 ) ) ;
#34460 = EDGE_CURVE ( 'NONE', #106953, #54196, #29862, .T. ) ;
#34462 = AXIS2_PLACEMENT_3D ( 'NONE', #58916, #117158, #27490 ) ;
#34461 = DIRECTION ( 'NONE',  ( 0.000000000000000000, 1.000000000000000000, 0.000000000000000000 ) ) ;
#34463 = CONICAL_SURFACE ( 'NONE', #122193, 0.1000000000000002554, 0.003490658503988666988 ) ;
#34464 = CARTESIAN_POINT ( 'NONE',  ( 5.599999999999934808, 2.500000000000000000, -4.776537180435978414 ) ) ;
#34465 = DIRECTION ( 'NONE',  ( 0.000000000000000000, 0.000000000000000000, 1.000000000000000000 ) ) ;
#34466 = AXIS2_PLACEMENT_3D ( 'NONE', #92768, #94045, #2417 ) ;
#34467 = CARTESIAN_POINT ( 'NONE',  ( 0.3999999999999568345, 2.500000000000000000, -5.022947341949754119 ) ) ;
#34468 = AXIS2_PLACEMENT_3D ( 'NONE', #127346, #108956, #10140 ) ;
#34469 = ADVANCED_FACE ( 'NONE', ( #50071 ), #96739, .T. ) ;
#34470 = DIRECTION ( 'NONE',  ( 0.000000000000000000, 0.000000000000000000, 1.000000000000000000 ) ) ;
#34471 = EDGE_LOOP ( 'NONE', ( #91487, #108441, #68860, #18521 ) ) ;
#34472 = VERTEX_POINT ( 'NONE', #70333 ) ;
#34473 = ORIENTED_EDGE ( 'NONE', *, *, #245, .F. ) ;
#34474 = EDGE_LOOP ( 'NONE', ( #35974, #23621 ) ) ;
#34475 = EDGE_LOOP ( 'NONE', ( #51389, #33660, #117029, #109755 ) ) ;
#34476 = DIRECTION ( 'NONE',  ( -0.000000000000000000, -1.000000000000000000, -0.000000000000000000 ) ) ;
#34477 = EDGE_CURVE ( 'NONE', #94312, #31579, #50686, .T. ) ;
#34478 = CARTESIAN_POINT ( 'NONE',  ( 7.299999999999927880, 12.50000000000000000, -4.741630453620015118 ) ) ;
#34479 = ORIENTED_EDGE ( 'NONE', *, *, #20566, .T. ) ;
#34480 = FACE_BOUND ( 'NONE', #3661, .T. ) ;
#34481 = EDGE_CURVE ( 'NONE', #79643, #37274, #128157, .T. ) ;
#34482 = DIRECTION ( 'NONE',  ( 0.000000000000000000, 0.000000000000000000, 1.000000000000000000 ) ) ;
#34483 = AXIS2_PLACEMENT_3D ( 'NONE', #26810, #8436, #55621 ) ;
#34484 = EDGE_CURVE ( 'NONE', #107557, #84136, #71716, .T. ) ;
#34485 = FACE_OUTER_BOUND ( 'NONE', #115085, .T. ) ;
#34486 = AXIS2_PLACEMENT_3D ( 'NONE', #83500, #23258, #123398 ) ;
#34488 = EDGE_LOOP ( 'NONE', ( #3482, #37452, #116047, #94557 ) ) ;
#34487 = CONICAL_SURFACE ( 'NONE', #19803, 0.1000000000000002554, 0.003490658503988666988 ) ;
#34489 = AXIS2_PLACEMENT_3D ( 'NONE', #46892, #67807, #106443 ) ;
#34490 = DIRECTION ( 'NONE',  ( 0.000000000000000000, 0.000000000000000000, 1.000000000000000000 ) ) ;
#34491 = PLANE ( 'NONE',  #128545 ) ;
#34492 = EDGE_CURVE ( 'NONE', #81402, #109700, #11058, .T. ) ;
#34493 = CARTESIAN_POINT ( 'NONE',  ( -2.950000000000033484, 2.500000000000000000, -6.495190528383302464 ) ) ;
#34494 = ORIENTED_EDGE ( 'NONE', *, *, #99087, .F. ) ;
#34495 = DIRECTION ( 'NONE',  ( 0.000000000000000000, 1.000000000000000000, 0.000000000000000000 ) ) ;
#34496 = EDGE_LOOP ( 'NONE', ( #60550, #95055, #12230, #88190 ) ) ;
#34497 = AXIS2_PLACEMENT_3D ( 'NONE', #3257, #121091, #43199 ) ;
#34498 = CIRCLE ( 'NONE', #59556, 0.1000000000000002554 ) ;
#34499 = ORIENTED_EDGE ( 'NONE', *, *, #54173, .F. ) ;
#34500 = ORIENTED_EDGE ( 'NONE', *, *, #82769, .T. ) ;
#34501 = DIRECTION ( 'NONE',  ( 0.000000000000000000, 0.000000000000000000, 1.000000000000000000 ) ) ;
#34502 = AXIS2_PLACEMENT_3D ( 'NONE', #122312, #32659, #13617 ) ;
#34503 = FACE_OUTER_BOUND ( 'NONE', #73093, .T. ) ;
#34504 = LINE ( 'NONE', #114326, #4905 ) ;
#34505 = VERTEX_POINT ( 'NONE', #96890 ) ;
#34506 = CARTESIAN_POINT ( 'NONE',  ( 5.399999999999936406, 2.500000000000000000, -3.737306695894649700 ) ) ;
#34507 = CONICAL_SURFACE ( 'NONE', #74198, 0.1000000000000002554, 0.003490658503988666988 ) ;
#34508 = CIRCLE ( 'NONE', #51228, 0.09999999999999982514 ) ;
#34509 = CARTESIAN_POINT ( 'NONE',  ( -8.550000000000013145, 12.50000000000000000, -1.818653347947326138 ) ) ;
#34510 = DIRECTION ( 'NONE',  ( 0.000000000000000000, 1.000000000000000000, 0.000000000000000000 ) ) ;
#34511 = CARTESIAN_POINT ( 'NONE',  ( 185.3645833340161175, -6.668395609140180369, 3.849999999999994760 ) ) ;
#34514 = VERTEX_POINT ( 'NONE', #6537 ) ;
#34513 = VECTOR ( 'NONE', #126479, 1000.000000000000000 ) ;
#34512 = CARTESIAN_POINT ( 'NONE',  ( -5.850000000000019185, 12.50000000000000000, 2.165063509461097713 ) ) ;
#34515 = CARTESIAN_POINT ( 'NONE',  ( -12.09999999999999609, 2.500000000000000000, -3.737306695894647035 ) ) ;
#34516 = ORIENTED_EDGE ( 'NONE', *, *, #97301, .F. ) ;
#34517 = CARTESIAN_POINT ( 'NONE',  ( 1.249999999999952038, 2.500000000000000000, -1.472243186433550122 ) ) ;
#34518 = ORIENTED_EDGE ( 'NONE', *, *, #3044, .F. ) ;
#34519 = EDGE_LOOP ( 'NONE', ( #50927, #62622, #113791, #13421 ) ) ;
#34520 = DIRECTION ( 'NONE',  ( -0.000000000000000000, -1.000000000000000000, -0.000000000000000000 ) ) ;
#34521 = DIRECTION ( 'NONE',  ( -0.000000000000000000, -1.000000000000000000, -0.000000000000000000 ) ) ;
#34522 = DIRECTION ( 'NONE',  ( 0.000000000000000000, 0.000000000000000000, 1.000000000000000000 ) ) ;
#34523 = DIRECTION ( 'NONE',  ( 0.000000000000000000, 0.000000000000000000, 1.000000000000000000 ) ) ;
#34524 = CARTESIAN_POINT ( 'NONE',  ( 184.4999999999999716, -4.098321783458930945, -6.521161088353083279 ) ) ;
#34525 = VECTOR ( 'NONE', #78103, 1000.000000000000000 ) ;
#34526 = EDGE_LOOP ( 'NONE', ( #122032, #48125, #106749, #80097 ) ) ;
#34528 = EDGE_CURVE ( 'NONE', #56626, #106131, #16374, .T. ) ;
#34527 = ORIENTED_EDGE ( 'NONE', *, *, #125920, .T. ) ;
#34529 = FACE_OUTER_BOUND ( 'NONE', #49078, .T. ) ;
#34530 = CARTESIAN_POINT ( 'NONE',  ( 1.849999999999950129, 12.50000000000000000, -6.776507416713040577 ) ) ;
#34532 = ADVANCED_FACE ( 'NONE', ( #27486 ), #46497, .T. ) ;
#34531 = CARTESIAN_POINT ( 'NONE',  ( 3.949999999999940670, 2.500000000000000000, 1.818653347947321475 ) ) ;
#34533 = EDGE_LOOP ( 'NONE', ( #12915, #77634 ) ) ;
#34534 = ORIENTED_EDGE ( 'NONE', *, *, #61817, .T. ) ;
#34535 = ADVANCED_FACE ( 'NONE', ( #127646 ), #35410, .T. ) ;
#34536 = LINE ( 'NONE', #64612, #12290 ) ;
#34537 = ADVANCED_FACE ( 'NONE', ( #125069 ), #52843, .T. ) ;
#34538 = CIRCLE ( 'NONE', #122357, 0.06509327318403741736 ) ;
#34539 = EDGE_CURVE ( 'NONE', #61976, #20692, #44521, .T. ) ;
#34540 = ORIENTED_EDGE ( 'NONE', *, *, #36591, .T. ) ;
#34542 = AXIS2_PLACEMENT_3D ( 'NONE', #90790, #121525, #52796 ) ;
#34541 = CARTESIAN_POINT ( 'NONE',  ( -12.89999999999999147, 12.50000000000000000, -4.957854068765714217 ) ) ;
#34543 = CARTESIAN_POINT ( 'NONE',  ( 6.699999999999930012, 12.50000000000000000, 4.330127018922196314 ) ) ;
#34544 = ORIENTED_EDGE ( 'NONE', *, *, #73933, .F. ) ;
#34545 = FACE_OUTER_BOUND ( 'NONE', #16462, .T. ) ;
#34546 = EDGE_CURVE ( 'NONE', #110045, #101913, #121888, .T. ) ;
#34547 = CARTESIAN_POINT ( 'NONE',  ( -8.350000000000010303, 2.500000000000000000, 6.495190528383297135 ) ) ;
#34548 = CARTESIAN_POINT ( 'NONE',  ( -12.49999999999999467, 12.50000000000000000, 0.6928203230275535862 ) ) ;
#34549 = DIRECTION ( 'NONE',  ( -0.000000000000000000, 1.000000000000000000, -0.000000000000000000 ) ) ;
#34550 = ORIENTED_EDGE ( 'NONE', *, *, #94189, .T. ) ;
#34551 = EDGE_CURVE ( 'NONE', #18774, #127039, #50954, .T. ) ;
#34552 = AXIS2_PLACEMENT_3D ( 'NONE', #28963, #99628, #98977 ) ;
#34553 = FACE_OUTER_BOUND ( 'NONE', #96154, .T. ) ;
#34554 = EDGE_CURVE ( 'NONE', #31546, #45780, #2646, .T. ) ;
#34556 = AXIS2_PLACEMENT_3D ( 'NONE', #35913, #75828, #115756 ) ;
#34555 = DIRECTION ( 'NONE',  ( 0.000000000000000000, 1.000000000000000000, 0.000000000000000000 ) ) ;
#34557 = VERTEX_POINT ( 'NONE', #77261 ) ;
#34558 = ORIENTED_EDGE ( 'NONE', *, *, #31268, .T. ) ;
#34559 = DIRECTION ( 'NONE',  ( -0.000000000000000000, -1.000000000000000000, -0.000000000000000000 ) ) ;
#34560 = DIRECTION ( 'NONE',  ( -0.000000000000000000, -1.000000000000000000, -0.000000000000000000 ) ) ;
#34561 = CARTESIAN_POINT ( 'NONE',  ( -11.69999999999999929, 2.500000000000000000, -0.09999999999999827083 ) ) ;
#34562 = DIRECTION ( 'NONE',  ( -0.000000000000000000, 1.000000000000000000, -0.000000000000000000 ) ) ;
#34563 = LINE ( 'NONE', #74466, #123809 ) ;
#34564 = VECTOR ( 'NONE', #45567, 1000.000000000000000 ) ;
#34565 = PLANE ( 'NONE',  #115757 ) ;
#34566 = DIRECTION ( 'NONE',  ( 0.000000000000000000, 0.000000000000000000, 1.000000000000000000 ) ) ;
#34567 = CARTESIAN_POINT ( 'NONE',  ( 162.5000000000000000, 0.5000000000000000000, -7.500000000000005329 ) ) ;
#34568 = DIRECTION ( 'NONE',  ( 0.000000000000000000, 0.000000000000000000, 1.000000000000000000 ) ) ;
#34569 = ADVANCED_FACE ( 'NONE', ( #85135 ), #123929, .T. ) ;
#34570 = DIRECTION ( 'NONE',  ( 0.000000000000000000, 0.000000000000000000, 1.000000000000000000 ) ) ;
#34571 = ORIENTED_EDGE ( 'NONE', *, *, #11569, .F. ) ;
#34572 = ORIENTED_EDGE ( 'NONE', *, *, #109163, .T. ) ;
#34573 = EDGE_LOOP ( 'NONE', ( #72766, #70506, #97060, #26551 ) ) ;
#34574 = ORIENTED_EDGE ( 'NONE', *, *, #77661, .F. ) ;
#34575 = CARTESIAN_POINT ( 'NONE',  ( 8.749999999999923617, 12.50000000000000000, 1.537336459617582918 ) ) ;
#34576 = AXIS2_PLACEMENT_3D ( 'NONE', #119832, #31464, #70735 ) ;
#34577 = CARTESIAN_POINT ( 'NONE',  ( 8.749999999999920064, 12.50000000000000000, 5.802370205355744659 ) ) ;
#34578 = LINE ( 'NONE', #78198, #31305 ) ;
#34579 = ORIENTED_EDGE ( 'NONE', *, *, #9429, .T. ) ;
#34580 = CARTESIAN_POINT ( 'NONE',  ( 9.999999999999948486, 12.50000000000000000, 4.330127018922196314 ) ) ;
#34581 = VECTOR ( 'NONE', #113756, 1000.000000000000000 ) ;
#34582 = AXIS2_PLACEMENT_3D ( 'NONE', #116154, #26508, #114865 ) ;
#34583 = CARTESIAN_POINT ( 'NONE',  ( -0.4000000000000404898, 2.500000000000000000, 5.122947341949749323 ) ) ;
#34585 = ORIENTED_EDGE ( 'NONE', *, *, #95097, .F. ) ;
#34584 = CARTESIAN_POINT ( 'NONE',  ( -5.400000000000020783, 2.500000000000000000, 0.6928203230275494784 ) ) ;
#34586 = AXIS2_PLACEMENT_3D ( 'NONE', #89078, #119818, #67467 ) ;
#34587 = PLANE ( 'NONE',  #49519 ) ;
#34588 = LINE ( 'NONE', #88658, #56289 ) ;
#34589 = ORIENTED_EDGE ( 'NONE', *, *, #13458, .F. ) ;
#34590 = TOROIDAL_SURFACE ( 'NONE', #1111, 8.199999999999999289, 0.5000000000000000000 ) ;
#34591 = EDGE_CURVE ( 'NONE', #114219, #22468, #104758, .T. ) ;
#34592 = CIRCLE ( 'NONE', #22066, 0.1000000000000002554 ) ;
#34593 = VECTOR ( 'NONE', #57056, 1000.000000000000000 ) ;
#34594 = VERTEX_POINT ( 'NONE', #5281 ) ;
#34595 = VERTEX_POINT ( 'NONE', #47809 ) ;
#34596 = EDGE_LOOP ( 'NONE', ( #9918, #100791, #42568, #47203 ) ) ;
#34597 = DIRECTION ( 'NONE',  ( -0.000000000000000000, 1.000000000000000000, -0.000000000000000000 ) ) ;
#34598 = VECTOR ( 'NONE', #102503, 1000.000000000000000 ) ;
#34599 = CARTESIAN_POINT ( 'NONE',  ( -7.500000000000015099, 2.500000000000000000, -5.122947341949753763 ) ) ;
#34600 = DIRECTION ( 'NONE',  ( 0.000000000000000000, 1.000000000000000000, 0.000000000000000000 ) ) ;
#34601 = CONICAL_SURFACE ( 'NONE', #111952, 0.1000000000000000472, 0.003490658503988666988 ) ;
#34602 = DIRECTION ( 'NONE',  ( 0.000000000000000000, 0.000000000000000000, 1.000000000000000000 ) ) ;
#34603 = CIRCLE ( 'NONE', #47193, 3.000000000000000000 ) ;
#34604 = ORIENTED_EDGE ( 'NONE', *, *, #1535, .T. ) ;
#34605 = CIRCLE ( 'NONE', #13726, 0.06509327318403745899 ) ;
#34607 = VECTOR ( 'NONE', #23601, 1000.000000000000000 ) ;
#34606 = DIRECTION ( 'NONE',  ( 0.000000000000000000, 0.000000000000000000, 1.000000000000000000 ) ) ;
#34608 = EDGE_LOOP ( 'NONE', ( #93033, #126995 ) ) ;
#34609 = DIRECTION ( 'NONE',  ( 1.000000000000000000, 0.000000000000000000, 0.000000000000000000 ) ) ;
#34610 = DIRECTION ( 'NONE',  ( 0.000000000000000000, 0.000000000000000000, 1.000000000000000000 ) ) ;
#34611 = DIRECTION ( 'NONE',  ( 0.000000000000000000, 1.000000000000000000, 0.000000000000000000 ) ) ;
#34612 = FACE_OUTER_BOUND ( 'NONE', #66922, .T. ) ;
#34613 = EDGE_LOOP ( 'NONE', ( #120287, #95862, #16263, #58295 ) ) ;
#34614 = VERTEX_POINT ( 'NONE', #85775 ) ;
#34615 = ORIENTED_EDGE ( 'NONE', *, *, #58700, .T. ) ;
#34616 = DIRECTION ( 'NONE',  ( -0.000000000000000000, -1.000000000000000000, -0.000000000000000000 ) ) ;
#34617 = CARTESIAN_POINT ( 'NONE',  ( 8.749999999999957367, 2.500000000000000000, 2.165063509461097713 ) ) ;
#34618 = CARTESIAN_POINT ( 'NONE',  ( 4.149999999999941735, 12.50000000000000000, -5.802370205355749988 ) ) ;
#34619 = FACE_BOUND ( 'NONE', #43257, .T. ) ;
#34620 = CARTESIAN_POINT ( 'NONE',  ( 1.649999999999950617, 12.50000000000000000, -2.165063509461101710 ) ) ;
#34621 = VECTOR ( 'NONE', #50405, 1000.000000000000000 ) ;
#34622 = DIRECTION ( 'NONE',  ( 0.000000000000000000, 0.000000000000000000, -1.000000000000000000 ) ) ;
#34623 = FACE_OUTER_BOUND ( 'NONE', #45983, .T. ) ;
#34624 = DIRECTION ( 'NONE',  ( 0.000000000000000000, 0.000000000000000000, -1.000000000000000000 ) ) ;
#34625 = VECTOR ( 'NONE', #52498, 1000.000000000000000 ) ;
#34626 = LINE ( 'NONE', #95460, #119834 ) ;
#34627 = DIRECTION ( 'NONE',  ( 0.000000000000000000, 0.000000000000000000, -1.000000000000000000 ) ) ;
#34628 = ORIENTED_EDGE ( 'NONE', *, *, #68294, .T. ) ;
#34629 = CIRCLE ( 'NONE', #15814, 0.1000000000000000472 ) ;
#34630 = AXIS2_PLACEMENT_3D ( 'NONE', #34467, #124110, #114294 ) ;
#34631 = EDGE_CURVE ( 'NONE', #92907, #81402, #37974, .T. ) ;
#34632 = CARTESIAN_POINT ( 'NONE',  ( 13.09999999999990195, 12.50000000000000000, -4.048810130592463530 ) ) ;
#34633 = EDGE_LOOP ( 'NONE', ( #75603, #100190, #66654, #16193 ) ) ;
#34634 = ORIENTED_EDGE ( 'NONE', *, *, #12967, .F. ) ;
#34635 = VERTEX_POINT ( 'NONE', #55038 ) ;
#34636 = ORIENTED_EDGE ( 'NONE', *, *, #33478, .F. ) ;
#34637 = ADVANCED_FACE ( 'NONE', ( #94973 ), #45229, .T. ) ;
#34638 = CARTESIAN_POINT ( 'NONE',  ( 11.04999999999990834, 12.50000000000000000, 1.818653347947321475 ) ) ;
#34639 = FACE_BOUND ( 'NONE', #77585, .T. ) ;
#34640 = ADVANCED_FACE ( 'NONE', ( #5912 ), #69558, .T. ) ;
#34641 = DIRECTION ( 'NONE',  ( 0.000000000000000000, -0.9999939076577903929, 0.003490651415223739937 ) ) ;
#34642 = AXIS2_PLACEMENT_3D ( 'NONE', #98171, #120407, #30107 ) ;
#34643 = AXIS2_PLACEMENT_3D ( 'NONE', #24013, #113026, #46221 ) ;
#34644 = EDGE_CURVE ( 'NONE', #72427, #80727, #29456, .T. ) ;
#34645 = ADVANCED_FACE ( 'NONE', ( #51040 ), #65443, .T. ) ;
#34646 = ORIENTED_EDGE ( 'NONE', *, *, #85580, .T. ) ;
#34647 = FACE_OUTER_BOUND ( 'NONE', #4325, .T. ) ;
#34648 = EDGE_CURVE ( 'NONE', #32199, #124072, #81138, .T. ) ;
#34649 = EDGE_CURVE ( 'NONE', #127662, #129312, #46573, .T. ) ;
#34650 = DIRECTION ( 'NONE',  ( 0.000000000000000000, 0.000000000000000000, 1.000000000000000000 ) ) ;
#34651 = EDGE_CURVE ( 'NONE', #111888, #31897, #48440, .T. ) ;
#34652 = ORIENTED_EDGE ( 'NONE', *, *, #117690, .F. ) ;
#34653 = CARTESIAN_POINT ( 'NONE',  ( -2.499999999999996003, 12.50000000000000000, -4.330127018922201643 ) ) ;
#34654 = DIRECTION ( 'NONE',  ( 0.000000000000000000, 0.000000000000000000, -1.000000000000000000 ) ) ;
#34655 = AXIS2_PLACEMENT_3D ( 'NONE', #77435, #125875, #57150 ) ;
#34656 = CIRCLE ( 'NONE', #13685, 0.06509327318403745899 ) ;
#34657 = ORIENTED_EDGE ( 'NONE', *, *, #41151, .T. ) ;
#34658 = DIRECTION ( 'NONE',  ( -0.000000000000000000, -1.000000000000000000, -0.000000000000000000 ) ) ;
#34660 = EDGE_CURVE ( 'NONE', #28229, #6619, #9007, .T. ) ;
#34659 = CARTESIAN_POINT ( 'NONE',  ( -11.84999999999999609, 12.50000000000000000, 6.776507416713035248 ) ) ;
#34661 = VERTEX_POINT ( 'NONE', #39305 ) ;
#34662 = CARTESIAN_POINT ( 'NONE',  ( -8.550000000000009592, 2.500000000000000000, 6.841600689897072485 ) ) ;
#34663 = DIRECTION ( 'NONE',  ( -0.000000000000000000, -1.000000000000000000, -0.000000000000000000 ) ) ;
#34664 = DIRECTION ( 'NONE',  ( 0.000000000000000000, 0.000000000000000000, 1.000000000000000000 ) ) ;
#34665 = EDGE_LOOP ( 'NONE', ( #126513, #80238 ) ) ;
#34666 = EDGE_LOOP ( 'NONE', ( #32063, #51547, #33114, #94626 ) ) ;
#34667 = LINE ( 'NONE', #123644, #45174 ) ;
#34668 = CIRCLE ( 'NONE', #18390, 0.06509327318403745899 ) ;
#34669 = ORIENTED_EDGE ( 'NONE', *, *, #124964, .F. ) ;
#34670 = DIRECTION ( 'NONE',  ( 0.000000000000000000, 0.000000000000000000, -1.000000000000000000 ) ) ;
#34671 = DIRECTION ( 'NONE',  ( -0.000000000000000000, -1.000000000000000000, -0.000000000000000000 ) ) ;
#34672 = AXIS2_PLACEMENT_3D ( 'NONE', #120616, #2118, #30971 ) ;
#34673 = ORIENTED_EDGE ( 'NONE', *, *, #35638, .T. ) ;
#34674 = CIRCLE ( 'NONE', #124545, 0.06509327318403745899 ) ;
#34675 = DIRECTION ( 'NONE',  ( 0.000000000000000000, 1.000000000000000000, 0.000000000000000000 ) ) ;
#34676 = CARTESIAN_POINT ( 'NONE',  ( 175.5000000000000000, 6.123233995736768501E-17, 2.500000000000000000 ) ) ;
#34677 = CARTESIAN_POINT ( 'NONE',  ( -5.800000000000022027, 12.50000000000000000, -4.265033745738164406 ) ) ;
#34678 = CARTESIAN_POINT ( 'NONE',  ( -4.600000000000025402, 12.50000000000000000, -2.385244779468109755E-15 ) ) ;
#34679 = FACE_OUTER_BOUND ( 'NONE', #87599, .T. ) ;
#34680 = EDGE_LOOP ( 'NONE', ( #57204, #39863 ) ) ;
#34681 = VERTEX_POINT ( 'NONE', #621 ) ;
#34682 = CARTESIAN_POINT ( 'NONE',  ( -6.900000000000019007, 12.50000000000000000, 0.4115034346978109769 ) ) ;
#34683 = CARTESIAN_POINT ( 'NONE',  ( 106.3499248685753997, 6.077234604209151847, -4.730958255624227782 ) ) ;
#34684 = DIRECTION ( 'NONE',  ( 0.000000000000000000, 0.000000000000000000, 1.000000000000000000 ) ) ;
#34687 = VERTEX_POINT ( 'NONE', #40589 ) ;
#34686 = ORIENTED_EDGE ( 'NONE', *, *, #103965, .F. ) ;
#34685 = AXIS2_PLACEMENT_3D ( 'NONE', #48098, #89305, #61139 ) ;
#34688 = ORIENTED_EDGE ( 'NONE', *, *, #42840, .T. ) ;
#34689 = EDGE_CURVE ( 'NONE', #66521, #74881, #21544, .T. ) ;
#34690 = DIRECTION ( 'NONE',  ( -0.000000000000000000, 1.000000000000000000, -0.000000000000000000 ) ) ;
#34691 = ADVANCED_FACE ( 'NONE', ( #30115 ), #23591, .T. ) ;
#34692 = CIRCLE ( 'NONE', #7466, 0.06509327318403745899 ) ;
#34694 = AXIS2_PLACEMENT_3D ( 'NONE', #47856, #10482, #70063 ) ;
#34693 = DIRECTION ( 'NONE',  ( -0.000000000000000000, 1.000000000000000000, -0.000000000000000000 ) ) ;
#34695 = CARTESIAN_POINT ( 'NONE',  ( -1.658312395177699017, -2.500000000000000444, 6.000000000000005329 ) ) ;
#34696 = ADVANCED_FACE ( 'NONE', ( #108001 ), #89661, .T. ) ;
#34697 = CARTESIAN_POINT ( 'NONE',  ( 0.000000000000000000, 0.000000000000000000, 0.000000000000000000 ) ) ;
#34698 = CARTESIAN_POINT ( 'NONE',  ( 11.64999999999990798, 2.500000000000000000, -1.472243186433550122 ) ) ;
#34699 = DIRECTION ( 'NONE',  ( 0.000000000000000000, 0.000000000000000000, -1.000000000000000000 ) ) ;
#34700 = FACE_OUTER_BOUND ( 'NONE', #1452, .T. ) ;
#34701 = CONICAL_SURFACE ( 'NONE', #61883, 0.1000000000000002554, 0.003490658503988666988 ) ;
#34702 = CARTESIAN_POINT ( 'NONE',  ( -8.350000000000008527, 12.50000000000000000, 5.802370205355744659 ) ) ;
#34703 = CARTESIAN_POINT ( 'NONE',  ( -0.6500000000000394351, 12.50000000000000000, 6.906693963081109722 ) ) ;
#34704 = EDGE_CURVE ( 'NONE', #70719, #14663, #65541, .T. ) ;
#34705 = DIRECTION ( 'NONE',  ( 0.000000000000000000, 1.000000000000000000, 0.000000000000000000 ) ) ;
#34706 = ADVANCED_FACE ( 'NONE', ( #41225 ), #70658, .T. ) ;
#34708 = VERTEX_POINT ( 'NONE', #18329 ) ;
#34707 = EDGE_CURVE ( 'NONE', #10760, #47322, #84327, .T. ) ;
#34709 = EDGE_CURVE ( 'NONE', #37316, #96170, #58275, .T. ) ;
#34710 = DIRECTION ( 'NONE',  ( -0.000000000000000000, -1.000000000000000000, -0.000000000000000000 ) ) ;
#34711 = VERTEX_POINT ( 'NONE', #39928 ) ;
#34712 = ORIENTED_EDGE ( 'NONE', *, *, #112530, .T. ) ;
#34713 = CARTESIAN_POINT ( 'NONE',  ( 1.049999999999954525, 2.500000000000000000, -2.511473670974877948 ) ) ;
#34714 = CARTESIAN_POINT ( 'NONE',  ( 10.59999999999990905, 12.50000000000000000, -3.918623584224389056 ) ) ;
#34715 = AXIS2_PLACEMENT_3D ( 'NONE', #43839, #61536, #92930 ) ;
#34716 = FACE_OUTER_BOUND ( 'NONE', #32504, .T. ) ;
#34717 = ADVANCED_FACE ( 'NONE', ( #118463 ), #9108, .T. ) ;
#34718 = DIRECTION ( 'NONE',  ( 0.000000000000000000, 0.000000000000000000, 1.000000000000000000 ) ) ;
#34719 = CARTESIAN_POINT ( 'NONE',  ( 0.3999999999999628852, 2.500000000000000000, -0.6928203230275520319 ) ) ;
#34720 = DIRECTION ( 'NONE',  ( -0.000000000000000000, -1.000000000000000000, -0.000000000000000000 ) ) ;
#34721 = DIRECTION ( 'NONE',  ( 0.000000000000000000, 1.000000000000000000, 0.000000000000000000 ) ) ;
#34722 = ORIENTED_EDGE ( 'NONE', *, *, #23697, .F. ) ;
#34723 = CARTESIAN_POINT ( 'NONE',  ( -7.500000000000001776, -2.500000000000000000, 1.734723475976807094E-15 ) ) ;
#34724 = AXIS2_PLACEMENT_3D ( 'NONE', #88387, #128358, #96277 ) ;
#34725 = AXIS2_PLACEMENT_3D ( 'NONE', #2236, #93858, #42186 ) ;
#34726 = VECTOR ( 'NONE', #129303, 1000.000000000000000 ) ;
#34727 = CARTESIAN_POINT ( 'NONE',  ( 4.549999999999935874, 2.500000000000000000, 6.395190528383296602 ) ) ;
#34728 = EDGE_LOOP ( 'NONE', ( #110697, #115894 ) ) ;
#34729 = VERTEX_POINT ( 'NONE', #108646 ) ;
#34730 = AXIS2_PLACEMENT_3D ( 'NONE', #13013, #91604, #102073 ) ;
#34731 = ORIENTED_EDGE ( 'NONE', *, *, #22390, .F. ) ;
#34732 = EDGE_CURVE ( 'NONE', #52697, #108629, #89021, .T. ) ;
#34733 = ORIENTED_EDGE ( 'NONE', *, *, #110712, .F. ) ;
#34734 = CARTESIAN_POINT ( 'NONE',  ( 0.5999999999999547917, 12.50000000000000000, 3.983716857408420076 ) ) ;
#34735 = DIRECTION ( 'NONE',  ( 0.000000000000000000, 1.000000000000000000, 0.000000000000000000 ) ) ;
#34736 = DIRECTION ( 'NONE',  ( -0.000000000000000000, 1.000000000000000000, -0.000000000000000000 ) ) ;
#34737 = FACE_OUTER_BOUND ( 'NONE', #79348, .T. ) ;
#34739 = AXIS2_PLACEMENT_3D ( 'NONE', #51877, #32251, #73427 ) ;
#34738 = AXIS2_PLACEMENT_3D ( 'NONE', #7117, #126267, #105980 ) ;
#34740 = DIRECTION ( 'NONE',  ( 0.000000000000000000, 0.000000000000000000, 1.000000000000000000 ) ) ;
#34741 = VERTEX_POINT ( 'NONE', #109292 ) ;
#34742 = DIRECTION ( 'NONE',  ( -0.000000000000000000, -1.000000000000000000, -0.000000000000000000 ) ) ;
#34743 = FACE_OUTER_BOUND ( 'NONE', #63152, .T. ) ;
#34744 = CARTESIAN_POINT ( 'NONE',  ( 1.249999999999950262, 12.50000000000000000, 7.188010851410848723 ) ) ;
#34745 = ORIENTED_EDGE ( 'NONE', *, *, #114540, .F. ) ;
#34746 = ADVANCED_FACE ( 'NONE', ( #19635 ), #79830, .T. ) ;
#34747 = VERTEX_POINT ( 'NONE', #113159 ) ;
#34748 = EDGE_LOOP ( 'NONE', ( #77572, #84686 ) ) ;
#34749 = CARTESIAN_POINT ( 'NONE',  ( 10.19999999999991047, 12.50000000000000000, -3.983716857408426293 ) ) ;
#34750 = FACE_OUTER_BOUND ( 'NONE', #109161, .T. ) ;
#34751 = DIRECTION ( 'NONE',  ( 0.000000000000000000, -0.9999939076577903929, 0.003490651415223739937 ) ) ;
#34752 = ORIENTED_EDGE ( 'NONE', *, *, #103491, .F. ) ;
#34753 = DIRECTION ( 'NONE',  ( -0.000000000000000000, 1.000000000000000000, -0.000000000000000000 ) ) ;
#34754 = DIRECTION ( 'NONE',  ( 0.000000000000000000, 0.000000000000000000, 1.000000000000000000 ) ) ;
#34755 = ADVANCED_FACE ( 'NONE', ( #111207 ), #27892, .T. ) ;
#34756 = CARTESIAN_POINT ( 'NONE',  ( -5.850000000000019185, 12.50000000000000000, 6.430097255199259010 ) ) ;
#34757 = DIRECTION ( 'NONE',  ( -4.274815082592931898E-19, -0.9999939076577903929, -0.003490651415223739937 ) ) ;
#34758 = LINE ( 'NONE', #74022, #5928 ) ;
#34759 = ORIENTED_EDGE ( 'NONE', *, *, #23495, .T. ) ;
#34760 = AXIS2_PLACEMENT_3D ( 'NONE', #124491, #104195, #14508 ) ;
#34761 = DIRECTION ( 'NONE',  ( 0.000000000000000000, -0.9999939076577903929, 0.003490651415223739937 ) ) ;
#34762 = VECTOR ( 'NONE', #68187, 1000.000000000000000 ) ;
#34763 = ORIENTED_EDGE ( 'NONE', *, *, #48450, .F. ) ;
#34764 = ORIENTED_EDGE ( 'NONE', *, *, #52542, .T. ) ;
#34765 = DIRECTION ( 'NONE',  ( -0.000000000000000000, -1.000000000000000000, -0.000000000000000000 ) ) ;
#34766 = CARTESIAN_POINT ( 'NONE',  ( 12.69999999999990337, 12.50000000000000000, 3.983716857408420076 ) ) ;
#34767 = CARTESIAN_POINT ( 'NONE',  ( 6.699999999999928235, 12.50000000000000000, -2.276824562219559311E-15 ) ) ;
#34768 = FACE_OUTER_BOUND ( 'NONE', #78763, .T. ) ;
#34769 = AXIS2_PLACEMENT_3D ( 'NONE', #127506, #26090, #97388 ) ;
#34770 = DIRECTION ( 'NONE',  ( 0.000000000000000000, 1.000000000000000000, 0.000000000000000000 ) ) ;
#34771 = ORIENTED_EDGE ( 'NONE', *, *, #85632, .F. ) ;
#34772 = VERTEX_POINT ( 'NONE', #123612 ) ;
#34773 = DIRECTION ( 'NONE',  ( 0.000000000000000000, 1.000000000000000000, 0.000000000000000000 ) ) ;
#34774 = FACE_OUTER_BOUND ( 'NONE', #84918, .T. ) ;
#34775 = CARTESIAN_POINT ( 'NONE',  ( 0.4499999999999569344, 12.50000000000000000, 2.099970236277060032 ) ) ;
#34776 = DIRECTION ( 'NONE',  ( 0.000000000000000000, 0.000000000000000000, 1.000000000000000000 ) ) ;
#34777 = VERTEX_POINT ( 'NONE', #23488 ) ;
#34778 = CIRCLE ( 'NONE', #101671, 0.09999999999999982514 ) ;
#34779 = LINE ( 'NONE', #66145, #7146 ) ;
#34781 = ADVANCED_FACE ( 'NONE', ( #31397 ), #61505, .T. ) ;
#34780 = AXIS2_PLACEMENT_3D ( 'NONE', #123218, #114666, #25006 ) ;
#34782 = CARTESIAN_POINT ( 'NONE',  ( 8.749999999999953815, 12.50000000000000000, -2.165063509461101710 ) ) ;
#34783 = VERTEX_POINT ( 'NONE', #14301 ) ;
#34784 = CARTESIAN_POINT ( 'NONE',  ( 4.349999999999940137, 12.50000000000000000, -6.776507416713040577 ) ) ;
#34785 = ORIENTED_EDGE ( 'NONE', *, *, #98631, .F. ) ;
#34786 = FACE_BOUND ( 'NONE', #114515, .T. ) ;
#34787 = ADVANCED_FACE ( 'NONE', ( #113814 ), #94164, .T. ) ;
#34788 = DIRECTION ( 'NONE',  ( 0.000000000000000000, 0.000000000000000000, -1.000000000000000000 ) ) ;
#34789 = ORIENTED_EDGE ( 'NONE', *, *, #52356, .F. ) ;
#34790 = CARTESIAN_POINT ( 'NONE',  ( 3.099999999999943245, 12.50000000000000000, 3.983716857408420076 ) ) ;
#34791 = FACE_OUTER_BOUND ( 'NONE', #82993, .T. ) ;
#34792 = ADVANCED_FACE ( 'NONE', ( #53608 ), #13001, .T. ) ;
#34793 = ORIENTED_EDGE ( 'NONE', *, *, #50183, .F. ) ;
#34794 = EDGE_CURVE ( 'NONE', #15661, #85617, #77691, .T. ) ;
#34795 = ORIENTED_EDGE ( 'NONE', *, *, #82505, .F. ) ;
#34796 = ADVANCED_FACE ( 'NONE', ( #32699 ), #94795, .T. ) ;
#34797 = ADVANCED_FACE ( 'NONE', ( #103356 ), #113579, .T. ) ;
#34798 = CARTESIAN_POINT ( 'NONE',  ( 185.9218750003414016, 0.000000000000000000, 7.564683531250000925 ) ) ;
#34799 = AXIS2_PLACEMENT_3D ( 'NONE', #28047, #98063, #10335 ) ;
#34800 = CARTESIAN_POINT ( 'NONE',  ( 185.0052083336747444, -6.551208109652278289, 3.782341765624995134 ) ) ;
#34801 = CARTESIAN_POINT ( 'NONE',  ( 3.149999999999942624, 2.500000000000000000, 6.841600689897072485 ) ) ;
#34802 = AXIS2_PLACEMENT_3D ( 'NONE', #9478, #47471, #87376 ) ;
#34803 = FACE_OUTER_BOUND ( 'NONE', #122048, .T. ) ;
#34804 = DIRECTION ( 'NONE',  ( 0.000000000000000000, 0.000000000000000000, 1.000000000000000000 ) ) ;
#34805 = CARTESIAN_POINT ( 'NONE',  ( -10.65000000000000391, 12.50000000000000000, -6.906693963081112386 ) ) ;
#34806 = AXIS2_PLACEMENT_3D ( 'NONE', #36601, #86960, #46380 ) ;
#34807 = PLANE ( 'NONE',  #79870 ) ;
#34808 = EDGE_CURVE ( 'NONE', #30916, #25579, #698, .T. ) ;
#34809 = AXIS2_PLACEMENT_3D ( 'NONE', #96258, #84525, #124455 ) ;
#34810 = AXIS2_PLACEMENT_3D ( 'NONE', #36883, #108818, #39480 ) ;
#34811 = EDGE_CURVE ( 'NONE', #62130, #14341, #80129, .T. ) ;
#34812 = EDGE_CURVE ( 'NONE', #4541, #17715, #91592, .T. ) ;
#34813 = ORIENTED_EDGE ( 'NONE', *, *, #73274, .F. ) ;
#34814 = CONICAL_SURFACE ( 'NONE', #105897, 0.09999999999999982514, 0.003490658503988666988 ) ;
#34815 = ORIENTED_EDGE ( 'NONE', *, *, #90454, .F. ) ;
#34816 = DIRECTION ( 'NONE',  ( 0.000000000000000000, 1.000000000000000000, 0.000000000000000000 ) ) ;
#34817 = DIRECTION ( 'NONE',  ( -0.000000000000000000, 1.000000000000000000, -0.000000000000000000 ) ) ;
#34818 = LINE ( 'NONE', #63619, #124490 ) ;
#34819 = CARTESIAN_POINT ( 'NONE',  ( -5.400000000000019895, 2.500000000000000000, -0.6928203230275541413 ) ) ;
#34821 = VERTEX_POINT ( 'NONE', #112534 ) ;
#34820 = EDGE_LOOP ( 'NONE', ( #73945, #96470, #101607, #105504 ) ) ;
#34822 = PLANE ( 'NONE',  #64137 ) ;
#34823 = EDGE_LOOP ( 'NONE', ( #108751, #37435, #37161, #23733 ) ) ;
#34824 = CARTESIAN_POINT ( 'NONE',  ( -10.65000000000000213, 2.500000000000000000, 2.411473670974873862 ) ) ;
#34825 = DIRECTION ( 'NONE',  ( 0.000000000000000000, 0.000000000000000000, 1.000000000000000000 ) ) ;
#34826 = CIRCLE ( 'NONE', #43234, 0.06509327318403745899 ) ;
#34827 = EDGE_LOOP ( 'NONE', ( #56802, #328 ) ) ;
#34828 = DIRECTION ( 'NONE',  ( 1.000000000000000000, 0.000000000000000000, -8.881784197001232602E-16 ) ) ;
#34829 = LINE ( 'NONE', #66821, #22310 ) ;
#34830 = CARTESIAN_POINT ( 'NONE',  ( -3.950000000000024603, 2.500000000000000000, -2.511473670974877948 ) ) ;
#34832 = AXIS2_PLACEMENT_3D ( 'NONE', #26917, #87116, #84547 ) ;
#34831 = AXIS2_PLACEMENT_3D ( 'NONE', #54153, #23384, #103255 ) ;
#34833 = DIRECTION ( 'NONE',  ( -0.000000000000000000, -1.000000000000000000, -0.000000000000000000 ) ) ;
#34834 = DIRECTION ( 'NONE',  ( -0.000000000000000000, 1.000000000000000000, -0.000000000000000000 ) ) ;
#34835 = CARTESIAN_POINT ( 'NONE',  ( 0.6499999999999543920, 2.500000000000000000, 6.941600689897073018 ) ) ;
#34836 = CARTESIAN_POINT ( 'NONE',  ( 187.3593750003414016, 0.000000000000000000, 7.564683531250000925 ) ) ;
#34837 = DIRECTION ( 'NONE',  ( 0.000000000000000000, -0.000000000000000000, 1.000000000000000000 ) ) ;
#34838 = DIRECTION ( 'NONE',  ( 0.000000000000000000, 0.000000000000000000, 1.000000000000000000 ) ) ;
#34839 = ORIENTED_EDGE ( 'NONE', *, *, #64170, .F. ) ;
#34840 = EDGE_LOOP ( 'NONE', ( #39881, #57995, #7999, #76059 ) ) ;
#34841 = ORIENTED_EDGE ( 'NONE', *, *, #16745, .F. ) ;
#34842 = DIRECTION ( 'NONE',  ( 0.000000000000000000, -0.9999939076577903929, 0.003490651415223739937 ) ) ;
#34843 = ORIENTED_EDGE ( 'NONE', *, *, #129130, .T. ) ;
#34844 = DIRECTION ( 'NONE',  ( 0.000000000000000000, 0.000000000000000000, -1.000000000000000000 ) ) ;
#34846 = EDGE_LOOP ( 'NONE', ( #3163, #34534 ) ) ;
#34845 = ORIENTED_EDGE ( 'NONE', *, *, #41322, .F. ) ;
#34847 = EDGE_LOOP ( 'NONE', ( #63196, #32845 ) ) ;
#34848 = DIRECTION ( 'NONE',  ( 0.000000000000000000, 0.000000000000000000, 1.000000000000000000 ) ) ;
#34849 = LINE ( 'NONE', #36777, #61510 ) ;
#34850 = DIRECTION ( 'NONE',  ( 0.000000000000000000, 1.000000000000000000, 0.000000000000000000 ) ) ;
#34851 = CARTESIAN_POINT ( 'NONE',  ( -3.642919299551294898E-14, 2.500000000000000000, 0.7928203230275517877 ) ) ;
#34852 = CARTESIAN_POINT ( 'NONE',  ( -9.350000000000008527, 2.500000000000000000, -6.841600689897072485 ) ) ;
#34853 = ORIENTED_EDGE ( 'NONE', *, *, #3386, .F. ) ;
#34854 = EDGE_CURVE ( 'NONE', #103956, #123894, #38380, .T. ) ;
#34855 = FACE_OUTER_BOUND ( 'NONE', #127124, .T. ) ;
#34856 = ORIENTED_EDGE ( 'NONE', *, *, #5681, .T. ) ;
#34857 = EDGE_CURVE ( 'NONE', #36092, #62518, #13208, .T. ) ;
#34859 = ORIENTED_EDGE ( 'NONE', *, *, #42957, .F. ) ;
#34858 = AXIS2_PLACEMENT_3D ( 'NONE', #54294, #44470, #5177 ) ;
#34860 = ORIENTED_EDGE ( 'NONE', *, *, #88745, .F. ) ;
#34861 = AXIS2_PLACEMENT_3D ( 'NONE', #48404, #29418, #59550 ) ;
#34862 = EDGE_CURVE ( 'NONE', #15846, #103155, #19477, .T. ) ;
#34863 = LINE ( 'NONE', #125157, #92371 ) ;
#34864 = EDGE_LOOP ( 'NONE', ( #118541, #5302 ) ) ;
#34865 = ORIENTED_EDGE ( 'NONE', *, *, #57078, .F. ) ;
#34866 = VERTEX_POINT ( 'NONE', #111881 ) ;
#34867 = PLANE ( 'NONE',  #111409 ) ;
#34868 = ADVANCED_FACE ( 'NONE', ( #22226 ), #101053, .T. ) ;
#34870 = CONICAL_SURFACE ( 'NONE', #43273, 0.1000000000000002554, 0.003490658503988666988 ) ;
#34869 = CIRCLE ( 'NONE', #87060, 0.06509327318403745899 ) ;
#34871 = CARTESIAN_POINT ( 'NONE',  ( 4.149999999999941735, 2.500000000000000000, -2.857883832488653741 ) ) ;
#34872 = FACE_OUTER_BOUND ( 'NONE', #82016, .T. ) ;
#34873 = CARTESIAN_POINT ( 'NONE',  ( 3.349999999999945466, 2.500000000000000000, -2.065063509461102065 ) ) ;
#34874 = CARTESIAN_POINT ( 'NONE',  ( -12.69999999999999041, 2.500000000000000000, 3.983716857408420964 ) ) ;
#34875 = CARTESIAN_POINT ( 'NONE',  ( 3.349999999999941913, 2.500000000000000000, 6.595190528383296780 ) ) ;
#34876 = ORIENTED_EDGE ( 'NONE', *, *, #110318, .T. ) ;
#34877 = DIRECTION ( 'NONE',  ( 0.000000000000000000, 0.000000000000000000, 1.000000000000000000 ) ) ;
#34879 = AXIS2_PLACEMENT_3D ( 'NONE', #54394, #26238, #114597 ) ;
#34878 = AXIS2_PLACEMENT_3D ( 'NONE', #30227, #70142, #73337 ) ;
#34880 = ORIENTED_EDGE ( 'NONE', *, *, #11933, .T. ) ;
#34881 = CARTESIAN_POINT ( 'NONE',  ( -7.100000000000017408, 2.500000000000000000, 0.5928203230275495006 ) ) ;
#34882 = CIRCLE ( 'NONE', #22260, 0.1000000000000002554 ) ;
#34883 = ORIENTED_EDGE ( 'NONE', *, *, #37237, .F. ) ;
#34884 = CARTESIAN_POINT ( 'NONE',  ( 1.899999999999951283, 12.50000000000000000, -3.918623584224389056 ) ) ;
#34885 = ORIENTED_EDGE ( 'NONE', *, *, #124796, .T. ) ;
#34886 = ADVANCED_FACE ( 'NONE', ( #16226 ), #61353, .T. ) ;
#34887 = ORIENTED_EDGE ( 'NONE', *, *, #23727, .F. ) ;
#34888 = DIRECTION ( 'NONE',  ( 0.000000000000000000, 0.000000000000000000, 1.000000000000000000 ) ) ;
#34889 = CARTESIAN_POINT ( 'NONE',  ( -10.84999999999999964, 2.500000000000000000, 2.857883832488649301 ) ) ;
#34890 = CARTESIAN_POINT ( 'NONE',  ( -11.89999999999999680, 2.500000000000000000, -0.3464101615137741841 ) ) ;
#34891 = DIRECTION ( 'NONE',  ( 0.000000000000000000, 0.000000000000000000, -1.000000000000000000 ) ) ;
#34892 = ORIENTED_EDGE ( 'NONE', *, *, #48549, .F. ) ;
#34893 = LINE ( 'NONE', #65613, #81210 ) ;
#34894 = DIRECTION ( 'NONE',  ( -0.000000000000000000, 1.000000000000000000, -0.000000000000000000 ) ) ;
#34895 = LINE ( 'NONE', #73495, #125422 ) ;
#34896 = AXIS2_PLACEMENT_3D ( 'NONE', #119479, #79575, #9546 ) ;
#34897 = CARTESIAN_POINT ( 'NONE',  ( 9.549999999999918998, 12.50000000000000000, 2.165063509461097713 ) ) ;
#34898 = CIRCLE ( 'NONE', #28621, 0.09999999999999982514 ) ;
#34899 = CARTESIAN_POINT ( 'NONE',  ( 3.099999999999945022, 12.50000000000000000, -4.611443907251940644 ) ) ;
#34900 = EDGE_LOOP ( 'NONE', ( #71199, #11477 ) ) ;
#34901 = AXIS2_PLACEMENT_3D ( 'NONE', #13328, #33635, #102377 ) ;
#34902 = EDGE_CURVE ( 'NONE', #107815, #125293, #85631, .T. ) ;
#34903 = ORIENTED_EDGE ( 'NONE', *, *, #33018, .T. ) ;
#34904 = AXIS2_PLACEMENT_3D ( 'NONE', #3086, #33818, #84852 ) ;
#34905 = ORIENTED_EDGE ( 'NONE', *, *, #14223, .T. ) ;
#34906 = CONICAL_SURFACE ( 'NONE', #120562, 0.1000000000000000056, 0.003490658503988666988 ) ;
#34907 = DIRECTION ( 'NONE',  ( 0.000000000000000000, 0.000000000000000000, 1.000000000000000000 ) ) ;
#34908 = CARTESIAN_POINT ( 'NONE',  ( 17.50000000000000000, 2.500000000000000000, -3.999999999999996447 ) ) ;
#34909 = CIRCLE ( 'NONE', #11890, 0.1000000000000000472 ) ;
#34910 = CARTESIAN_POINT ( 'NONE',  ( 184.2135416670080588, 4.367472073101518859, -7.564683531249999149 ) ) ;
#34912 = AXIS2_PLACEMENT_3D ( 'NONE', #26136, #16285, #54298 ) ;
#34911 = CARTESIAN_POINT ( 'NONE',  ( 9.149999999999920419, 2.500000000000000000, 1.472243186433545459 ) ) ;
#34913 = FACE_OUTER_BOUND ( 'NONE', #6509, .T. ) ;
#34914 = EDGE_CURVE ( 'NONE', #50143, #8279, #105279, .T. ) ;
#34915 = DIRECTION ( 'NONE',  ( 0.000000000000000000, -0.9999939076577903929, 0.003490651415223739937 ) ) ;
#34916 = FACE_OUTER_BOUND ( 'NONE', #103844, .T. ) ;
#34917 = VERTEX_POINT ( 'NONE', #56792 ) ;
#34918 = VECTOR ( 'NONE', #31550, 1000.000000000000000 ) ;
#34920 = AXIS2_PLACEMENT_3D ( 'NONE', #94211, #84390, #64744 ) ;
#34919 = VECTOR ( 'NONE', #67830, 1000.000000000000227 ) ;
#34921 = CARTESIAN_POINT ( 'NONE',  ( 2.299999999999948752, 2.500000000000000000, -4.083716857408426826 ) ) ;
#34922 = DIRECTION ( 'NONE',  ( -0.000000000000000000, -1.000000000000000000, -0.000000000000000000 ) ) ;
#34923 = ORIENTED_EDGE ( 'NONE', *, *, #72324, .F. ) ;
#34924 = EDGE_CURVE ( 'NONE', #55864, #50530, #126082, .T. ) ;
#34925 = CARTESIAN_POINT ( 'NONE',  ( -9.600000000000006750, 12.50000000000000000, 5.088040615133786027 ) ) ;
#34926 = VERTEX_POINT ( 'NONE', #65991 ) ;
#34927 = DIRECTION ( 'NONE',  ( -4.274815082592931898E-19, -0.9999939076577903929, -0.003490651415223739937 ) ) ;
#34928 = EDGE_LOOP ( 'NONE', ( #53208, #104309, #93293, #47336 ) ) ;
#34929 = DIRECTION ( 'NONE',  ( 0.000000000000000000, -0.9999939076577903929, 0.003490651415223739937 ) ) ;
#34930 = FACE_OUTER_BOUND ( 'NONE', #40314, .T. ) ;
#34931 = VECTOR ( 'NONE', #17405, 1000.000000000000000 ) ;
#34932 = CARTESIAN_POINT ( 'NONE',  ( -9.400000000000007461, 2.500000000000000000, -0.3464101615137783474 ) ) ;
#34933 = ORIENTED_EDGE ( 'NONE', *, *, #9943, .F. ) ;
#34934 = DIRECTION ( 'NONE',  ( 0.000000000000000000, 0.000000000000000000, -1.000000000000000000 ) ) ;
#34935 = ADVANCED_FACE ( 'NONE', ( #46346 ), #59314, .T. ) ;
#34936 = DIRECTION ( 'NONE',  ( 0.000000000000000000, 0.000000000000000000, -1.000000000000000000 ) ) ;
#34937 = ORIENTED_EDGE ( 'NONE', *, *, #86961, .F. ) ;
#34938 = CARTESIAN_POINT ( 'NONE',  ( 10.64999999999990976, 2.500000000000000000, -6.741600689897077281 ) ) ;
#34939 = EDGE_CURVE ( 'NONE', #121018, #3070, #55084, .T. ) ;
#34940 = VECTOR ( 'NONE', #42399, 1000.000000000000000 ) ;
#34941 = ORIENTED_EDGE ( 'NONE', *, *, #6803, .F. ) ;
#34942 = ORIENTED_EDGE ( 'NONE', *, *, #101543, .T. ) ;
#34943 = DIRECTION ( 'NONE',  ( 0.000000000000000000, 0.000000000000000000, 1.000000000000000000 ) ) ;
#34944 = DIRECTION ( 'NONE',  ( 0.000000000000000000, 1.000000000000000000, 0.000000000000000000 ) ) ;
#34945 = ADVANCED_FACE ( 'NONE', ( #64700 ), #128260, .T. ) ;
#34946 = EDGE_CURVE ( 'NONE', #71349, #80664, #6934, .T. ) ;
#34947 = EDGE_LOOP ( 'NONE', ( #101959, #13696 ) ) ;
#34948 = EDGE_CURVE ( 'NONE', #43610, #27804, #126206, .T. ) ;
#34949 = EDGE_CURVE ( 'NONE', #61414, #70903, #6394, .T. ) ;
#34950 = FACE_OUTER_BOUND ( 'NONE', #125029, .T. ) ;
#34951 = CARTESIAN_POINT ( 'NONE',  ( -13.09999999999999254, 12.50000000000000000, -0.4115034346978115321 ) ) ;
#34952 = ORIENTED_EDGE ( 'NONE', *, *, #87778, .T. ) ;
#34953 = AXIS2_PLACEMENT_3D ( 'NONE', #75295, #25534, #105411 ) ;
#34954 = DIRECTION ( 'NONE',  ( -0.000000000000000000, -1.000000000000000000, -0.000000000000000000 ) ) ;
#34955 = CARTESIAN_POINT ( 'NONE',  ( -9.150000000000005684, 12.50000000000000000, 5.802370205355744659 ) ) ;
#34956 = EDGE_CURVE ( 'NONE', #27189, #74312, #103108, .T. ) ;
#34957 = DIRECTION ( 'NONE',  ( 0.000000000000000000, 0.000000000000000000, 1.000000000000000000 ) ) ;
#34958 = FACE_OUTER_BOUND ( 'NONE', #10380, .T. ) ;
#34959 = CARTESIAN_POINT ( 'NONE',  ( 5.799999999999934985, 2.500000000000000000, -4.330127018922201643 ) ) ;
#34960 = EDGE_CURVE ( 'NONE', #92950, #60183, #34626, .T. ) ;
#34961 = LINE ( 'NONE', #75494, #36775 ) ;
#34962 = DIRECTION ( 'NONE',  ( -0.000000000000000000, 1.000000000000000000, -0.000000000000000000 ) ) ;
#34963 = ADVANCED_FACE ( 'NONE', ( #74531 ), #96835, .T. ) ;
#34965 = AXIS2_PLACEMENT_3D ( 'NONE', #128821, #79059, #86264 ) ;
#34964 = VECTOR ( 'NONE', #105052, 1000.000000000000000 ) ;
#34966 = EDGE_CURVE ( 'NONE', #12963, #122201, #23691, .T. ) ;
#34967 = CIRCLE ( 'NONE', #1489, 0.06509327318403745899 ) ;
#34968 = EDGE_CURVE ( 'NONE', #123444, #69018, #57231, .T. ) ;
#34969 = VERTEX_POINT ( 'NONE', #115731 ) ;
#34970 = VERTEX_POINT ( 'NONE', #5133 ) ;
#34971 = ORIENTED_EDGE ( 'NONE', *, *, #71695, .T. ) ;
#34972 = EDGE_LOOP ( 'NONE', ( #34201, #30512 ) ) ;
#34973 = DIRECTION ( 'NONE',  ( 0.000000000000000000, -0.000000000000000000, 1.000000000000000000 ) ) ;
#34974 = DIRECTION ( 'NONE',  ( 0.000000000000000000, 0.000000000000000000, -1.000000000000000000 ) ) ;
#34975 = DIRECTION ( 'NONE',  ( 0.000000000000000000, -0.9999939076577903929, 0.003490651415223739937 ) ) ;
#34976 = VERTEX_POINT ( 'NONE', #65334 ) ;
#34977 = ADVANCED_FACE ( 'NONE', ( #45083 ), #69751, .T. ) ;
#34978 = FACE_BOUND ( 'NONE', #34067, .T. ) ;
#34979 = ADVANCED_FACE ( 'NONE', ( #26083 ), #115072, .F. ) ;
#34980 = CARTESIAN_POINT ( 'NONE',  ( -12.29999999999999538, 12.50000000000000000, -0.4115034346978116431 ) ) ;
#34981 = CARTESIAN_POINT ( 'NONE',  ( 10.79999999999991012, 12.50000000000000000, -4.330127018922201643 ) ) ;
#34982 = CARTESIAN_POINT ( 'NONE',  ( 11.64999999999990443, 2.500000000000000000, -7.288010851410854585 ) ) ;
#34983 = CARTESIAN_POINT ( 'NONE',  ( -15.39999999999998082, 2.500000000000000000, 0.7928203230275517877 ) ) ;
#34984 = CARTESIAN_POINT ( 'NONE',  ( 7.099999999999928590, 12.50000000000000000, -4.957854068765716882 ) ) ;
#34985 = CARTESIAN_POINT ( 'NONE',  ( 4.999999999999973355, 2.500000000000000000, -4.230127018922201998 ) ) ;
#34986 = DIRECTION ( 'NONE',  ( -0.000000000000000000, -1.000000000000000000, -0.000000000000000000 ) ) ;
#34987 = DIRECTION ( 'NONE',  ( 0.000000000000000000, 1.000000000000000000, 0.000000000000000000 ) ) ;
#34988 = CARTESIAN_POINT ( 'NONE',  ( 5.849999999999932143, 12.50000000000000000, 2.099970236277060032 ) ) ;
#34989 = CONICAL_SURFACE ( 'NONE', #39196, 0.1000000000000000056, 0.003490658503988666988 ) ;
#34990 = AXIS2_PLACEMENT_3D ( 'NONE', #64899, #23705, #43999 ) ;
#34991 = FACE_OUTER_BOUND ( 'NONE', #59978, .T. ) ;
#34992 = ORIENTED_EDGE ( 'NONE', *, *, #29238, .F. ) ;
#34994 = ORIENTED_EDGE ( 'NONE', *, *, #29022, .F. ) ;
#34993 = AXIS2_PLACEMENT_3D ( 'NONE', #71613, #101079, #2216 ) ;
#34995 = ORIENTED_EDGE ( 'NONE', *, *, #92327, .T. ) ;
#34996 = ORIENTED_EDGE ( 'NONE', *, *, #5883, .T. ) ;
#34997 = CARTESIAN_POINT ( 'NONE',  ( -3.100000000000028511, 12.50000000000000000, -0.3464101615137782364 ) ) ;
#34998 = ORIENTED_EDGE ( 'NONE', *, *, #94317, .F. ) ;
#34999 = CARTESIAN_POINT ( 'NONE',  ( -9.400000000000009237, 12.50000000000000000, -3.983716857408421852 ) ) ;
#35000 = ORIENTED_EDGE ( 'NONE', *, *, #1550, .T. ) ;
#35002 = ORIENTED_EDGE ( 'NONE', *, *, #52578, .F. ) ;
#35001 = AXIS2_PLACEMENT_3D ( 'NONE', #4834, #33051, #44794 ) ;
#35003 = AXIS2_PLACEMENT_3D ( 'NONE', #41737, #33203, #31901 ) ;
#35004 = AXIS2_PLACEMENT_3D ( 'NONE', #70282, #89268, #109558 ) ;
#35005 = VECTOR ( 'NONE', #8478, 1000.000000000000000 ) ;
#35006 = FACE_OUTER_BOUND ( 'NONE', #23977, .T. ) ;
#35007 = DIRECTION ( 'NONE',  ( -0.000000000000000000, 1.000000000000000000, -0.000000000000000000 ) ) ;
#35008 = CARTESIAN_POINT ( 'NONE',  ( -14.34999999999998543, 2.500000000000000000, -1.718653347947323606 ) ) ;
#35009 = DIRECTION ( 'NONE',  ( 0.000000000000000000, 1.000000000000000000, 0.000000000000000000 ) ) ;
#35010 = AXIS2_PLACEMENT_3D ( 'NONE', #71864, #101324, #63318 ) ;
#35011 = ORIENTED_EDGE ( 'NONE', *, *, #64631, .F. ) ;
#35012 = ORIENTED_EDGE ( 'NONE', *, *, #47225, .T. ) ;
#35013 = ADVANCED_FACE ( 'NONE', ( #28662 ), #70500, .T. ) ;
#35015 = VECTOR ( 'NONE', #38016, 1000.000000000000000 ) ;
#35014 = AXIS2_PLACEMENT_3D ( 'NONE', #4230, #56556, #116771 ) ;
#35016 = EDGE_LOOP ( 'NONE', ( #38875, #82640 ) ) ;
#35018 = ORIENTED_EDGE ( 'NONE', *, *, #103481, .F. ) ;
#35017 = DIRECTION ( 'NONE',  ( 0.000000000000000000, 1.000000000000000000, 0.000000000000000000 ) ) ;
#35019 = ADVANCED_FACE ( 'NONE', ( #100598 ), #8352, .T. ) ;
#35020 = DIRECTION ( 'NONE',  ( -4.274815082592931898E-19, -0.9999939076577903929, -0.003490651415223739937 ) ) ;
#35021 = EDGE_LOOP ( 'NONE', ( #13384, #39042, #121222, #28762 ) ) ;
#35022 = ORIENTED_EDGE ( 'NONE', *, *, #28365, .F. ) ;
#35023 = DIRECTION ( 'NONE',  ( 0.000000000000000000, 0.000000000000000000, -1.000000000000000000 ) ) ;
#35024 = EDGE_CURVE ( 'NONE', #78315, #121706, #103201, .T. ) ;
#35025 = DIRECTION ( 'NONE',  ( -0.000000000000000000, -1.000000000000000000, -0.000000000000000000 ) ) ;
#35026 = DIRECTION ( 'NONE',  ( -0.000000000000000000, -1.000000000000000000, -0.000000000000000000 ) ) ;
#35027 = CARTESIAN_POINT ( 'NONE',  ( 12.09999999999990195, 12.50000000000000000, -0.6277270498435166823 ) ) ;
#35028 = DIRECTION ( 'NONE',  ( 0.000000000000000000, 1.000000000000000000, 0.000000000000000000 ) ) ;
#35029 = AXIS2_PLACEMENT_3D ( 'NONE', #39038, #29834, #128710 ) ;
#35030 = VERTEX_POINT ( 'NONE', #109794 ) ;
#35031 = CARTESIAN_POINT ( 'NONE',  ( 0.3999999999999563904, 2.500000000000000000, 4.922947341949748257 ) ) ;
#35032 = EDGE_LOOP ( 'NONE', ( #56492, #49700, #115985, #104480 ) ) ;
#35033 = CARTESIAN_POINT ( 'NONE',  ( -5.850000000000018296, 12.50000000000000000, 5.802370205355744659 ) ) ;
#35034 = EDGE_LOOP ( 'NONE', ( #16991, #45070 ) ) ;
#35035 = CARTESIAN_POINT ( 'NONE',  ( -1.250000000000001110, 12.50000000000000000, -6.430097255199264339 ) ) ;
#35036 = DIRECTION ( 'NONE',  ( -0.000000000000000000, -1.000000000000000000, -0.000000000000000000 ) ) ;
#35037 = DIRECTION ( 'NONE',  ( 0.000000000000000000, 1.000000000000000000, 0.000000000000000000 ) ) ;
#35038 = DIRECTION ( 'NONE',  ( 0.000000000000000000, 1.000000000000000000, 0.000000000000000000 ) ) ;
#35039 = ORIENTED_EDGE ( 'NONE', *, *, #63070, .F. ) ;
#35040 =( NAMED_UNIT ( * ) PLANE_ANGLE_UNIT ( ) SI_UNIT ( $, .RADIAN. ) );
#35041 = AXIS2_PLACEMENT_3D ( 'NONE', #42086, #53202, #100992 ) ;
#35042 = AXIS2_PLACEMENT_3D ( 'NONE', #10097, #110231, #48095 ) ;
#35043 = DIRECTION ( 'NONE',  ( -0.000000000000000000, -1.000000000000000000, -0.000000000000000000 ) ) ;
#35044 = EDGE_LOOP ( 'NONE', ( #98133, #107711 ) ) ;
#35045 = ORIENTED_EDGE ( 'NONE', *, *, #117738, .T. ) ;
#35046 = ORIENTED_EDGE ( 'NONE', *, *, #39686, .F. ) ;
#35047 = DIRECTION ( 'NONE',  ( 0.000000000000000000, 0.000000000000000000, 1.000000000000000000 ) ) ;
#35048 = DIRECTION ( 'NONE',  ( 0.000000000000000000, 0.000000000000000000, 1.000000000000000000 ) ) ;
#35049 = CARTESIAN_POINT ( 'NONE',  ( 184.3177083336747160, 4.367472073101515306, 7.564683531250000925 ) ) ;
#35050 = DIRECTION ( 'NONE',  ( -4.274815082592931898E-19, -0.9999939076577903929, -0.003490651415223739937 ) ) ;
#35052 = AXIS2_PLACEMENT_3D ( 'NONE', #86874, #105230, #56747 ) ;
#35051 = CONICAL_SURFACE ( 'NONE', #5755, 0.1000000000000002554, 0.003490658503988666988 ) ;
#35053 = EDGE_CURVE ( 'NONE', #16096, #29908, #69201, .T. ) ;
#35054 = AXIS2_PLACEMENT_3D ( 'NONE', #60451, #42084, #80723 ) ;
#35055 = CARTESIAN_POINT ( 'NONE',  ( -7.100000000000017408, 12.50000000000000000, -0.6928203230275542523 ) ) ;
#35056 = DIRECTION ( 'NONE',  ( 0.000000000000000000, 0.000000000000000000, -1.000000000000000000 ) ) ;
#35057 = EDGE_LOOP ( 'NONE', ( #111986, #44497 ) ) ;
#35058 = CARTESIAN_POINT ( 'NONE',  ( 105.5000000000000142, 0.000000000000000000, 0.000000000000000000 ) ) ;
#35059 = ORIENTED_EDGE ( 'NONE', *, *, #33883, .F. ) ;
#35060 = EDGE_CURVE ( 'NONE', #47494, #31560, #13301, .T. ) ;
#35061 = FACE_OUTER_BOUND ( 'NONE', #125821, .T. ) ;
#35062 = PLANE ( 'NONE',  #86070 ) ;
#35063 = EDGE_CURVE ( 'NONE', #35289, #104203, #101152, .T. ) ;
#35064 = CARTESIAN_POINT ( 'NONE',  ( 2.699999999999946443, 12.50000000000000000, 0.3464101615137735735 ) ) ;
#35065 = ORIENTED_EDGE ( 'NONE', *, *, #57081, .T. ) ;
#35066 = VECTOR ( 'NONE', #60579, 1000.000000000000000 ) ;
#35067 = CARTESIAN_POINT ( 'NONE',  ( -3.749999999999991562, 2.500000000000000000, 6.495190528383297135 ) ) ;
#35068 = DIRECTION ( 'NONE',  ( -0.000000000000000000, -1.000000000000000000, -0.000000000000000000 ) ) ;
#35069 = VECTOR ( 'NONE', #36755, 1000.000000000000000 ) ;
#35070 = EDGE_CURVE ( 'NONE', #16557, #33663, #88183, .T. ) ;
#35071 = AXIS2_PLACEMENT_3D ( 'NONE', #62034, #44816, #124662 ) ;
#35072 = ORIENTED_EDGE ( 'NONE', *, *, #107639, .F. ) ;
#35073 = CONICAL_SURFACE ( 'NONE', #106068, 0.1000000000000002554, 0.003490658503988666988 ) ;
#35074 = CARTESIAN_POINT ( 'NONE',  ( -4.400000000000025224, 2.500000000000000000, 0.4464101615137735513 ) ) ;
#35075 = VECTOR ( 'NONE', #108295, 1000.000000000000000 ) ;
#35076 = ORIENTED_EDGE ( 'NONE', *, *, #127563, .T. ) ;
#35077 = ORIENTED_EDGE ( 'NONE', *, *, #113831, .F. ) ;
#35078 = CARTESIAN_POINT ( 'NONE',  ( -0.2000000000000347888, 12.50000000000000000, 0.3464101615137758494 ) ) ;
#35079 = VECTOR ( 'NONE', #40789, 1000.000000000000000 ) ;
#35080 = VERTEX_POINT ( 'NONE', #48948 ) ;
#35081 = CARTESIAN_POINT ( 'NONE',  ( 5.199999999999935341, 12.50000000000000000, -0.4115034346978157509 ) ) ;
#35082 = DIRECTION ( 'NONE',  ( 0.000000000000000000, 0.000000000000000000, -1.000000000000000000 ) ) ;
#35083 = DIRECTION ( 'NONE',  ( -0.000000000000000000, -1.000000000000000000, -0.000000000000000000 ) ) ;
#35084 = EDGE_LOOP ( 'NONE', ( #10122, #43701 ) ) ;
#35085 = CONICAL_SURFACE ( 'NONE', #76928, 0.1000000000000002554, 0.003490658503988666988 ) ;
#35086 = FACE_BOUND ( 'NONE', #67955, .T. ) ;
#35087 = CARTESIAN_POINT ( 'NONE',  ( 6.899999999999928413, 12.50000000000000000, 4.676537180435972552 ) ) ;
#35089 = ORIENTED_EDGE ( 'NONE', *, *, #15100, .F. ) ;
#35088 = CARTESIAN_POINT ( 'NONE',  ( 13.09999999999990195, 2.500000000000000000, 4.676537180435972552 ) ) ;
#35090 = DIRECTION ( 'NONE',  ( -0.000000000000000000, -1.000000000000000000, -0.000000000000000000 ) ) ;
#35091 = CIRCLE ( 'NONE', #106187, 0.1000000000000000472 ) ;
#35092 = DIRECTION ( 'NONE',  ( 1.000000000000000000, 0.000000000000000000, 0.000000000000000000 ) ) ;
#35093 = EDGE_LOOP ( 'NONE', ( #15173, #9471, #46990, #45488 ) ) ;
#35094 = EDGE_CURVE ( 'NONE', #93190, #73490, #36329, .T. ) ;
#35096 = CONICAL_SURFACE ( 'NONE', #26764, 0.09999999999999999167, 0.003490658503988666988 ) ;
#35095 = VECTOR ( 'NONE', #114057, 1000.000000000000000 ) ;
#35097 = ORIENTED_EDGE ( 'NONE', *, *, #77597, .F. ) ;
#35098 = VERTEX_POINT ( 'NONE', #47655 ) ;
#35099 = DIRECTION ( 'NONE',  ( 0.000000000000000000, 0.000000000000000000, 1.000000000000000000 ) ) ;
#35100 = CARTESIAN_POINT ( 'NONE',  ( -10.84999999999999964, 12.50000000000000000, 2.857883832488649301 ) ) ;
#35101 = LINE ( 'NONE', #85465, #35776 ) ;
#35102 = EDGE_CURVE ( 'NONE', #79548, #82957, #46781, .T. ) ;
#35103 = FACE_BOUND ( 'NONE', #77428, .T. ) ;
#35104 = ORIENTED_EDGE ( 'NONE', *, *, #79304, .F. ) ;
#35105 = CARTESIAN_POINT ( 'NONE',  ( 185.9427083336747160, -6.551208109652278289, 3.782341765624995134 ) ) ;
#35106 = ADVANCED_FACE ( 'NONE', ( #110426 ), #87557, .T. ) ;
#35107 = FACE_OUTER_BOUND ( 'NONE', #112379, .T. ) ;
#35108 = CARTESIAN_POINT ( 'NONE',  ( 13.14999999999990088, 2.500000000000000000, 2.411473670974873862 ) ) ;
#35109 = CARTESIAN_POINT ( 'NONE',  ( 12.09999999999990550, 2.500000000000000000, 4.230127018922196669 ) ) ;
#35110 = ADVANCED_FACE ( 'NONE', ( #120264 ), #117847, .T. ) ;
#35111 = DIRECTION ( 'NONE',  ( -1.000000000000000000, 0.000000000000000000, 0.000000000000000000 ) ) ;
#35112 = EDGE_CURVE ( 'NONE', #20003, #55549, #119594, .T. ) ;
#35113 = FACE_OUTER_BOUND ( 'NONE', #56829, .T. ) ;
#35114 = EDGE_CURVE ( 'NONE', #93230, #8603, #86463, .T. ) ;
#35115 = CARTESIAN_POINT ( 'NONE',  ( 9.599999999999914380, 12.50000000000000000, 4.330127018922196314 ) ) ;
#35116 = DIRECTION ( 'NONE',  ( 0.000000000000000000, 0.000000000000000000, -1.000000000000000000 ) ) ;
#35117 = CARTESIAN_POINT ( 'NONE',  ( 1.249999999999988898, 12.50000000000000000, -6.495190528383302464 ) ) ;
#35118 = EDGE_CURVE ( 'NONE', #13136, #20444, #50989, .T. ) ;
#35119 = ORIENTED_EDGE ( 'NONE', *, *, #105709, .F. ) ;
#35120 = EDGE_LOOP ( 'NONE', ( #22052, #94714 ) ) ;
#35121 = EDGE_LOOP ( 'NONE', ( #25972, #46352 ) ) ;
#35122 = VERTEX_POINT ( 'NONE', #50236 ) ;
#35123 = VERTEX_POINT ( 'NONE', #37825 ) ;
#35124 = CARTESIAN_POINT ( 'NONE',  ( -7.100000000000017408, 2.500000000000000000, -3.637306695894650055 ) ) ;
#35125 = AXIS2_PLACEMENT_3D ( 'NONE', #1149, #111755, #51558 ) ;
#35126 = CARTESIAN_POINT ( 'NONE',  ( 12.04999999999990834, 2.500000000000000000, 6.395190528383296602 ) ) ;
#35127 = ORIENTED_EDGE ( 'NONE', *, *, #108689, .F. ) ;
#35128 = FACE_BOUND ( 'NONE', #80837, .T. ) ;
#35129 = ADVANCED_FACE ( 'NONE', ( #90124 ), #67687, .T. ) ;
#35130 = CARTESIAN_POINT ( 'NONE',  ( 11.04999999999990834, 2.500000000000000000, -6.741600689897077281 ) ) ;
#35131 = CIRCLE ( 'NONE', #51839, 0.09999999999999982514 ) ;
#35132 = CIRCLE ( 'NONE', #118732, 0.06509327318403745899 ) ;
#35133 = DIRECTION ( 'NONE',  ( 0.000000000000000000, 0.000000000000000000, 1.000000000000000000 ) ) ;
#35134 = ORIENTED_EDGE ( 'NONE', *, *, #82421, .F. ) ;
#35135 = DIRECTION ( 'NONE',  ( 0.000000000000000000, 0.000000000000000000, 1.000000000000000000 ) ) ;
#35136 = CARTESIAN_POINT ( 'NONE',  ( 186.8333333333333144, 6.668395609140177704, -3.849999999999998312 ) ) ;
#35137 = CARTESIAN_POINT ( 'NONE',  ( -1.050000000000037348, 2.500000000000000000, -6.941600689897078347 ) ) ;
#35138 = ORIENTED_EDGE ( 'NONE', *, *, #27418, .F. ) ;
#35139 = CARTESIAN_POINT ( 'NONE',  ( 8.349999999999923261, 2.500000000000000000, -6.395190528383301931 ) ) ;
#35140 = CONICAL_SURFACE ( 'NONE', #41395, 0.1000000000000002554, 0.003490658503988666988 ) ;
#35141 = VERTEX_POINT ( 'NONE', #98662 ) ;
#35142 = AXIS2_PLACEMENT_3D ( 'NONE', #129039, #69435, #79283 ) ;
#35143 = AXIS2_PLACEMENT_3D ( 'NONE', #107342, #80491, #122344 ) ;
#35144 = ORIENTED_EDGE ( 'NONE', *, *, #44107, .T. ) ;
#35145 = VERTEX_POINT ( 'NONE', #77729 ) ;
#35146 = DIRECTION ( 'NONE',  ( -4.274815082592931898E-19, -0.9999939076577903929, -0.003490651415223739937 ) ) ;
#35147 = CARTESIAN_POINT ( 'NONE',  ( 0.000000000000000000, 0.000000000000000000, -5.000000000000004441 ) ) ;
#35148 = DIRECTION ( 'NONE',  ( 0.000000000000000000, 0.000000000000000000, 1.000000000000000000 ) ) ;
#35149 = VERTEX_POINT ( 'NONE', #117643 ) ;
#35150 = CARTESIAN_POINT ( 'NONE',  ( 12.06068301313072411, 2.499999999999358735, -8.632776999393163564 ) ) ;
#35151 = AXIS2_PLACEMENT_3D ( 'NONE', #125104, #55714, #43339 ) ;
#35152 = LINE ( 'NONE', #95985, #44941 ) ;
#35153 = CARTESIAN_POINT ( 'NONE',  ( 7.899999999999921307, 12.50000000000000000, 0.06509327318403504425 ) ) ;
#35154 = CARTESIAN_POINT ( 'NONE',  ( 184.0312500006828031, 9.429780353434619030E-16, -7.700000000000000178 ) ) ;
#35155 = CARTESIAN_POINT ( 'NONE',  ( -1.650000000000035660, 12.50000000000000000, 7.188010851410848723 ) ) ;
#35156 = PLANE ( 'NONE',  #95556 ) ;
#35157 = VERTEX_POINT ( 'NONE', #98028 ) ;
#35158 = PLANE ( 'NONE',  #42079 ) ;
#35159 = ORIENTED_EDGE ( 'NONE', *, *, #8944, .T. ) ;
#35160 = EDGE_CURVE ( 'NONE', #10677, #62255, #124124, .T. ) ;
#35161 = ORIENTED_EDGE ( 'NONE', *, *, #78347, .F. ) ;
#35162 = FACE_OUTER_BOUND ( 'NONE', #93063, .T. ) ;
#35163 = CARTESIAN_POINT ( 'NONE',  ( -11.84999999999999609, 2.500000000000000000, 6.841600689897072485 ) ) ;
#35164 = FACE_OUTER_BOUND ( 'NONE', #51124, .T. ) ;
#35165 = CARTESIAN_POINT ( 'NONE',  ( -4.350000000000023626, 12.50000000000000000, -2.511473670974877948 ) ) ;
#35166 = DIRECTION ( 'NONE',  ( 0.000000000000000000, 1.000000000000000000, 0.000000000000000000 ) ) ;
#35167 = ORIENTED_EDGE ( 'NONE', *, *, #37918, .T. ) ;
#35168 = AXIS2_PLACEMENT_3D ( 'NONE', #62844, #61573, #31460 ) ;
#35169 = ORIENTED_EDGE ( 'NONE', *, *, #30283, .T. ) ;
#35170 = ADVANCED_FACE ( 'NONE', ( #122831 ), #61986, .T. ) ;
#35171 = CARTESIAN_POINT ( 'NONE',  ( 15.19999999999989093, 2.500000000000000000, 0.2464101615137735679 ) ) ;
#35172 = AXIS2_PLACEMENT_3D ( 'NONE', #97041, #49247, #127158 ) ;
#35173 = CARTESIAN_POINT ( 'NONE',  ( 21.23528140090977345, 2.699413673072321718, -2.293764360948945757 ) ) ;
#35174 = DIRECTION ( 'NONE',  ( -0.000000000000000000, -1.000000000000000000, -0.000000000000000000 ) ) ;
#35175 = ORIENTED_EDGE ( 'NONE', *, *, #24588, .T. ) ;
#35176 = ORIENTED_EDGE ( 'NONE', *, *, #98321, .T. ) ;
#35177 = DIRECTION ( 'NONE',  ( -0.000000000000000000, 1.000000000000000000, -0.000000000000000000 ) ) ;
#35178 = AXIS2_PLACEMENT_3D ( 'NONE', #104813, #127065, #15139 ) ;
#35179 = ORIENTED_EDGE ( 'NONE', *, *, #28557, .T. ) ;
#35180 = LINE ( 'NONE', #75086, #45769 ) ;
#35181 = FACE_OUTER_BOUND ( 'NONE', #63388, .T. ) ;
#35182 = ORIENTED_EDGE ( 'NONE', *, *, #78571, .F. ) ;
#35183 = LINE ( 'NONE', #2461, #54417 ) ;
#35184 = DIRECTION ( 'NONE',  ( 0.000000000000000000, 0.000000000000000000, -1.000000000000000000 ) ) ;
#35185 = CARTESIAN_POINT ( 'NONE',  ( 12.09999999999990195, 2.500000000000000000, 0.7928203230275495672 ) ) ;
#35186 = AXIS2_PLACEMENT_3D ( 'NONE', #34142, #2079, #31559 ) ;
#35187 = CYLINDRICAL_SURFACE ( 'NONE', #73038, 3.000000000000000444 ) ;
#35188 = ORIENTED_EDGE ( 'NONE', *, *, #107375, .T. ) ;
#35189 = DIRECTION ( 'NONE',  ( 0.000000000000000000, 0.000000000000000000, 1.000000000000000000 ) ) ;
#35191 = VECTOR ( 'NONE', #31529, 1000.000000000000000 ) ;
#35190 = AXIS2_PLACEMENT_3D ( 'NONE', #117238, #67498, #97630 ) ;
#35192 = DIRECTION ( 'NONE',  ( 0.000000000000000000, 0.000000000000000000, 1.000000000000000000 ) ) ;
#35193 = ORIENTED_EDGE ( 'NONE', *, *, #29814, .F. ) ;
#35194 = VERTEX_POINT ( 'NONE', #120888 ) ;
#35195 = CARTESIAN_POINT ( 'NONE',  ( 185.2135416670080872, 4.367472073101518859, -7.564683531249999149 ) ) ;
#35196 = CARTESIAN_POINT ( 'NONE',  ( 4.549999999999937650, 2.500000000000000000, 2.265063509461097357 ) ) ;
#35197 = CARTESIAN_POINT ( 'NONE',  ( -2.950000000000033484, 2.500000000000000000, -6.495190528383302464 ) ) ;
#35198 = PLANE ( 'NONE',  #57457 ) ;
#35199 = FACE_OUTER_BOUND ( 'NONE', #80853, .T. ) ;
#35200 = EDGE_CURVE ( 'NONE', #111361, #128844, #63913, .T. ) ;
#35201 = CYLINDRICAL_SURFACE ( 'NONE', #50940, 10.00000000000000000 ) ;
#35202 = CARTESIAN_POINT ( 'NONE',  ( -14.54999999999998472, 2.500000000000000000, 2.165063509461101265 ) ) ;
#35203 = DIRECTION ( 'NONE',  ( -0.000000000000000000, -1.000000000000000000, -0.000000000000000000 ) ) ;
#35204 = CARTESIAN_POINT ( 'NONE',  ( -11.89999999999999680, 2.500000000000000000, -4.776537180435975749 ) ) ;
#35205 = CARTESIAN_POINT ( 'NONE',  ( 4.199999999999938005, 2.500000000000000000, 4.330127018922196314 ) ) ;
#35206 = ADVANCED_FACE ( 'NONE', ( #31241 ), #99104, .T. ) ;
#35207 = VERTEX_POINT ( 'NONE', #82269 ) ;
#35208 = VERTEX_POINT ( 'NONE', #113653 ) ;
#35209 = CONICAL_SURFACE ( 'NONE', #28945, 0.09999999999999982514, 0.003490658503988666988 ) ;
#35210 = ORIENTED_EDGE ( 'NONE', *, *, #55918, .F. ) ;
#35211 = AXIS2_PLACEMENT_3D ( 'NONE', #9861, #51725, #1953 ) ;
#35212 = VECTOR ( 'NONE', #89566, 1000.000000000000000 ) ;
#35213 = EDGE_CURVE ( 'NONE', #97794, #61962, #80226, .T. ) ;
#35214 = ORIENTED_EDGE ( 'NONE', *, *, #86096, .F. ) ;
#35215 = PLANE ( 'NONE',  #123063 ) ;
#35216 = EDGE_CURVE ( 'NONE', #122967, #46749, #73082, .T. ) ;
#35217 = FACE_OUTER_BOUND ( 'NONE', #16346, .T. ) ;
#35218 = CARTESIAN_POINT ( 'NONE',  ( -8.150000000000009237, 2.500000000000000000, 6.741600689897071952 ) ) ;
#35219 = EDGE_LOOP ( 'NONE', ( #115291, #93257, #37292, #51669 ) ) ;
#35220 = VECTOR ( 'NONE', #111282, 1000.000000000000000 ) ;
#35221 = DIRECTION ( 'NONE',  ( 0.000000000000000000, 0.000000000000000000, 1.000000000000000000 ) ) ;
#35222 = AXIS2_PLACEMENT_3D ( 'NONE', #41786, #123527, #1188 ) ;
#35223 = EDGE_CURVE ( 'NONE', #6156, #52245, #63500, .T. ) ;
#35224 = DIRECTION ( 'NONE',  ( 0.000000000000000000, 0.000000000000000000, 1.000000000000000000 ) ) ;
#35226 = VERTEX_POINT ( 'NONE', #72447 ) ;
#35225 = CARTESIAN_POINT ( 'NONE',  ( 8.349999999999923261, 12.50000000000000000, -6.495190528383302464 ) ) ;
#35227 = EDGE_CURVE ( 'NONE', #44931, #67896, #83560, .T. ) ;
#35228 = CARTESIAN_POINT ( 'NONE',  ( -8.950000000000008171, 2.500000000000000000, 1.818653347947321475 ) ) ;
#35229 = ORIENTED_EDGE ( 'NONE', *, *, #84326, .T. ) ;
#35230 = AXIS2_PLACEMENT_3D ( 'NONE', #41961, #61608, #101520 ) ;
#35231 = ORIENTED_EDGE ( 'NONE', *, *, #85313, .T. ) ;
#35232 = VERTEX_POINT ( 'NONE', #101254 ) ;
#35233 = ORIENTED_EDGE ( 'NONE', *, *, #89963, .F. ) ;
#35234 = FACE_OUTER_BOUND ( 'NONE', #3451, .T. ) ;
#35235 = DIRECTION ( 'NONE',  ( 0.000000000000000000, 0.000000000000000000, 1.000000000000000000 ) ) ;
#35236 = CARTESIAN_POINT ( 'NONE',  ( -3.644143946350442628E-14, 2.500000000000000000, 0.5928203230275517210 ) ) ;
#35237 = CARTESIAN_POINT ( 'NONE',  ( -2.050000000000033129, 2.500000000000000000, 2.165063509461097713 ) ) ;
#35238 = EDGE_LOOP ( 'NONE', ( #126767, #83287 ) ) ;
#35239 = DIRECTION ( 'NONE',  ( -0.000000000000000000, -1.000000000000000000, -0.000000000000000000 ) ) ;
#35240 = ORIENTED_EDGE ( 'NONE', *, *, #58610, .F. ) ;
#35241 = AXIS2_PLACEMENT_3D ( 'NONE', #45349, #85884, #114711 ) ;
#35242 = CARTESIAN_POINT ( 'NONE',  ( 59.74180401167438959, -3.401974578012062267, -5.439313020133131005 ) ) ;
#35243 = CARTESIAN_POINT ( 'NONE',  ( 10.84999999999990905, 2.500000000000000000, -6.495190528383302464 ) ) ;
#35244 = CARTESIAN_POINT ( 'NONE',  ( 108.0000000000000142, 8.500000000000000000, 0.000000000000000000 ) ) ;
#35245 = CARTESIAN_POINT ( 'NONE',  ( -12.89999999999999147, 2.500000000000000000, -0.6928203230275500335 ) ) ;
#35246 = EDGE_LOOP ( 'NONE', ( #5408, #54542 ) ) ;
#35247 = ADVANCED_FACE ( 'NONE', ( #81608 ), #33801, .T. ) ;
#35248 = STYLED_ITEM ( 'NONE', ( #111273 ), #2393 ) ;
#35249 = ORIENTED_EDGE ( 'NONE', *, *, #82414, .F. ) ;
#35250 = VERTEX_POINT ( 'NONE', #23989 ) ;
#35251 = CARTESIAN_POINT ( 'NONE',  ( 13.29999999999989946, 2.500000000000000000, -2.385244779468109755E-15 ) ) ;
#35252 = DIRECTION ( 'NONE',  ( 0.000000000000000000, 0.000000000000000000, 1.000000000000000000 ) ) ;
#35253 = CARTESIAN_POINT ( 'NONE',  ( 2.499999999999948930, 2.500000000000000000, -5.022947341949754119 ) ) ;
#35254 = FACE_BOUND ( 'NONE', #35034, .T. ) ;
#35255 = CARTESIAN_POINT ( 'NONE',  ( -14.14999999999998614, 2.500000000000000000, -2.757883832488651876 ) ) ;
#35256 = DIRECTION ( 'NONE',  ( 0.000000000000000000, 0.000000000000000000, 1.000000000000000000 ) ) ;
#35257 = CONICAL_SURFACE ( 'NONE', #129359, 0.1000000000000000472, 0.003490658503988666988 ) ;
#35258 = EDGE_CURVE ( 'NONE', #86589, #2147, #43013, .T. ) ;
#35259 = DIRECTION ( 'NONE',  ( 0.000000000000000000, 0.000000000000000000, 1.000000000000000000 ) ) ;
#35260 = VECTOR ( 'NONE', #31520, 1000.000000000000000 ) ;
#35261 = EDGE_CURVE ( 'NONE', #129348, #84561, #1115, .T. ) ;
#35262 = FACE_OUTER_BOUND ( 'NONE', #88717, .T. ) ;
#35263 = DIRECTION ( 'NONE',  ( 0.000000000000000000, 1.000000000000000000, 0.000000000000000000 ) ) ;
#35264 = AXIS2_PLACEMENT_3D ( 'NONE', #29647, #110139, #109497 ) ;
#35265 = ADVANCED_FACE ( 'NONE', ( #43642 ), #23791, .T. ) ;
#35266 = PLANE ( 'NONE',  #3037 ) ;
#35267 = ORIENTED_EDGE ( 'NONE', *, *, #103226, .F. ) ;
#35268 = EDGE_CURVE ( 'NONE', #73774, #45181, #17504, .T. ) ;
#35269 = DIRECTION ( 'NONE',  ( 0.000000000000000000, 1.000000000000000000, 0.000000000000000000 ) ) ;
#35271 = EDGE_CURVE ( 'NONE', #14509, #113423, #61336, .T. ) ;
#35270 = CIRCLE ( 'NONE', #48074, 0.1000000000000002554 ) ;
#35272 = ORIENTED_EDGE ( 'NONE', *, *, #45150, .T. ) ;
#35273 = VERTEX_POINT ( 'NONE', #123457 ) ;
#35274 = VERTEX_POINT ( 'NONE', #91433 ) ;
#35275 = ORIENTED_EDGE ( 'NONE', *, *, #72646, .T. ) ;
#35276 = VECTOR ( 'NONE', #86116, 1000.000000000000000 ) ;
#35277 = CARTESIAN_POINT ( 'NONE',  ( 4.349999999999940137, 12.50000000000000000, -6.841600689897078702 ) ) ;
#35278 = FACE_BOUND ( 'NONE', #111773, .T. ) ;
#35279 = PLANE ( 'NONE',  #70307 ) ;
#35280 = ADVANCED_FACE ( 'NONE', ( #1752 ), #38472, .T. ) ;
#35282 = EDGE_CURVE ( 'NONE', #82263, #103538, #4984, .T. ) ;
#35281 = CONICAL_SURFACE ( 'NONE', #3865, 0.1000000000000002554, 0.003490658503988666988 ) ;
#35283 = ORIENTED_EDGE ( 'NONE', *, *, #47531, .T. ) ;
#35284 = DIRECTION ( 'NONE',  ( -0.000000000000000000, -1.000000000000000000, -0.000000000000000000 ) ) ;
#35285 = DIRECTION ( 'NONE',  ( -0.000000000000000000, 1.000000000000000000, -0.000000000000000000 ) ) ;
#35286 = ORIENTED_EDGE ( 'NONE', *, *, #123945, .T. ) ;
#35287 = DIRECTION ( 'NONE',  ( -4.274815082592931898E-19, -0.9999939076577903929, -0.003490651415223739937 ) ) ;
#35288 = CARTESIAN_POINT ( 'NONE',  ( 7.049999999999926992, 2.500000000000000000, 2.165063509461097713 ) ) ;
#35289 = VERTEX_POINT ( 'NONE', #113005 ) ;
#35290 = CIRCLE ( 'NONE', #95910, 0.1000000000000002554 ) ;
#35291 = CARTESIAN_POINT ( 'NONE',  ( 11.24999999999994316, 2.500000000000000000, -6.495190528383302464 ) ) ;
#35292 = CARTESIAN_POINT ( 'NONE',  ( -6.650000000000014566, 2.500000000000000000, 1.472243186433545459 ) ) ;
#35293 = VERTEX_POINT ( 'NONE', #63260 ) ;
#35294 = CIRCLE ( 'NONE', #41563, 0.06509327318403745899 ) ;
#35295 = DIRECTION ( 'NONE',  ( 0.000000000000000000, 1.000000000000000000, 0.000000000000000000 ) ) ;
#35296 = DIRECTION ( 'NONE',  ( 0.000000000000000000, 0.000000000000000000, -1.000000000000000000 ) ) ;
#35297 = AXIS2_PLACEMENT_3D ( 'NONE', #63977, #103901, #15502 ) ;
#35298 = DIRECTION ( 'NONE',  ( 0.000000000000000000, 0.000000000000000000, 1.000000000000000000 ) ) ;
#35299 = VERTEX_POINT ( 'NONE', #115563 ) ;
#35300 = EDGE_LOOP ( 'NONE', ( #128036, #23184 ) ) ;
#35301 = DIRECTION ( 'NONE',  ( 0.000000000000000000, 0.000000000000000000, 1.000000000000000000 ) ) ;
#35303 = ORIENTED_EDGE ( 'NONE', *, *, #33531, .T. ) ;
#35302 = AXIS2_PLACEMENT_3D ( 'NONE', #9442, #119378, #99761 ) ;
#35304 = CARTESIAN_POINT ( 'NONE',  ( 9.599999999999917932, 12.50000000000000000, -0.6277270498435166823 ) ) ;
#35305 = FACE_OUTER_BOUND ( 'NONE', #86947, .T. ) ;
#35306 = AXIS2_PLACEMENT_3D ( 'NONE', #67324, #37272, #126936 ) ;
#35307 = AXIS2_PLACEMENT_3D ( 'NONE', #86830, #84248, #16137 ) ;
#35308 = ORIENTED_EDGE ( 'NONE', *, *, #47085, .F. ) ;
#35309 = CARTESIAN_POINT ( 'NONE',  ( 13.34999999999989662, 2.500000000000000000, -1.472243186433550122 ) ) ;
#35310 = LINE ( 'NONE', #64748, #49786 ) ;
#35311 = CARTESIAN_POINT ( 'NONE',  ( 10.84999999999991260, 2.500000000000000000, 6.595190528383296780 ) ) ;
#35312 = CARTESIAN_POINT ( 'NONE',  ( -1.650000000000034772, 2.500000000000000000, 6.495190528383297135 ) ) ;
#35313 = CARTESIAN_POINT ( 'NONE',  ( -0.4000000000000339950, 2.500000000000000000, 0.7928203230275517877 ) ) ;
#35314 = VECTOR ( 'NONE', #30592, 1000.000000000000000 ) ;
#35315 = ORIENTED_EDGE ( 'NONE', *, *, #66152, .T. ) ;
#35316 = EDGE_CURVE ( 'NONE', #46102, #62111, #35740, .T. ) ;
#35318 = ORIENTED_EDGE ( 'NONE', *, *, #126679, .F. ) ;
#35317 = CIRCLE ( 'NONE', #64639, 0.06509327318403741736 ) ;
#35319 = DIRECTION ( 'NONE',  ( 1.000000000000000000, -0.000000000000000000, -1.084202172485504434E-16 ) ) ;
#35320 = DIRECTION ( 'NONE',  ( 0.000000000000000000, 0.000000000000000000, 1.000000000000000000 ) ) ;
#35321 = DIRECTION ( 'NONE',  ( 0.000000000000000000, -0.000000000000000000, 1.000000000000000000 ) ) ;
#35323 = ORIENTED_EDGE ( 'NONE', *, *, #125936, .F. ) ;
#35322 = ORIENTED_EDGE ( 'NONE', *, *, #70510, .F. ) ;
#35324 = ORIENTED_EDGE ( 'NONE', *, *, #109075, .T. ) ;
#35325 = CARTESIAN_POINT ( 'NONE',  ( 6.249999999999930722, 2.500000000000000000, 7.188010851410848723 ) ) ;
#35326 = FACE_OUTER_BOUND ( 'NONE', #114303, .T. ) ;
#35327 = CARTESIAN_POINT ( 'NONE',  ( -14.39999999999998614, 2.500000000000000000, 0.4464101615137758272 ) ) ;
#35328 = DIRECTION ( 'NONE',  ( 0.000000000000000000, 0.000000000000000000, 1.000000000000000000 ) ) ;
#35329 = LINE ( 'NONE', #123675, #104597 ) ;
#35330 = FACE_OUTER_BOUND ( 'NONE', #11142, .T. ) ;
#35331 = CARTESIAN_POINT ( 'NONE',  ( 11.44999999999991047, 2.500000000000000000, 6.148780366869520009 ) ) ;
#35332 = AXIS2_PLACEMENT_3D ( 'NONE', #57421, #86864, #5718 ) ;
#35333 = CARTESIAN_POINT ( 'NONE',  ( -0.6500000000000389910, 2.500000000000000000, -1.718653347947326049 ) ) ;
#35334 = CARTESIAN_POINT ( 'NONE',  ( 6.849999999999927702, 2.500000000000000000, 2.411473670974873862 ) ) ;
#35335 = ORIENTED_EDGE ( 'NONE', *, *, #99090, .F. ) ;
#35336 = AXIS2_PLACEMENT_3D ( 'NONE', #16011, #16651, #45508 ) ;
#35337 = FACE_OUTER_BOUND ( 'NONE', #1943, .T. ) ;
#35338 = EDGE_LOOP ( 'NONE', ( #47462, #64052, #112195, #96188 ) ) ;
#35339 = VERTEX_POINT ( 'NONE', #25249 ) ;
#35340 = CARTESIAN_POINT ( 'NONE',  ( 2.099999999999948574, 2.500000000000000000, 3.637306695894644726 ) ) ;
#35341 = CARTESIAN_POINT ( 'NONE',  ( 10.84999999999990905, 12.50000000000000000, -7.188010851410854052 ) ) ;
#35342 = CIRCLE ( 'NONE', #31150, 0.09999999999999999167 ) ;
#35343 = DIRECTION ( 'NONE',  ( -0.000000000000000000, -1.000000000000000000, -0.000000000000000000 ) ) ;
#35345 = CIRCLE ( 'NONE', #60399, 0.06509327318403745899 ) ;
#35344 = CARTESIAN_POINT ( 'NONE',  ( 15.79999999999989058, 2.500000000000000000, -2.385244779468109755E-15 ) ) ;
#35346 = DIRECTION ( 'NONE',  ( -0.000000000000000000, -1.000000000000000000, -0.000000000000000000 ) ) ;
#35347 = PLANE ( 'NONE',  #57651 ) ;
#35348 = CARTESIAN_POINT ( 'NONE',  ( 1.649999999999951505, 2.500000000000000000, -2.857883832488653741 ) ) ;
#35349 = ORIENTED_EDGE ( 'NONE', *, *, #24438, .T. ) ;
#35350 = FACE_OUTER_BOUND ( 'NONE', #39556, .T. ) ;
#35351 = AXIS2_PLACEMENT_3D ( 'NONE', #124660, #35007, #6149 ) ;
#35352 = DIRECTION ( 'NONE',  ( 0.000000000000000000, 1.000000000000000000, 0.000000000000000000 ) ) ;
#35353 = ORIENTED_EDGE ( 'NONE', *, *, #87762, .T. ) ;
#35354 = ADVANCED_FACE ( 'NONE', ( #35113 ), #116216, .T. ) ;
#35355 = ORIENTED_EDGE ( 'NONE', *, *, #79761, .T. ) ;
#35357 = CIRCLE ( 'NONE', #16454, 0.1000000000000002554 ) ;
#35356 = VECTOR ( 'NONE', #12492, 1000.000000000000000 ) ;
#35358 = EDGE_LOOP ( 'NONE', ( #84518, #95797, #108790, #99836 ) ) ;
#35359 = ADVANCED_FACE ( 'NONE', ( #15429 ), #16710, .T. ) ;
#35360 = ORIENTED_EDGE ( 'NONE', *, *, #86693, .F. ) ;
#35361 = EDGE_CURVE ( 'NONE', #45135, #87037, #45569, .T. ) ;
#35362 = FACE_OUTER_BOUND ( 'NONE', #21448, .T. ) ;
#35363 = FACE_OUTER_BOUND ( 'NONE', #63344, .T. ) ;
#35364 = AXIS2_PLACEMENT_3D ( 'NONE', #60674, #20096, #99303 ) ;
#35365 = FACE_OUTER_BOUND ( 'NONE', #1682, .T. ) ;
#35366 = PLANE ( 'NONE',  #111346 ) ;
#35367 = EDGE_CURVE ( 'NONE', #26681, #87979, #30150, .T. ) ;
#35368 = DIRECTION ( 'NONE',  ( 0.000000000000000000, 0.000000000000000000, 1.000000000000000000 ) ) ;
#35370 = VERTEX_POINT ( 'NONE', #14146 ) ;
#35369 = EDGE_CURVE ( 'NONE', #99741, #99122, #53125, .T. ) ;
#35371 = DIRECTION ( 'NONE',  ( -0.000000000000000000, 1.000000000000000000, -0.000000000000000000 ) ) ;
#35372 = ADVANCED_FACE ( 'NONE', ( #54090 ), #124762, .T. ) ;
#35373 = DIRECTION ( 'NONE',  ( 0.000000000000000000, 1.000000000000000000, 0.000000000000000000 ) ) ;
#35374 = DIRECTION ( 'NONE',  ( 0.000000000000000000, -0.9999939076577903929, 0.003490651415223739937 ) ) ;
#35375 = ORIENTED_EDGE ( 'NONE', *, *, #57580, .T. ) ;
#35376 = ORIENTED_EDGE ( 'NONE', *, *, #104834, .T. ) ;
#35377 = ORIENTED_EDGE ( 'NONE', *, *, #20346, .T. ) ;
#35378 = CARTESIAN_POINT ( 'NONE',  ( 3.749999999999944045, 12.50000000000000000, -7.188010851410854052 ) ) ;
#35379 = DIRECTION ( 'NONE',  ( -0.000000000000000000, 1.000000000000000000, -0.000000000000000000 ) ) ;
#35380 = DIRECTION ( 'NONE',  ( 0.000000000000000000, 0.000000000000000000, 1.000000000000000000 ) ) ;
#35381 = VECTOR ( 'NONE', #106519, 1000.000000000000000 ) ;
#35382 = ORIENTED_EDGE ( 'NONE', *, *, #121357, .F. ) ;
#35383 = DIRECTION ( 'NONE',  ( 0.000000000000000000, 1.000000000000000000, 0.000000000000000000 ) ) ;
#35384 = DIRECTION ( 'NONE',  ( 0.000000000000000000, 1.000000000000000000, 0.000000000000000000 ) ) ;
#35385 = DIRECTION ( 'NONE',  ( 0.000000000000000000, 0.000000000000000000, 1.000000000000000000 ) ) ;
#35386 = DIRECTION ( 'NONE',  ( 0.000000000000000000, 0.000000000000000000, 1.000000000000000000 ) ) ;
#35387 = CARTESIAN_POINT ( 'NONE',  ( 8.749999999999918288, 12.50000000000000000, 7.253104124594885960 ) ) ;
#35388 = AXIS2_PLACEMENT_3D ( 'NONE', #11366, #98444, #38931 ) ;
#35389 = CONICAL_SURFACE ( 'NONE', #108543, 0.09999999999999982514, 0.003490658503988666988 ) ;
#35390 = ORIENTED_EDGE ( 'NONE', *, *, #113084, .F. ) ;
#35391 = AXIS2_PLACEMENT_3D ( 'NONE', #23553, #112595, #63487 ) ;
#35392 = DIRECTION ( 'NONE',  ( 0.000000000000000000, 1.000000000000000000, 0.000000000000000000 ) ) ;
#35393 = VERTEX_POINT ( 'NONE', #114925 ) ;
#35394 = ORIENTED_EDGE ( 'NONE', *, *, #53522, .T. ) ;
#35395 = VERTEX_POINT ( 'NONE', #94008 ) ;
#35396 = ADVANCED_FACE ( 'NONE', ( #4969 ), #103302, .T. ) ;
#35397 = CARTESIAN_POINT ( 'NONE',  ( 2.499999999999983569, 2.500000000000000000, 0.09999999999999772959 ) ) ;
#35398 = FACE_BOUND ( 'NONE', #88386, .T. ) ;
#35399 = CIRCLE ( 'NONE', #56307, 0.06509327318403745899 ) ;
#35400 = CARTESIAN_POINT ( 'NONE',  ( 11.24999999999990941, 12.50000000000000000, 7.188010851410848723 ) ) ;
#35401 = CARTESIAN_POINT ( 'NONE',  ( -8.150000000000009237, 2.500000000000000000, 6.148780366869520009 ) ) ;
#35402 = CARTESIAN_POINT ( 'NONE',  ( 13.14999999999989733, 12.50000000000000000, -1.818653347947325916 ) ) ;
#35403 = AXIS2_PLACEMENT_3D ( 'NONE', #102345, #52587, #83353 ) ;
#35404 = VECTOR ( 'NONE', #29595, 1000.000000000000000 ) ;
#35405 = ADVANCED_FACE ( 'NONE', ( #76953 ), #25922, .T. ) ;
#35406 = VERTEX_POINT ( 'NONE', #65828 ) ;
#35407 = ADVANCED_FACE ( 'NONE', ( #44254 ), #5608, .F. ) ;
#35408 = CARTESIAN_POINT ( 'NONE',  ( 5.849999999999933031, 2.500000000000000000, -1.472243186433550122 ) ) ;
#35409 = LINE ( 'NONE', #64848, #9283 ) ;
#35410 = PLANE ( 'NONE',  #109270 ) ;
#35411 = EDGE_CURVE ( 'NONE', #123035, #88198, #25635, .T. ) ;
#35412 = DIRECTION ( 'NONE',  ( 0.000000000000000000, 0.000000000000000000, 1.000000000000000000 ) ) ;
#35413 = ORIENTED_EDGE ( 'NONE', *, *, #29269, .T. ) ;
#35414 = LINE ( 'NONE', #125072, #105460 ) ;
#35415 = CARTESIAN_POINT ( 'NONE',  ( -3.350000000000028955, 2.500000000000000000, 2.165063509461097713 ) ) ;
#35416 = CIRCLE ( 'NONE', #70923, 3.000000000000000000 ) ;
#35417 = ADVANCED_FACE ( 'NONE', ( #84180 ), #44514, .T. ) ;
#35418 = EDGE_LOOP ( 'NONE', ( #58429, #87320 ) ) ;
#35419 = DIRECTION ( 'NONE',  ( 0.000000000000000000, 1.000000000000000000, 0.000000000000000000 ) ) ;
#35420 = ADVANCED_FACE ( 'NONE', ( #54715 ), #44922, .T. ) ;
#35421 = ORIENTED_EDGE ( 'NONE', *, *, #116966, .F. ) ;
#35422 = FACE_BOUND ( 'NONE', #123309, .T. ) ;
#35423 = DIRECTION ( 'NONE',  ( -0.000000000000000000, 1.000000000000000000, -0.000000000000000000 ) ) ;
#35424 = ADVANCED_FACE ( 'NONE', ( #6250 ), #46196, .T. ) ;
#35425 = EDGE_CURVE ( 'NONE', #29584, #11046, #69546, .T. ) ;
#35426 = ADVANCED_FACE ( 'NONE', ( #50096 ), #13397, .T. ) ;
#35427 = EDGE_LOOP ( 'NONE', ( #120336, #51491, #121938, #63301 ) ) ;
#35428 = DIRECTION ( 'NONE',  ( -0.000000000000000000, -1.000000000000000000, -0.000000000000000000 ) ) ;
#35429 = CARTESIAN_POINT ( 'NONE',  ( -0.8500000000000382805, 2.500000000000000000, -1.372243186433550033 ) ) ;
#35430 = ORIENTED_EDGE ( 'NONE', *, *, #59221, .F. ) ;
#35431 = ORIENTED_EDGE ( 'NONE', *, *, #111788, .T. ) ;
#35432 = CARTESIAN_POINT ( 'NONE',  ( 186.3802083336747444, 4.367472073101515306, 7.564683531250000925 ) ) ;
#35433 = AXIS2_PLACEMENT_3D ( 'NONE', #63019, #104232, #24386 ) ;
#35434 = EDGE_CURVE ( 'NONE', #43040, #86788, #123925, .T. ) ;
#35435 = ORIENTED_EDGE ( 'NONE', *, *, #33167, .T. ) ;
#35436 = CARTESIAN_POINT ( 'NONE',  ( 185.9218750003414016, 0.000000000000000000, 7.564683531250000925 ) ) ;
#35437 = CARTESIAN_POINT ( 'NONE',  ( -2.700000000000029932, 2.500000000000000000, -4.676537180435977881 ) ) ;
#35438 = DIRECTION ( 'NONE',  ( 0.000000000000000000, 0.000000000000000000, 1.000000000000000000 ) ) ;
#35439 = LINE ( 'NONE', #103530, #9190 ) ;
#35440 = DIRECTION ( 'NONE',  ( -0.000000000000000000, -1.000000000000000000, -0.000000000000000000 ) ) ;
#35441 = CARTESIAN_POINT ( 'NONE',  ( 13.34999999999990017, 2.500000000000000000, 2.165063509461097713 ) ) ;
#35442 = AXIS2_PLACEMENT_3D ( 'NONE', #10645, #11959, #30990 ) ;
#35443 = VERTEX_POINT ( 'NONE', #40259 ) ;
#35444 = VERTEX_POINT ( 'NONE', #19305 ) ;
#35445 = CARTESIAN_POINT ( 'NONE',  ( -7.700000000000016165, 12.50000000000000000, -3.983716857408426293 ) ) ;
#35446 = AXIS2_PLACEMENT_3D ( 'NONE', #101250, #39144, #31239 ) ;
#35447 = CARTESIAN_POINT ( 'NONE',  ( 187.2500000000000000, 9.429780353434619030E-16, -7.700000000000000178 ) ) ;
#35448 = CARTESIAN_POINT ( 'NONE',  ( 12.29999999999990479, 2.500000000000000000, 4.676537180435972552 ) ) ;
#35449 = DIRECTION ( 'NONE',  ( -0.000000000000000000, 1.000000000000000000, -0.000000000000000000 ) ) ;
#35450 = VECTOR ( 'NONE', #67620, 1000.000000000000000 ) ;
#35452 = ORIENTED_EDGE ( 'NONE', *, *, #85886, .F. ) ;
#35451 = VERTEX_POINT ( 'NONE', #88028 ) ;
#35453 = FACE_BOUND ( 'NONE', #21898, .T. ) ;
#35454 = ORIENTED_EDGE ( 'NONE', *, *, #54206, .T. ) ;
#35455 = EDGE_CURVE ( 'NONE', #72066, #96049, #2639, .T. ) ;
#35456 = DIRECTION ( 'NONE',  ( -0.000000000000000000, 1.000000000000000000, -0.000000000000000000 ) ) ;
#35457 = CARTESIAN_POINT ( 'NONE',  ( 13.74999999999993072, 12.50000000000000000, -2.165063509461101710 ) ) ;
#35458 = VERTEX_POINT ( 'NONE', #127985 ) ;
#35459 = FACE_OUTER_BOUND ( 'NONE', #113070, .T. ) ;
#35461 = DIRECTION ( 'NONE',  ( -0.000000000000000000, 1.000000000000000000, -0.000000000000000000 ) ) ;
#35460 = VECTOR ( 'NONE', #37657, 1000.000000000000000 ) ;
#35462 = DIRECTION ( 'NONE',  ( 0.000000000000000000, 0.000000000000000000, 1.000000000000000000 ) ) ;
#35463 = FACE_OUTER_BOUND ( 'NONE', #68516, .T. ) ;
#35464 = CARTESIAN_POINT ( 'NONE',  ( -0.8000000000000381251, 12.50000000000000000, 4.395220292106234439 ) ) ;
#35465 = DIRECTION ( 'NONE',  ( -4.274815082592931898E-19, -0.9999939076577903929, -0.003490651415223739937 ) ) ;
#35466 = CARTESIAN_POINT ( 'NONE',  ( 187.2343750003414016, 8.734944146203032389, 5.348610694689227483E-16 ) ) ;
#35467 = LINE ( 'NONE', #16429, #40170 ) ;
#35468 = DIRECTION ( 'NONE',  ( 0.000000000000000000, 0.000000000000000000, -1.000000000000000000 ) ) ;
#35469 = ORIENTED_EDGE ( 'NONE', *, *, #70738, .T. ) ;
#35470 = EDGE_CURVE ( 'NONE', #6533, #45263, #77963, .T. ) ;
#35471 = EDGE_LOOP ( 'NONE', ( #72086, #126382, #94186, #30398 ) ) ;
#35472 = DIRECTION ( 'NONE',  ( -0.000000000000000000, 1.000000000000000000, -0.000000000000000000 ) ) ;
#35473 = VERTEX_POINT ( 'NONE', #38330 ) ;
#35474 = CARTESIAN_POINT ( 'NONE',  ( -11.25000000000000000, 2.500000000000000000, -2.957883832488649833 ) ) ;
#35475 = AXIS2_PLACEMENT_3D ( 'NONE', #107566, #57823, #80034 ) ;
#35477 = ORIENTED_EDGE ( 'NONE', *, *, #73503, .T. ) ;
#35476 = VERTEX_POINT ( 'NONE', #69056 ) ;
#35478 = ORIENTED_EDGE ( 'NONE', *, *, #97301, .T. ) ;
#35479 = DIRECTION ( 'NONE',  ( -4.274815082592931898E-19, -0.9999939076577903929, -0.003490651415223739937 ) ) ;
#35480 = CIRCLE ( 'NONE', #89834, 0.06509327318403745899 ) ;
#35481 = CONICAL_SURFACE ( 'NONE', #33431, 0.09999999999999999167, 0.003490658503988666988 ) ;
#35482 = DIRECTION ( 'NONE',  ( 0.000000000000000000, 1.000000000000000000, 0.000000000000000000 ) ) ;
#35483 = FILL_AREA_STYLE ('',( #66208 ) ) ;
#35484 = DIRECTION ( 'NONE',  ( 0.000000000000000000, -0.9999939076577903929, 0.003490651415223739937 ) ) ;
#35485 = CARTESIAN_POINT ( 'NONE',  ( 3.149999999999942624, 12.50000000000000000, 6.776507416713035248 ) ) ;
#35486 = CARTESIAN_POINT ( 'NONE',  ( 6.249999999999934275, 12.50000000000000000, -7.188010851410854052 ) ) ;
#35487 = EDGE_CURVE ( 'NONE', #88829, #52488, #57024, .T. ) ;
#35488 = EDGE_LOOP ( 'NONE', ( #29311, #122070 ) ) ;
#35489 = VECTOR ( 'NONE', #123259, 1000.000000000000000 ) ;
#35492 = CONICAL_SURFACE ( 'NONE', #6210, 0.1000000000000002554, 0.003490658503988666988 ) ;
#35491 = DIRECTION ( 'NONE',  ( 0.000000000000000000, 0.000000000000000000, -1.000000000000000000 ) ) ;
#35490 = VECTOR ( 'NONE', #83488, 1000.000000000000000 ) ;
#35493 = VERTEX_POINT ( 'NONE', #57964 ) ;
#35494 = ORIENTED_EDGE ( 'NONE', *, *, #6387, .F. ) ;
#35495 = VERTEX_POINT ( 'NONE', #89354 ) ;
#35496 = CARTESIAN_POINT ( 'NONE',  ( -7.100000000000017408, 2.500000000000000000, -0.6928203230275542523 ) ) ;
#35497 = ORIENTED_EDGE ( 'NONE', *, *, #73031, .F. ) ;
#35498 = VERTEX_POINT ( 'NONE', #28504 ) ;
#35499 = EDGE_LOOP ( 'NONE', ( #79788, #67645, #78936, #46086 ) ) ;
#35500 = AXIS2_PLACEMENT_3D ( 'NONE', #46682, #126535, #36871 ) ;
#35501 = DIRECTION ( 'NONE',  ( -0.000000000000000000, -1.000000000000000000, -0.000000000000000000 ) ) ;
#35502 = AXIS2_PLACEMENT_3D ( 'NONE', #34260, #74171, #101699 ) ;
#35503 = DIRECTION ( 'NONE',  ( 0.000000000000000000, 0.000000000000000000, 1.000000000000000000 ) ) ;
#35504 = CARTESIAN_POINT ( 'NONE',  ( -9.800000000000004263, 12.50000000000000000, -0.3464101615137783474 ) ) ;
#35505 = AXIS2_PLACEMENT_3D ( 'NONE', #66297, #125225, #115370 ) ;
#35506 = DIRECTION ( 'NONE',  ( 0.000000000000000000, -0.000000000000000000, 1.000000000000000000 ) ) ;
#35507 = FACE_OUTER_BOUND ( 'NONE', #58241, .T. ) ;
#35508 = CARTESIAN_POINT ( 'NONE',  ( -6.900000000000019007, 2.500000000000000000, 0.2464101615137735679 ) ) ;
#35509 = ORIENTED_EDGE ( 'NONE', *, *, #92391, .T. ) ;
#35510 = CARTESIAN_POINT ( 'NONE',  ( -5.450000000000023270, 2.500000000000000000, -2.265063509461101798 ) ) ;
#35511 = AXIS2_PLACEMENT_3D ( 'NONE', #83211, #84494, #124419 ) ;
#35512 = EDGE_LOOP ( 'NONE', ( #112841, #19823 ) ) ;
#35513 = CARTESIAN_POINT ( 'NONE',  ( 6.899999999999926636, 2.500000000000000000, -0.3464101615137782364 ) ) ;
#35514 = EDGE_CURVE ( 'NONE', #24394, #114462, #11051, .T. ) ;
#35515 = EDGE_LOOP ( 'NONE', ( #83371, #69777 ) ) ;
#35516 = CARTESIAN_POINT ( 'NONE',  ( 184.7500000000000000, 9.429780353434619030E-16, -7.700000000000000178 ) ) ;
#35517 = CIRCLE ( 'NONE', #54280, 0.06509327318403745899 ) ;
#35518 = ORIENTED_EDGE ( 'NONE', *, *, #7640, .T. ) ;
#35519 = VERTEX_POINT ( 'NONE', #107039 ) ;
#35520 = ADVANCED_FACE ( 'NONE', ( #8838 ), #17293, .T. ) ;
#35521 = LINE ( 'NONE', #95723, #36493 ) ;
#35522 = CARTESIAN_POINT ( 'NONE',  ( 9.149999999999916866, 2.500000000000000000, -2.757883832488654097 ) ) ;
#35523 = DIRECTION ( 'NONE',  ( 0.000000000000000000, 0.000000000000000000, 1.000000000000000000 ) ) ;
#35524 = FACE_OUTER_BOUND ( 'NONE', #95406, .T. ) ;
#35525 = ADVANCED_FACE ( 'NONE', ( #68410 ), #34062, .T. ) ;
#35526 = CARTESIAN_POINT ( 'NONE',  ( 4.149999999999938183, 12.50000000000000000, 2.230156782645134950 ) ) ;
#35528 = ORIENTED_EDGE ( 'NONE', *, *, #2584, .F. ) ;
#35527 = EDGE_CURVE ( 'NONE', #91704, #14107, #50784, .T. ) ;
#35529 = DIRECTION ( 'NONE',  ( 0.000000000000000000, -0.000000000000000000, 1.000000000000000000 ) ) ;
#35530 = FACE_OUTER_BOUND ( 'NONE', #13230, .T. ) ;
#35531 = EDGE_CURVE ( 'NONE', #39312, #91186, #59268, .T. ) ;
#35532 = DIRECTION ( 'NONE',  ( -0.000000000000000000, 1.000000000000000000, -0.000000000000000000 ) ) ;
#35533 = EDGE_CURVE ( 'NONE', #119152, #93088, #90467, .T. ) ;
#35534 = ADVANCED_FACE ( 'NONE', ( #118806 ), #19971, .T. ) ;
#35535 = PLANE ( 'NONE',  #101553 ) ;
#35536 = DIRECTION ( 'NONE',  ( -4.274815082592931898E-19, -0.9999939076577903929, -0.003490651415223739937 ) ) ;
#35537 = VERTEX_POINT ( 'NONE', #77577 ) ;
#35538 = EDGE_LOOP ( 'NONE', ( #37605, #120729, #90476, #125857 ) ) ;
#35539 = VECTOR ( 'NONE', #59494, 1000.000000000000000 ) ;
#35540 = EDGE_CURVE ( 'NONE', #31716, #128537, #27846, .T. ) ;
#35541 = VERTEX_POINT ( 'NONE', #108336 ) ;
#35542 = EDGE_CURVE ( 'NONE', #102877, #36999, #86262, .T. ) ;
#35543 = CARTESIAN_POINT ( 'NONE',  ( 9.149999999999915090, 2.500000000000000000, 6.495190528383297135 ) ) ;
#35544 = CARTESIAN_POINT ( 'NONE',  ( 1.449999999999952216, 2.500000000000000000, -2.511473670974877948 ) ) ;
#35545 = ADVANCED_FACE ( 'NONE', ( #97871 ), #61253, .T. ) ;
#35546 = AXIS2_PLACEMENT_3D ( 'NONE', #28495, #67088, #116211 ) ;
#35547 = CARTESIAN_POINT ( 'NONE',  ( 187.4583333333333428, 4.445597072760117285, 7.699999999999999289 ) ) ;
#35548 = DIRECTION ( 'NONE',  ( 0.000000000000000000, 0.000000000000000000, -1.000000000000000000 ) ) ;
#35549 = DIRECTION ( 'NONE',  ( 0.000000000000000000, 0.000000000000000000, 1.000000000000000000 ) ) ;
#35550 = DIRECTION ( 'NONE',  ( 0.000000000000000000, 0.000000000000000000, -1.000000000000000000 ) ) ;
#35551 = DIRECTION ( 'NONE',  ( -4.274815082592931898E-19, -0.9999939076577903929, -0.003490651415223739937 ) ) ;
#35552 = EDGE_LOOP ( 'NONE', ( #111031, #127674 ) ) ;
#35554 = CONICAL_SURFACE ( 'NONE', #95895, 0.09999999999999982514, 0.003490658503988666988 ) ;
#35553 = CIRCLE ( 'NONE', #50220, 0.09999999999999982514 ) ;
#35555 = LINE ( 'NONE', #75456, #121251 ) ;
#35556 = DIRECTION ( 'NONE',  ( 0.000000000000000000, 0.000000000000000000, 1.000000000000000000 ) ) ;
#35557 = ORIENTED_EDGE ( 'NONE', *, *, #19214, .T. ) ;
#35558 = CARTESIAN_POINT ( 'NONE',  ( -11.24999999999996447, 2.500000000000000000, -2.065063509461098068 ) ) ;
#35559 = CARTESIAN_POINT ( 'NONE',  ( 7.099999999999926814, 2.500000000000000000, -0.5928203230275541635 ) ) ;
#35560 = CARTESIAN_POINT ( 'NONE',  ( 3.949999999999942446, 2.500000000000000000, -2.611473670974877592 ) ) ;
#35561 = EDGE_LOOP ( 'NONE', ( #47138, #34527, #40650, #100260, #53877, #98163, #120185, #97684, #124096, #66708, #94191, #92556, #10611, #36738, #126128 ) ) ;
#35562 = DIRECTION ( 'NONE',  ( 0.000000000000000000, 0.000000000000000000, 1.000000000000000000 ) ) ;
#35563 = EDGE_CURVE ( 'NONE', #33973, #129536, #103026, .T. ) ;
#35564 = VERTEX_POINT ( 'NONE', #23175 ) ;
#35565 = CARTESIAN_POINT ( 'NONE',  ( -1.450000000000035039, 12.50000000000000000, -2.511473670974877948 ) ) ;
#35566 = LINE ( 'NONE', #76126, #11134 ) ;
#35567 = EDGE_LOOP ( 'NONE', ( #119908, #123918 ) ) ;
#35568 = AXIS2_PLACEMENT_3D ( 'NONE', #16298, #56237, #67988 ) ;
#35569 = CARTESIAN_POINT ( 'NONE',  ( 4.349999999999938360, 2.500000000000000000, 1.718653347947321386 ) ) ;
#35570 = CONICAL_SURFACE ( 'NONE', #16751, 0.09999999999999982514, 0.003490658503988666988 ) ;
#35571 = EDGE_CURVE ( 'NONE', #9027, #82955, #65337, .T. ) ;
#35572 = CARTESIAN_POINT ( 'NONE',  ( 12.49999999999990585, 2.500000000000000000, 3.637306695894644726 ) ) ;
#35573 = EDGE_CURVE ( 'NONE', #108669, #71566, #4786, .T. ) ;
#35574 = EDGE_LOOP ( 'NONE', ( #90453, #18028 ) ) ;
#35575 = AXIS2_PLACEMENT_3D ( 'NONE', #38464, #117615, #79029 ) ;
#35576 = CARTESIAN_POINT ( 'NONE',  ( -8.100000000000010303, 12.50000000000000000, 4.676537180435972552 ) ) ;
#35577 = EDGE_CURVE ( 'NONE', #67278, #29034, #94684, .T. ) ;
#35578 = ORIENTED_EDGE ( 'NONE', *, *, #91048, .T. ) ;
#35579 = EDGE_CURVE ( 'NONE', #99488, #85816, #111394, .T. ) ;
#35580 = ORIENTED_EDGE ( 'NONE', *, *, #39365, .T. ) ;
#35581 = PLANE ( 'NONE',  #46397 ) ;
#35582 = CARTESIAN_POINT ( 'NONE',  ( -11.24999999999999822, 2.500000000000000000, 1.472243186433545459 ) ) ;
#35583 = VERTEX_POINT ( 'NONE', #1600 ) ;
#35584 = CIRCLE ( 'NONE', #79499, 0.1000000000000002554 ) ;
#35585 = CARTESIAN_POINT ( 'NONE',  ( 2.949999999999946887, 12.50000000000000000, -2.165063509461101710 ) ) ;
#35586 = DIRECTION ( 'NONE',  ( -4.274815082592931898E-19, -0.9999939076577903929, -0.003490651415223739937 ) ) ;
#35587 = ORIENTED_EDGE ( 'NONE', *, *, #87568, .F. ) ;
#35588 = ADVANCED_FACE ( 'NONE', ( #52637 ), #109261, .T. ) ;
#35590 = DIRECTION ( 'NONE',  ( 0.000000000000000000, 1.000000000000000000, 0.000000000000000000 ) ) ;
#35589 = VECTOR ( 'NONE', #97025, 1000.000000000000000 ) ;
#35591 = DIRECTION ( 'NONE',  ( 0.000000000000000000, 0.000000000000000000, 1.000000000000000000 ) ) ;
#35592 = CONICAL_SURFACE ( 'NONE', #16676, 0.09999999999999982514, 0.003490658503988666988 ) ;
#35593 = CARTESIAN_POINT ( 'NONE',  ( 2.499999999999947153, 2.500000000000000000, 0.5928203230275495006 ) ) ;
#35594 = CARTESIAN_POINT ( 'NONE',  ( 3.349999999999944578, 2.500000000000000000, -1.572243186433550211 ) ) ;
#35595 = DIRECTION ( 'NONE',  ( -0.000000000000000000, -1.000000000000000000, -0.000000000000000000 ) ) ;
#35596 = CARTESIAN_POINT ( 'NONE',  ( -4.600000000000024514, 12.50000000000000000, -0.7579135962115917113 ) ) ;
#35597 = VECTOR ( 'NONE', #49741, 1000.000000000000000 ) ;
#35598 = ORIENTED_EDGE ( 'NONE', *, *, #116245, .T. ) ;
#35599 = ORIENTED_EDGE ( 'NONE', *, *, #83348, .T. ) ;
#35600 = ORIENTED_EDGE ( 'NONE', *, *, #58314, .F. ) ;
#35601 = VERTEX_POINT ( 'NONE', #111566 ) ;
#35602 = AXIS2_PLACEMENT_3D ( 'NONE', #115895, #64219, #103510 ) ;
#35603 = PLANE ( 'NONE',  #55786 ) ;
#35604 = DIRECTION ( 'NONE',  ( 0.000000000000000000, 0.000000000000000000, 1.000000000000000000 ) ) ;
#35605 = CARTESIAN_POINT ( 'NONE',  ( 10.59999999999991260, 12.50000000000000000, 0.3464101615137735735 ) ) ;
#35606 = ORIENTED_EDGE ( 'NONE', *, *, #16753, .T. ) ;
#35607 = FACE_BOUND ( 'NONE', #45316, .T. ) ;
#35608 = ADVANCED_FACE ( 'NONE', ( #12070 ), #2737, .T. ) ;
#35609 = CARTESIAN_POINT ( 'NONE',  ( -1.250000000000001110, 2.500000000000000000, -2.065063509461102065 ) ) ;
#35610 = LINE ( 'NONE', #66969, #89811 ) ;
#35611 = DIRECTION ( 'NONE',  ( 0.000000000000000000, 0.000000000000000000, -1.000000000000000000 ) ) ;
#35612 = CARTESIAN_POINT ( 'NONE',  ( -3.470457856696441969E-14, 12.50000000000000000, -0.7579135962115893799 ) ) ;
#35613 = PLANE ( 'NONE',  #80632 ) ;
#35614 = DIRECTION ( 'NONE',  ( -4.274815082592931898E-19, -0.9999939076577903929, -0.003490651415223739937 ) ) ;
#35615 = FACE_OUTER_BOUND ( 'NONE', #122255, .T. ) ;
#35616 = CARTESIAN_POINT ( 'NONE',  ( 12.69999999999990159, 12.50000000000000000, -3.983716857408426293 ) ) ;
#35617 = DIRECTION ( 'NONE',  ( 0.000000000000000000, 1.000000000000000000, 0.000000000000000000 ) ) ;
#35618 = CARTESIAN_POINT ( 'NONE',  ( 0.8499999999999553468, 12.50000000000000000, -2.792790559304616504 ) ) ;
#35619 = EDGE_LOOP ( 'NONE', ( #60085, #90611, #96906, #52151 ) ) ;
#35620 = ORIENTED_EDGE ( 'NONE', *, *, #107356, .T. ) ;
#35621 = EDGE_CURVE ( 'NONE', #118275, #79663, #8997, .T. ) ;
#35622 = ORIENTED_EDGE ( 'NONE', *, *, #23441, .T. ) ;
#35623 = EDGE_LOOP ( 'NONE', ( #64684, #120445 ) ) ;
#35624 = DIRECTION ( 'NONE',  ( 0.000000000000000000, 1.000000000000000000, 0.000000000000000000 ) ) ;
#35625 = ORIENTED_EDGE ( 'NONE', *, *, #113727, .F. ) ;
#35626 = AXIS2_PLACEMENT_3D ( 'NONE', #70419, #62544, #110341 ) ;
#35627 = DIRECTION ( 'NONE',  ( 0.000000000000000000, 0.000000000000000000, 1.000000000000000000 ) ) ;
#35628 = CONICAL_SURFACE ( 'NONE', #106702, 0.09999999999999982514, 0.003490658503988666988 ) ;
#35629 = EDGE_LOOP ( 'NONE', ( #24244, #75009 ) ) ;
#35630 = ORIENTED_EDGE ( 'NONE', *, *, #27680, .T. ) ;
#35631 = DIRECTION ( 'NONE',  ( -0.000000000000000000, 1.000000000000000000, -0.000000000000000000 ) ) ;
#35633 = AXIS2_PLACEMENT_3D ( 'NONE', #123942, #34305, #82763 ) ;
#35632 = AXIS2_PLACEMENT_3D ( 'NONE', #119390, #31672, #70951 ) ;
#35634 = CARTESIAN_POINT ( 'NONE',  ( 12.69999999999990337, 2.500000000000000000, 4.083716857408420609 ) ) ;
#35635 = DIRECTION ( 'NONE',  ( 0.000000000000000000, -0.000000000000000000, 1.000000000000000000 ) ) ;
#35636 = CARTESIAN_POINT ( 'NONE',  ( -3.100000000000028955, 12.50000000000000000, 4.048810130592458201 ) ) ;
#35637 = LINE ( 'NONE', #16614, #45627 ) ;
#35638 = EDGE_CURVE ( 'NONE', #70042, #119203, #86366, .T. ) ;
#35639 = ORIENTED_EDGE ( 'NONE', *, *, #74408, .T. ) ;
#35640 = VERTEX_POINT ( 'NONE', #21913 ) ;
#35641 = EDGE_LOOP ( 'NONE', ( #27184, #99266, #44708, #95953 ) ) ;
#35643 = ORIENTED_EDGE ( 'NONE', *, *, #37293, .F. ) ;
#35642 = CARTESIAN_POINT ( 'NONE',  ( 2.699999999999944666, 12.50000000000000000, 4.611443907251934426 ) ) ;
#35644 = FACE_OUTER_BOUND ( 'NONE', #107158, .T. ) ;
#35645 = ORIENTED_EDGE ( 'NONE', *, *, #45383, .T. ) ;
#35646 = ORIENTED_EDGE ( 'NONE', *, *, #92781, .F. ) ;
#35647 = LINE ( 'NONE', #84738, #102815 ) ;
#35648 = DIRECTION ( 'NONE',  ( 0.000000000000000000, -0.9999939076577903929, 0.003490651415223739937 ) ) ;
#35649 = FACE_OUTER_BOUND ( 'NONE', #108948, .T. ) ;
#35650 = CARTESIAN_POINT ( 'NONE',  ( 187.4218750003414016, 0.000000000000000000, 7.564683531250000925 ) ) ;
#35651 = FACE_OUTER_BOUND ( 'NONE', #106784, .T. ) ;
#35652 = LINE ( 'NONE', #115467, #30929 ) ;
#35653 = ORIENTED_EDGE ( 'NONE', *, *, #93165, .F. ) ;
#35654 = CARTESIAN_POINT ( 'NONE',  ( 1.249999999999952482, 2.500000000000000000, -5.702370205355749455 ) ) ;
#35655 = AXIS2_PLACEMENT_3D ( 'NONE', #70765, #32151, #51775 ) ;
#35656 = CONICAL_SURFACE ( 'NONE', #56563, 0.1000000000000002554, 0.003490658503988666988 ) ;
#35657 = EDGE_LOOP ( 'NONE', ( #120539, #7041, #127706, #90872 ) ) ;
#35658 = CARTESIAN_POINT ( 'NONE',  ( -3.150000000000030109, 2.500000000000000000, 1.818653347947321475 ) ) ;
#35659 = EDGE_CURVE ( 'NONE', #15804, #21810, #70353, .T. ) ;
#35660 = EDGE_LOOP ( 'NONE', ( #67931, #15472, #92931, #40023 ) ) ;
#35661 = DIRECTION ( 'NONE',  ( 0.000000000000000000, 0.000000000000000000, 1.000000000000000000 ) ) ;
#35662 = CARTESIAN_POINT ( 'NONE',  ( -3.300000000000027800, 12.50000000000000000, -4.330127018922201643 ) ) ;
#35663 = ORIENTED_EDGE ( 'NONE', *, *, #7743, .T. ) ;
#35664 = DIRECTION ( 'NONE',  ( -0.000000000000000000, 1.000000000000000000, -0.000000000000000000 ) ) ;
#35665 = DIRECTION ( 'NONE',  ( 0.000000000000000000, 1.000000000000000000, 0.000000000000000000 ) ) ;
#35666 = ORIENTED_EDGE ( 'NONE', *, *, #59804, .F. ) ;
#35667 = AXIS2_PLACEMENT_3D ( 'NONE', #79653, #11551, #121494 ) ;
#35668 = EDGE_CURVE ( 'NONE', #92847, #47032, #63395, .T. ) ;
#35669 = DIRECTION ( 'NONE',  ( 0.000000000000000000, 0.000000000000000000, 1.000000000000000000 ) ) ;
#35670 = CARTESIAN_POINT ( 'NONE',  ( -11.44999999999999751, 2.500000000000000000, -2.511473670974873951 ) ) ;
#35671 = ORIENTED_EDGE ( 'NONE', *, *, #16173, .F. ) ;
#35672 = EDGE_CURVE ( 'NONE', #10174, #96773, #33028, .T. ) ;
#35674 = VERTEX_POINT ( 'NONE', #92571 ) ;
#35673 = EDGE_CURVE ( 'NONE', #34505, #39201, #110276, .T. ) ;
#35675 = DIRECTION ( 'NONE',  ( -0.000000000000000000, -1.000000000000000000, -0.000000000000000000 ) ) ;
#35676 = DIRECTION ( 'NONE',  ( -0.000000000000000000, 1.000000000000000000, -0.000000000000000000 ) ) ;
#35677 = ADVANCED_FACE ( 'NONE', ( #112216 ), #119825, .T. ) ;
#35678 = CARTESIAN_POINT ( 'NONE',  ( 187.3802083336747444, 4.367472073101515306, 7.564683531250000925 ) ) ;
#35679 = EDGE_CURVE ( 'NONE', #5496, #63429, #117746, .T. ) ;
#35680 = DIRECTION ( 'NONE',  ( 0.000000000000000000, 0.000000000000000000, -1.000000000000000000 ) ) ;
#35681 = CIRCLE ( 'NONE', #98347, 0.1000000000000002554 ) ;
#35682 = CIRCLE ( 'NONE', #29333, 0.1000000000000002554 ) ;
#35683 = CARTESIAN_POINT ( 'NONE',  ( -6.650000000000018119, 2.500000000000000000, -6.495190528383302464 ) ) ;
#35684 = CARTESIAN_POINT ( 'NONE',  ( -11.24999999999999822, 2.500000000000000000, 5.802370205355744659 ) ) ;
#35685 = EDGE_CURVE ( 'NONE', #123334, #113423, #121875, .T. ) ;
#35686 = EDGE_CURVE ( 'NONE', #96252, #85559, #52930, .T. ) ;
#35687 = EDGE_CURVE ( 'NONE', #115043, #43214, #46670, .T. ) ;
#35688 = CONICAL_SURFACE ( 'NONE', #79597, 0.1000000000000002554, 0.003490658503988666988 ) ;
#35689 = VERTEX_POINT ( 'NONE', #55232 ) ;
#35690 = EDGE_CURVE ( 'NONE', #97645, #72180, #4880, .T. ) ;
#35691 = LINE ( 'NONE', #76261, #38092 ) ;
#35692 = ADVANCED_FACE ( 'NONE', ( #84679 ), #69649, .T. ) ;
#35693 = EDGE_LOOP ( 'NONE', ( #102139, #22596 ) ) ;
#35694 = AXIS2_PLACEMENT_3D ( 'NONE', #86104, #102695, #75023 ) ;
#35695 = FACE_OUTER_BOUND ( 'NONE', #30823, .T. ) ;
#35696 = FACE_OUTER_BOUND ( 'NONE', #21119, .T. ) ;
#35697 = CARTESIAN_POINT ( 'NONE',  ( -0.4000000000000331624, 2.500000000000000000, -0.1000000000000000056 ) ) ;
#35698 = EDGE_CURVE ( 'NONE', #4176, #104225, #16562, .T. ) ;
#35699 = EDGE_LOOP ( 'NONE', ( #47894, #118634, #118772, #14697 ) ) ;
#35700 = CARTESIAN_POINT ( 'NONE',  ( -10.85000000000000142, 12.50000000000000000, -6.430097255199260786 ) ) ;
#35701 = CARTESIAN_POINT ( 'NONE',  ( -8.350000000000013856, 2.500000000000000000, 2.065063509461097624 ) ) ;
#35702 = VERTEX_POINT ( 'NONE', #125253 ) ;
#35703 = DIRECTION ( 'NONE',  ( -0.000000000000000000, -1.000000000000000000, -0.000000000000000000 ) ) ;
#35704 = ORIENTED_EDGE ( 'NONE', *, *, #13465, .F. ) ;
#35705 = ORIENTED_EDGE ( 'NONE', *, *, #37731, .F. ) ;
#35706 = DIRECTION ( 'NONE',  ( 0.000000000000000000, 1.000000000000000000, 0.000000000000000000 ) ) ;
#35707 = AXIS2_PLACEMENT_3D ( 'NONE', #13739, #44502, #101502 ) ;
#35708 = AXIS2_PLACEMENT_3D ( 'NONE', #77511, #38249, #19220 ) ;
#35709 = VECTOR ( 'NONE', #60615, 1000.000000000000000 ) ;
#35710 = EDGE_LOOP ( 'NONE', ( #20418, #83617 ) ) ;
#35711 = CARTESIAN_POINT ( 'NONE',  ( 6.899999999999926636, 12.50000000000000000, 0.3464101615137736845 ) ) ;
#35712 = CARTESIAN_POINT ( 'NONE',  ( -8.350000000000013856, 2.500000000000000000, -5.802370205355744659 ) ) ;
#35713 = CARTESIAN_POINT ( 'NONE',  ( -6.250000000000019540, 2.500000000000000000, -7.188010851410854052 ) ) ;
#35714 = ORIENTED_EDGE ( 'NONE', *, *, #6378, .F. ) ;
#35715 = FACE_BOUND ( 'NONE', #83113, .T. ) ;
#35717 = ORIENTED_EDGE ( 'NONE', *, *, #88568, .T. ) ;
#35716 = DIRECTION ( 'NONE',  ( -0.000000000000000000, 1.000000000000000000, -0.000000000000000000 ) ) ;
#35718 = CIRCLE ( 'NONE', #102610, 0.06509327318403745899 ) ;
#35719 = DIRECTION ( 'NONE',  ( 0.000000000000000000, 1.000000000000000000, 0.000000000000000000 ) ) ;
#35720 = DIRECTION ( 'NONE',  ( -0.000000000000000000, -1.000000000000000000, -0.000000000000000000 ) ) ;
#35721 = EDGE_LOOP ( 'NONE', ( #47780, #5901, #33395, #20332 ) ) ;
#35722 = EDGE_CURVE ( 'NONE', #112193, #62955, #11149, .T. ) ;
#35723 = ORIENTED_EDGE ( 'NONE', *, *, #72061, .F. ) ;
#35724 = ADVANCED_FACE ( 'NONE', ( #6103 ), #95791, .T. ) ;
#35725 = ORIENTED_EDGE ( 'NONE', *, *, #85265, .F. ) ;
#35726 = PLANE ( 'NONE',  #25277 ) ;
#35727 = FACE_OUTER_BOUND ( 'NONE', #100975, .T. ) ;
#35728 = DIRECTION ( 'NONE',  ( 0.000000000000000000, 1.000000000000000000, 0.000000000000000000 ) ) ;
#35729 = FACE_BOUND ( 'NONE', #55784, .T. ) ;
#35730 = VERTEX_POINT ( 'NONE', #54559 ) ;
#35731 = CARTESIAN_POINT ( 'NONE',  ( 184.7343750003414016, 8.734944146203032389, 5.348610694689227483E-16 ) ) ;
#35732 = EDGE_CURVE ( 'NONE', #98489, #79642, #6729, .T. ) ;
#35733 = DIRECTION ( 'NONE',  ( 0.000000000000000000, 1.000000000000000000, 0.000000000000000000 ) ) ;
#35734 = CARTESIAN_POINT ( 'NONE',  ( 7.049999999999928768, 2.500000000000000000, 6.595190528383296780 ) ) ;
#35735 = EDGE_CURVE ( 'NONE', #31758, #15286, #75906, .T. ) ;
#35736 = AXIS2_PLACEMENT_3D ( 'NONE', #15635, #4511, #123041 ) ;
#35738 = EDGE_CURVE ( 'NONE', #781, #63941, #36240, .T. ) ;
#35737 = DIRECTION ( 'NONE',  ( 0.000000000000000000, -0.9999939076577903929, 0.003490651415223739937 ) ) ;
#35739 = CARTESIAN_POINT ( 'NONE',  ( -0.4000000000000339950, 2.500000000000000000, 0.6928203230275518099 ) ) ;
#35740 = LINE ( 'NONE', #95305, #71917 ) ;
#35741 = CARTESIAN_POINT ( 'NONE',  ( 4.149999999999938183, 2.500000000000000000, 7.088010851410848190 ) ) ;
#35742 = CARTESIAN_POINT ( 'NONE',  ( 10.44999999999991402, 2.500000000000000000, -2.165063509461101710 ) ) ;
#35743 = CIRCLE ( 'NONE', #108883, 0.06509327318403745899 ) ;
#35744 = CIRCLE ( 'NONE', #50401, 0.1000000000000000472 ) ;
#35745 = DIRECTION ( 'NONE',  ( 0.000000000000000000, 0.000000000000000000, 1.000000000000000000 ) ) ;
#35746 = ORIENTED_EDGE ( 'NONE', *, *, #9099, .T. ) ;
#35747 = ORIENTED_EDGE ( 'NONE', *, *, #80782, .T. ) ;
#35748 = ORIENTED_EDGE ( 'NONE', *, *, #74097, .T. ) ;
#35749 = ORIENTED_EDGE ( 'NONE', *, *, #72716, .F. ) ;
#35750 = ORIENTED_EDGE ( 'NONE', *, *, #40994, .F. ) ;
#35751 = CARTESIAN_POINT ( 'NONE',  ( 184.5000000000000000, 0.000000000000000000, 0.000000000000000000 ) ) ;
#35752 = DIRECTION ( 'NONE',  ( 0.000000000000000000, 1.000000000000000000, 0.000000000000000000 ) ) ;
#35753 = ORIENTED_EDGE ( 'NONE', *, *, #53265, .F. ) ;
#35754 = FACE_BOUND ( 'NONE', #53126, .T. ) ;
#35755 = CIRCLE ( 'NONE', #62935, 0.1000000000000000472 ) ;
#35756 = DIRECTION ( 'NONE',  ( 0.000000000000000000, 1.000000000000000000, 0.000000000000000000 ) ) ;
#35757 = CIRCLE ( 'NONE', #96372, 0.1000000000000002554 ) ;
#35758 = DIRECTION ( 'NONE',  ( 0.000000000000000000, 0.000000000000000000, 1.000000000000000000 ) ) ;
#35759 = ORIENTED_EDGE ( 'NONE', *, *, #111623, .F. ) ;
#35760 = LINE ( 'NONE', #106426, #5610 ) ;
#35761 = FACE_OUTER_BOUND ( 'NONE', #56875, .T. ) ;
#35762 = CARTESIAN_POINT ( 'NONE',  ( -15.19999999999998330, 2.500000000000000000, 0.4464101615137758272 ) ) ;
#35763 = ORIENTED_EDGE ( 'NONE', *, *, #60515, .T. ) ;
#35764 = LINE ( 'NONE', #35139, #57713 ) ;
#35766 = EDGE_CURVE ( 'NONE', #50259, #74009, #61339, .T. ) ;
#35765 = VECTOR ( 'NONE', #78544, 1000.000000000000000 ) ;
#35767 = ORIENTED_EDGE ( 'NONE', *, *, #26864, .T. ) ;
#35768 = AXIS2_PLACEMENT_3D ( 'NONE', #120250, #82259, #12832 ) ;
#35769 = ORIENTED_EDGE ( 'NONE', *, *, #121234, .F. ) ;
#35770 = ORIENTED_EDGE ( 'NONE', *, *, #119416, .F. ) ;
#35771 = CARTESIAN_POINT ( 'NONE',  ( 1.849999999999949685, 2.500000000000000000, -2.611473670974877592 ) ) ;
#35772 = DIRECTION ( 'NONE',  ( -0.000000000000000000, -1.000000000000000000, -0.000000000000000000 ) ) ;
#35773 = DIRECTION ( 'NONE',  ( -0.000000000000000000, -1.000000000000000000, -0.000000000000000000 ) ) ;
#35774 = ORIENTED_EDGE ( 'NONE', *, *, #90865, .T. ) ;
#35775 = CARTESIAN_POINT ( 'NONE',  ( 15.23091471310319278, 2.499999999999935163, -7.179421168902959671 ) ) ;
#35776 = VECTOR ( 'NONE', #106393, 1000.000000000000000 ) ;
#35777 = DIRECTION ( 'NONE',  ( 0.000000000000000000, 0.000000000000000000, -1.000000000000000000 ) ) ;
#35778 = DIRECTION ( 'NONE',  ( 0.000000000000000000, 1.000000000000000000, 0.000000000000000000 ) ) ;
#35779 = AXIS2_PLACEMENT_3D ( 'NONE', #13357, #2913, #53307 ) ;
#35780 = AXIS2_PLACEMENT_3D ( 'NONE', #64620, #23399, #73792 ) ;
#35781 = CARTESIAN_POINT ( 'NONE',  ( 183.7812500006828031, 0.000000000000000000, 7.700000000000000178 ) ) ;
#35782 = CARTESIAN_POINT ( 'NONE',  ( 1.649999999999951505, 2.500000000000000000, 1.572243186433545548 ) ) ;
#35783 = ADVANCED_FACE ( 'NONE', ( #93860 ), #25728, .T. ) ;
#35784 = CARTESIAN_POINT ( 'NONE',  ( 2.499999999999947153, 2.500000000000000000, 3.637306695894644726 ) ) ;
#35785 = EDGE_CURVE ( 'NONE', #47693, #75963, #98891, .T. ) ;
#35786 = ORIENTED_EDGE ( 'NONE', *, *, #86285, .F. ) ;
#35787 = DIRECTION ( 'NONE',  ( 0.000000000000000000, 0.000000000000000000, -1.000000000000000000 ) ) ;
#35788 = ORIENTED_EDGE ( 'NONE', *, *, #26506, .T. ) ;
#35789 = ORIENTED_EDGE ( 'NONE', *, *, #10663, .T. ) ;
#35790 = DIRECTION ( 'NONE',  ( 0.000000000000000000, -0.000000000000000000, 1.000000000000000000 ) ) ;
#35791 = DIRECTION ( 'NONE',  ( 0.000000000000000000, 1.000000000000000000, 0.000000000000000000 ) ) ;
#35793 = ADVANCED_FACE ( 'NONE', ( #124613 ), #90573, .T. ) ;
#35792 = DIRECTION ( 'NONE',  ( -0.000000000000000000, 1.000000000000000000, -0.000000000000000000 ) ) ;
#35794 = ORIENTED_EDGE ( 'NONE', *, *, #6090, .T. ) ;
#35795 = ORIENTED_EDGE ( 'NONE', *, *, #58208, .T. ) ;
#35796 = DIRECTION ( 'NONE',  ( -0.000000000000000000, 1.000000000000000000, -0.000000000000000000 ) ) ;
#35797 = CARTESIAN_POINT ( 'NONE',  ( 81.97074731400692826, 3.937872643741660017, -6.123955218199263584 ) ) ;
#35799 = DIRECTION ( 'NONE',  ( -0.000000000000000000, -1.000000000000000000, -0.000000000000000000 ) ) ;
#35798 = CIRCLE ( 'NONE', #33741, 0.1000000000000002554 ) ;
#35800 = ORIENTED_EDGE ( 'NONE', *, *, #60264, .T. ) ;
#35801 = ORIENTED_EDGE ( 'NONE', *, *, #73114, .T. ) ;
#35802 = AXIS2_PLACEMENT_3D ( 'NONE', #43747, #41324, #89755 ) ;
#35803 = CIRCLE ( 'NONE', #273, 0.1000000000000002554 ) ;
#35804 = FACE_OUTER_BOUND ( 'NONE', #94569, .T. ) ;
#35805 = ORIENTED_EDGE ( 'NONE', *, *, #103403, .T. ) ;
#35806 = DIRECTION ( 'NONE',  ( 0.000000000000000000, 0.000000000000000000, -1.000000000000000000 ) ) ;
#35807 = AXIS2_PLACEMENT_3D ( 'NONE', #86398, #116508, #10427 ) ;
#35808 = DIRECTION ( 'NONE',  ( 0.000000000000000000, -0.000000000000000000, 1.000000000000000000 ) ) ;
#35809 = ORIENTED_EDGE ( 'NONE', *, *, #51214, .T. ) ;
#35810 = DIRECTION ( 'NONE',  ( -0.000000000000000000, -1.000000000000000000, -0.000000000000000000 ) ) ;
#35811 = CARTESIAN_POINT ( 'NONE',  ( 10.84999999999990905, 12.50000000000000000, 1.407149913249508000 ) ) ;
#35812 = DIRECTION ( 'NONE',  ( -0.000000000000000000, 1.000000000000000000, -0.000000000000000000 ) ) ;
#35813 = AXIS2_PLACEMENT_3D ( 'NONE', #124670, #55913, #64445 ) ;
#35814 = LINE ( 'NONE', #87474, #66762 ) ;
#35815 = EDGE_LOOP ( 'NONE', ( #68420, #102635, #38689, #1276 ) ) ;
#35816 = EDGE_CURVE ( 'NONE', #89205, #7349, #115604, .T. ) ;
#35817 = FACE_OUTER_BOUND ( 'NONE', #124927, .T. ) ;
#35818 = LINE ( 'NONE', #75730, #10226 ) ;
#35819 = EDGE_LOOP ( 'NONE', ( #6361, #86541 ) ) ;
#35820 = EDGE_LOOP ( 'NONE', ( #12727, #76975 ) ) ;
#35821 = ADVANCED_FACE ( 'NONE', ( #15923 ), #53938, .T. ) ;
#35822 = EDGE_CURVE ( 'NONE', #98931, #22721, #107300, .T. ) ;
#35823 = CARTESIAN_POINT ( 'NONE',  ( 184.3802083336747444, 4.367472073101515306, 7.564683531250000925 ) ) ;
#35824 = FACE_OUTER_BOUND ( 'NONE', #24729, .T. ) ;
#35825 = CARTESIAN_POINT ( 'NONE',  ( -12.49999999999995914, 12.50000000000000000, -4.330127018922198978 ) ) ;
#35826 = EDGE_CURVE ( 'NONE', #127250, #107780, #115395, .T. ) ;
#35827 = DIRECTION ( 'NONE',  ( 0.000000000000000000, 0.000000000000000000, 1.000000000000000000 ) ) ;
#35828 = EDGE_CURVE ( 'NONE', #74205, #65138, #44609, .T. ) ;
#35829 = CARTESIAN_POINT ( 'NONE',  ( -6.900000000000019007, 12.50000000000000000, 0.3464101615137735735 ) ) ;
#35830 = CARTESIAN_POINT ( 'NONE',  ( 3.149999999999944400, 2.500000000000000000, 2.511473670974873507 ) ) ;
#35831 = DIRECTION ( 'NONE',  ( -1.000000000000000000, -0.000000000000000000, -0.000000000000000000 ) ) ;
#35832 = CARTESIAN_POINT ( 'NONE',  ( -4.150000000000025224, 12.50000000000000000, 7.188010851410848723 ) ) ;
#35833 = DIRECTION ( 'NONE',  ( 0.000000000000000000, 0.000000000000000000, 1.000000000000000000 ) ) ;
#35834 = EDGE_CURVE ( 'NONE', #123777, #62546, #65678, .T. ) ;
#35835 = ADVANCED_FACE ( 'NONE', ( #129149 ), #71805, .T. ) ;
#35836 = CARTESIAN_POINT ( 'NONE',  ( -7.900000000000011013, 12.50000000000000000, 3.637306695894644726 ) ) ;
#35837 = CONICAL_SURFACE ( 'NONE', #12818, 0.1000000000000002554, 0.003490658503988666988 ) ;
#35838 = VERTEX_POINT ( 'NONE', #59760 ) ;
#35839 = AXIS2_PLACEMENT_3D ( 'NONE', #121952, #93142, #43411 ) ;
#35840 = EDGE_CURVE ( 'NONE', #46113, #23974, #116709, .T. ) ;
#35841 = ORIENTED_EDGE ( 'NONE', *, *, #77357, .F. ) ;
#35842 = ORIENTED_EDGE ( 'NONE', *, *, #28433, .T. ) ;
#35843 = EDGE_CURVE ( 'NONE', #89842, #27226, #126548, .T. ) ;
#35844 = CARTESIAN_POINT ( 'NONE',  ( 5.649999999999932854, 12.50000000000000000, 2.446380397790835826 ) ) ;
#35845 = DIRECTION ( 'NONE',  ( 0.000000000000000000, 0.000000000000000000, -1.000000000000000000 ) ) ;
#35846 = DIRECTION ( 'NONE',  ( 0.000000000000000000, 0.000000000000000000, -1.000000000000000000 ) ) ;
#35848 = EDGE_CURVE ( 'NONE', #122177, #81286, #128253, .T. ) ;
#35847 = CIRCLE ( 'NONE', #117379, 0.1000000000000000472 ) ;
#35849 = CIRCLE ( 'NONE', #6554, 0.09999999999999982514 ) ;
#35850 = ORIENTED_EDGE ( 'NONE', *, *, #98379, .F. ) ;
#35851 = LINE ( 'NONE', #6352, #123994 ) ;
#35852 = CARTESIAN_POINT ( 'NONE',  ( -4.800000000000024691, 2.500000000000000000, 4.576537180435972019 ) ) ;
#35854 = ORIENTED_EDGE ( 'NONE', *, *, #17031, .T. ) ;
#35853 = CARTESIAN_POINT ( 'NONE',  ( 1.699999999999951994, 2.500000000000000000, -4.230127018922201998 ) ) ;
#35855 = FACE_OUTER_BOUND ( 'NONE', #52202, .T. ) ;
#35856 = CIRCLE ( 'NONE', #90121, 0.1000000000000002554 ) ;
#35857 = ORIENTED_EDGE ( 'NONE', *, *, #84329, .T. ) ;
#35858 = DIRECTION ( 'NONE',  ( 0.000000000000000000, 0.000000000000000000, -1.000000000000000000 ) ) ;
#35859 = AXIS2_PLACEMENT_3D ( 'NONE', #78241, #18006, #117467 ) ;
#35860 = ORIENTED_EDGE ( 'NONE', *, *, #13667, .F. ) ;
#35861 = VERTEX_POINT ( 'NONE', #109481 ) ;
#35863 = ORIENTED_EDGE ( 'NONE', *, *, #29892, .T. ) ;
#35862 = CONICAL_SURFACE ( 'NONE', #79776, 0.1000000000000000056, 0.003490658503988666988 ) ;
#35864 = CARTESIAN_POINT ( 'NONE',  ( 3.549999999999940314, 2.500000000000000000, 6.841600689897072485 ) ) ;
#35865 = AXIS2_PLACEMENT_3D ( 'NONE', #13336, #10743, #112850 ) ;
#35866 = PLANE ( 'NONE',  #44608 ) ;
#35867 = DIRECTION ( 'NONE',  ( -0.000000000000000000, -0.000000000000000000, -1.000000000000000000 ) ) ;
#35868 = CARTESIAN_POINT ( 'NONE',  ( -5.850000000000018296, 2.500000000000000000, 5.802370205355744659 ) ) ;
#35869 = ORIENTED_EDGE ( 'NONE', *, *, #45605, .T. ) ;
#35870 = AXIS2_PLACEMENT_3D ( 'NONE', #34318, #74224, #15925 ) ;
#35871 = AXIS2_PLACEMENT_3D ( 'NONE', #73633, #4886, #62553 ) ;
#35872 = DIRECTION ( 'NONE',  ( 0.000000000000000000, 0.000000000000000000, 1.000000000000000000 ) ) ;
#35873 = ORIENTED_EDGE ( 'NONE', *, *, #118587, .T. ) ;
#35874 = CARTESIAN_POINT ( 'NONE',  ( 76.40063402985219909, -3.742348971402477353, -5.987205606701297533 ) ) ;
#35875 = CARTESIAN_POINT ( 'NONE',  ( 13.92826132181480681, -2.499999999999999112, -6.790916467786979993 ) ) ;
#35876 = DIRECTION ( 'NONE',  ( -0.000000000000000000, 1.000000000000000000, -0.000000000000000000 ) ) ;
#35877 = CARTESIAN_POINT ( 'NONE',  ( 16.72050902517240800, -2.552201582239431943, 5.918448581780632267 ) ) ;
#35878 = ORIENTED_EDGE ( 'NONE', *, *, #26972, .F. ) ;
#35879 = ADVANCED_FACE ( 'NONE', ( #28997 ), #21723, .T. ) ;
#35880 = EDGE_LOOP ( 'NONE', ( #114337, #25593 ) ) ;
#35881 = EDGE_CURVE ( 'NONE', #103364, #4955, #128147, .T. ) ;
#35882 = ORIENTED_EDGE ( 'NONE', *, *, #4058, .T. ) ;
#35883 = CARTESIAN_POINT ( 'NONE',  ( -12.09999999999999432, 12.50000000000000000, 5.022947341949748790 ) ) ;
#35884 = DIRECTION ( 'NONE',  ( -0.000000000000000000, -1.000000000000000000, -0.000000000000000000 ) ) ;
#35885 = DIRECTION ( 'NONE',  ( 0.000000000000000000, 0.000000000000000000, 1.000000000000000000 ) ) ;
#35886 = FACE_BOUND ( 'NONE', #84810, .T. ) ;
#35887 = CARTESIAN_POINT ( 'NONE',  ( -4.600000000000025402, 2.500000000000000000, 4.330127018922196314 ) ) ;
#35888 = DIRECTION ( 'NONE',  ( -0.000000000000000000, 1.000000000000000000, -0.000000000000000000 ) ) ;
#35889 = CARTESIAN_POINT ( 'NONE',  ( -8.350000000000013856, 12.50000000000000000, 2.165063509461097713 ) ) ;
#35890 = CARTESIAN_POINT ( 'NONE',  ( -4.999999999999990230, 2.500000000000000000, -4.230127018922201998 ) ) ;
#35891 = AXIS2_PLACEMENT_3D ( 'NONE', #93524, #113157, #23487 ) ;
#35893 = AXIS2_PLACEMENT_3D ( 'NONE', #106793, #38745, #17099 ) ;
#35892 = CARTESIAN_POINT ( 'NONE',  ( 186.0468750003414300, -8.734944146203032389, -1.604583208406767949E-15 ) ) ;
#35894 = DIRECTION ( 'NONE',  ( -4.274815082592931898E-19, -0.9999939076577903929, -0.003490651415223739937 ) ) ;
#35895 = DIRECTION ( 'NONE',  ( 0.000000000000000000, -0.000000000000000000, 1.000000000000000000 ) ) ;
#35896 = AXIS2_PLACEMENT_3D ( 'NONE', #116353, #35876, #95442 ) ;
#35897 = CARTESIAN_POINT ( 'NONE',  ( 8.549999999999922551, 12.50000000000000000, 2.576566944158910744 ) ) ;
#35898 = CONICAL_SURFACE ( 'NONE', #19143, 0.1000000000000002554, 0.003490658503988666988 ) ;
#35899 = VERTEX_POINT ( 'NONE', #99669 ) ;
#35900 = ORIENTED_EDGE ( 'NONE', *, *, #45438, .T. ) ;
#35901 = ORIENTED_EDGE ( 'NONE', *, *, #96496, .F. ) ;
#35902 = ORIENTED_EDGE ( 'NONE', *, *, #20594, .F. ) ;
#35903 = CONICAL_SURFACE ( 'NONE', #29640, 0.09999999999999999167, 0.003490658503988666988 ) ;
#35904 = CARTESIAN_POINT ( 'NONE',  ( -8.750000000000012434, 2.500000000000000000, -5.902370205355745192 ) ) ;
#35905 = FACE_BOUND ( 'NONE', #58546, .T. ) ;
#35906 = DIRECTION ( 'NONE',  ( 0.000000000000000000, 0.000000000000000000, -1.000000000000000000 ) ) ;
#35907 = AXIS2_PLACEMENT_3D ( 'NONE', #78271, #19981, #86769 ) ;
#35908 = ORIENTED_EDGE ( 'NONE', *, *, #54603, .F. ) ;
#35909 = DIRECTION ( 'NONE',  ( -0.000000000000000000, -1.000000000000000000, -0.000000000000000000 ) ) ;
#35910 = DIRECTION ( 'NONE',  ( 0.000000000000000000, 0.000000000000000000, -1.000000000000000000 ) ) ;
#35911 = ORIENTED_EDGE ( 'NONE', *, *, #67128, .T. ) ;
#35912 = DIRECTION ( 'NONE',  ( 1.000000000000000000, -0.000000000000000000, -0.000000000000000000 ) ) ;
#35913 = CARTESIAN_POINT ( 'NONE',  ( 0.6499999999999566125, 2.500000000000000000, -6.148780366869526226 ) ) ;
#35914 = EDGE_CURVE ( 'NONE', #32951, #18013, #107390, .T. ) ;
#35915 = EDGE_LOOP ( 'NONE', ( #77421, #35144, #40405, #98151 ) ) ;
#35916 = DIRECTION ( 'NONE',  ( 0.000000000000000000, 1.000000000000000000, 0.000000000000000000 ) ) ;
#35917 = DIRECTION ( 'NONE',  ( -4.274815082592931898E-19, -0.9999939076577903929, -0.003490651415223739937 ) ) ;
#35918 = CONICAL_SURFACE ( 'NONE', #75714, 0.1000000000000000472, 0.003490658503988666988 ) ;
#35919 = EDGE_CURVE ( 'NONE', #124332, #59408, #9990, .T. ) ;
#35920 = CIRCLE ( 'NONE', #109056, 0.06509327318403745899 ) ;
#35921 = ORIENTED_EDGE ( 'NONE', *, *, #76206, .F. ) ;
#35922 = CARTESIAN_POINT ( 'NONE',  ( -7.700000000000016165, 2.500000000000000000, 0.2464101615137735679 ) ) ;
#35923 = FACE_OUTER_BOUND ( 'NONE', #52264, .T. ) ;
#35924 = VERTEX_POINT ( 'NONE', #7392 ) ;
#35925 = CARTESIAN_POINT ( 'NONE',  ( 10.19999999999991047, 2.500000000000000000, -4.083716857408426826 ) ) ;
#35926 = ORIENTED_EDGE ( 'NONE', *, *, #67383, .T. ) ;
#35927 = EDGE_CURVE ( 'NONE', #102542, #64648, #18516, .T. ) ;
#35928 = ORIENTED_EDGE ( 'NONE', *, *, #103554, .F. ) ;
#35929 = EDGE_CURVE ( 'NONE', #65247, #1730, #30048, .T. ) ;
#35930 = DIRECTION ( 'NONE',  ( -0.000000000000000000, -1.000000000000000000, -0.000000000000000000 ) ) ;
#35931 = AXIS2_PLACEMENT_3D ( 'NONE', #68544, #118940, #17502 ) ;
#35932 = ORIENTED_EDGE ( 'NONE', *, *, #1972, .F. ) ;
#35933 = FACE_OUTER_BOUND ( 'NONE', #86767, .T. ) ;
#35934 = VECTOR ( 'NONE', #15980, 1000.000000000000000 ) ;
#35935 = FACE_OUTER_BOUND ( 'NONE', #20849, .T. ) ;
#35936 = CIRCLE ( 'NONE', #52655, 0.1000000000000002554 ) ;
#35937 = ORIENTED_EDGE ( 'NONE', *, *, #103662, .F. ) ;
#35938 = AXIS2_PLACEMENT_3D ( 'NONE', #49964, #110148, #70229 ) ;
#35939 = CARTESIAN_POINT ( 'NONE',  ( -11.44999999999999929, 2.500000000000000000, -1.818653347947322141 ) ) ;
#35940 = CARTESIAN_POINT ( 'NONE',  ( -0.6500000000000389910, 2.500000000000000000, -6.048780366869526581 ) ) ;
#35941 = CARTESIAN_POINT ( 'NONE',  ( -8.350000000000010303, 12.50000000000000000, 6.495190528383297135 ) ) ;
#35942 = DIRECTION ( 'NONE',  ( 0.000000000000000000, 0.000000000000000000, 1.000000000000000000 ) ) ;
#35944 = ADVANCED_FACE ( 'NONE', ( #27055 ), #46769, .T. ) ;
#35943 = LINE ( 'NONE', #66680, #102975 ) ;
#35945 = CARTESIAN_POINT ( 'NONE',  ( -6.850000000000017408, 12.50000000000000000, -6.148780366869526226 ) ) ;
#35946 = CONICAL_SURFACE ( 'NONE', #100684, 0.1000000000000000472, 0.003490658503988666988 ) ;
#35947 = ORIENTED_EDGE ( 'NONE', *, *, #53835, .F. ) ;
#35948 = AXIS2_PLACEMENT_3D ( 'NONE', #101085, #11411, #90612 ) ;
#35949 = ORIENTED_EDGE ( 'NONE', *, *, #108929, .F. ) ;
#35950 = DIRECTION ( 'NONE',  ( -0.000000000000000000, -1.000000000000000000, -0.000000000000000000 ) ) ;
#35952 = CIRCLE ( 'NONE', #81904, 0.1000000000000002554 ) ;
#35951 = CARTESIAN_POINT ( 'NONE',  ( 16.70850060796086467, -0.4765610498145330665, 5.930927070179653704 ) ) ;
#35953 = CONICAL_SURFACE ( 'NONE', #58943, 0.1000000000000000472, 0.003490658503988666988 ) ;
#35954 = VECTOR ( 'NONE', #35146, 1000.000000000000000 ) ;
#35955 = DIRECTION ( 'NONE',  ( 0.000000000000000000, 0.000000000000000000, -1.000000000000000000 ) ) ;
#35957 = ORIENTED_EDGE ( 'NONE', *, *, #128872, .T. ) ;
#35956 = ORIENTED_EDGE ( 'NONE', *, *, #128508, .F. ) ;
#35958 = ORIENTED_EDGE ( 'NONE', *, *, #35261, .F. ) ;
#35959 = DIRECTION ( 'NONE',  ( 0.000000000000000000, -0.9999939076577903929, 0.003490651415223739937 ) ) ;
#35960 = AXIS2_PLACEMENT_3D ( 'NONE', #4155, #76630, #44097 ) ;
#35961 = DIRECTION ( 'NONE',  ( -0.000000000000000000, 1.000000000000000000, -0.000000000000000000 ) ) ;
#35962 = CARTESIAN_POINT ( 'NONE',  ( 10.59999999999990905, 2.500000000000000000, 4.576537180435972019 ) ) ;
#35963 = DIRECTION ( 'NONE',  ( 0.000000000000000000, 0.000000000000000000, 1.000000000000000000 ) ) ;
#35964 = CARTESIAN_POINT ( 'NONE',  ( 9.599999999999917932, 2.500000000000000000, 0.09999999999999772959 ) ) ;
#35965 = AXIS2_PLACEMENT_3D ( 'NONE', #123173, #61018, #91770 ) ;
#35966 = CARTESIAN_POINT ( 'NONE',  ( 11.24999999999991118, 2.500000000000000000, -2.957883832488653830 ) ) ;
#35967 = DIRECTION ( 'NONE',  ( 0.000000000000000000, 0.000000000000000000, 1.000000000000000000 ) ) ;
#35968 = CARTESIAN_POINT ( 'NONE',  ( -5.400000000000019895, 12.50000000000000000, -2.276824562219559311E-15 ) ) ;
#35969 = DIRECTION ( 'NONE',  ( -4.274815082592931898E-19, -0.9999939076577903929, -0.003490651415223739937 ) ) ;
#35970 = LINE ( 'NONE', #75244, #14344 ) ;
#35971 = ORIENTED_EDGE ( 'NONE', *, *, #112422, .F. ) ;
#35972 = ADVANCED_FACE ( 'NONE', ( #128502 ), #58461, .T. ) ;
#35973 = CARTESIAN_POINT ( 'NONE',  ( 9.199999999999919353, 2.500000000000000000, -0.1000000000000022815 ) ) ;
#35974 = ORIENTED_EDGE ( 'NONE', *, *, #1075, .T. ) ;
#35975 = ORIENTED_EDGE ( 'NONE', *, *, #116470, .T. ) ;
#35976 = EDGE_CURVE ( 'NONE', #34456, #62695, #8671, .T. ) ;
#35977 = DIRECTION ( 'NONE',  ( 0.000000000000000000, -0.000000000000000000, 1.000000000000000000 ) ) ;
#35978 = DIRECTION ( 'NONE',  ( 0.000000000000000000, 0.000000000000000000, 1.000000000000000000 ) ) ;
#35979 = DIRECTION ( 'NONE',  ( -0.000000000000000000, -1.000000000000000000, -0.000000000000000000 ) ) ;
#35980 = EDGE_CURVE ( 'NONE', #2098, #36092, #9344, .T. ) ;
#35981 = FACE_OUTER_BOUND ( 'NONE', #42247, .T. ) ;
#35982 = FACE_OUTER_BOUND ( 'NONE', #107537, .T. ) ;
#35983 = CARTESIAN_POINT ( 'NONE',  ( 9.799999999999918998, 2.500000000000000000, -0.4464101615137782142 ) ) ;
#35984 = CIRCLE ( 'NONE', #109116, 0.1000000000000000472 ) ;
#35985 = CARTESIAN_POINT ( 'NONE',  ( 2.499999999999948930, 2.500000000000000000, -0.5928203230275541635 ) ) ;
#35986 = ORIENTED_EDGE ( 'NONE', *, *, #3988, .F. ) ;
#35987 = CARTESIAN_POINT ( 'NONE',  ( 6.249999999999928946, 12.50000000000000000, 2.857883832488649301 ) ) ;
#35988 = AXIS2_PLACEMENT_3D ( 'NONE', #100890, #68861, #99626 ) ;
#35989 = EDGE_CURVE ( 'NONE', #41467, #115621, #13291, .T. ) ;
#35990 = AXIS2_PLACEMENT_3D ( 'NONE', #56412, #38072, #66873 ) ;
#35991 = EDGE_CURVE ( 'NONE', #49421, #89608, #63490, .T. ) ;
#35992 = ADVANCED_FACE ( 'NONE', ( #37530 ), #77438, .F. ) ;
#35993 = EDGE_CURVE ( 'NONE', #37339, #59274, #27676, .T. ) ;
#35994 = CARTESIAN_POINT ( 'NONE',  ( -0.2000000000000339284, 12.50000000000000000, -0.3464101615137759604 ) ) ;
#35995 = ORIENTED_EDGE ( 'NONE', *, *, #84446, .T. ) ;
#35996 = AXIS2_PLACEMENT_3D ( 'NONE', #83377, #25088, #63735 ) ;
#35997 = VERTEX_POINT ( 'NONE', #81935 ) ;
#35998 = VECTOR ( 'NONE', #104719, 1000.000000000000000 ) ;
#35999 = AXIS2_PLACEMENT_3D ( 'NONE', #19701, #59655, #49819 ) ;
#36000 = ADVANCED_FACE ( 'NONE', ( #21750 ), #30936, .T. ) ;
#36001 = ORIENTED_EDGE ( 'NONE', *, *, #28221, .T. ) ;
#36002 = AXIS2_PLACEMENT_3D ( 'NONE', #23208, #43526, #36918 ) ;
#36003 = CIRCLE ( 'NONE', #69437, 0.1000000000000002554 ) ;
#36004 = EDGE_LOOP ( 'NONE', ( #39355, #67929, #67795, #5921 ) ) ;
#36005 = FACE_OUTER_BOUND ( 'NONE', #89697, .T. ) ;
#36006 = FACE_OUTER_BOUND ( 'NONE', #58103, .T. ) ;
#36007 = EDGE_CURVE ( 'NONE', #61414, #88412, #50982, .T. ) ;
#36008 = AXIS2_PLACEMENT_3D ( 'NONE', #12313, #32641, #43101 ) ;
#36009 = DIRECTION ( 'NONE',  ( 0.000000000000000000, 0.000000000000000000, 1.000000000000000000 ) ) ;
#36010 = DIRECTION ( 'NONE',  ( 0.000000000000000000, 1.000000000000000000, 0.000000000000000000 ) ) ;
#36011 = CARTESIAN_POINT ( 'NONE',  ( 4.599999999999937472, 12.50000000000000000, 0.6277270498435120194 ) ) ;
#36012 = ORIENTED_EDGE ( 'NONE', *, *, #67794, .T. ) ;
#36013 = CARTESIAN_POINT ( 'NONE',  ( 3.749999999999978684, 12.50000000000000000, -2.230156782645139391 ) ) ;
#36014 = CARTESIAN_POINT ( 'NONE',  ( -4.999999999999986677, 2.500000000000000000, 4.330127018922196314 ) ) ;
#36015 = ORIENTED_EDGE ( 'NONE', *, *, #106305, .T. ) ;
#36016 = ORIENTED_EDGE ( 'NONE', *, *, #63426, .F. ) ;
#36017 = ORIENTED_EDGE ( 'NONE', *, *, #40467, .T. ) ;
#36018 = DIRECTION ( 'NONE',  ( 0.000000000000000000, 1.000000000000000000, 0.000000000000000000 ) ) ;
#36019 = CARTESIAN_POINT ( 'NONE',  ( -1.650000000000035216, 2.500000000000000000, -1.572243186433550211 ) ) ;
#36020 = AXIS2_PLACEMENT_3D ( 'NONE', #69654, #40874, #1553 ) ;
#36021 = LINE ( 'NONE', #125036, #92093 ) ;
#36022 = VERTEX_POINT ( 'NONE', #81313 ) ;
#36023 = CARTESIAN_POINT ( 'NONE',  ( 4.349999999999940137, 12.50000000000000000, -2.511473670974877948 ) ) ;
#36024 = DIRECTION ( 'NONE',  ( 0.000000000000000000, 1.000000000000000000, 0.000000000000000000 ) ) ;
#36025 = FACE_OUTER_BOUND ( 'NONE', #117748, .T. ) ;
#36026 = DIRECTION ( 'NONE',  ( 0.000000000000000000, -0.000000000000000000, 1.000000000000000000 ) ) ;
#36027 = CARTESIAN_POINT ( 'NONE',  ( -12.49999999999999289, 2.500000000000000000, 5.022947341949748790 ) ) ;
#36028 = CIRCLE ( 'NONE', #123840, 0.06509327318403741736 ) ;
#36029 = AXIS2_PLACEMENT_3D ( 'NONE', #77494, #38900, #97785 ) ;
#36030 = CONICAL_SURFACE ( 'NONE', #23500, 0.1000000000000000472, 0.003490658503988666988 ) ;
#36031 = ORIENTED_EDGE ( 'NONE', *, *, #118023, .T. ) ;
#36032 = DIRECTION ( 'NONE',  ( 0.000000000000000000, 0.000000000000000000, 1.000000000000000000 ) ) ;
#36033 = AXIS2_PLACEMENT_3D ( 'NONE', #101046, #51325, #91230 ) ;
#36034 = EDGE_CURVE ( 'NONE', #51049, #50142, #32110, .T. ) ;
#36035 = ORIENTED_EDGE ( 'NONE', *, *, #122180, .F. ) ;
#36036 = ORIENTED_EDGE ( 'NONE', *, *, #123170, .T. ) ;
#36037 = ORIENTED_EDGE ( 'NONE', *, *, #471, .T. ) ;
#36038 = DIRECTION ( 'NONE',  ( 0.000000000000000000, 0.000000000000000000, -1.000000000000000000 ) ) ;
#36039 = FACE_BOUND ( 'NONE', #42574, .T. ) ;
#36040 = CARTESIAN_POINT ( 'NONE',  ( -9.400000000000007461, 2.500000000000000000, 3.983716857408420076 ) ) ;
#36042 = LINE ( 'NONE', #55026, #79854 ) ;
#36041 = CIRCLE ( 'NONE', #71539, 0.1000000000000002554 ) ;
#36044 = DIRECTION ( 'NONE',  ( 0.000000000000000000, 1.000000000000000000, 0.000000000000000000 ) ) ;
#36043 = AXIS2_PLACEMENT_3D ( 'NONE', #21737, #19800, #71461 ) ;
#36045 = EDGE_CURVE ( 'NONE', #60753, #106745, #25833, .T. ) ;
#36046 = AXIS2_PLACEMENT_3D ( 'NONE', #23563, #42584, #82502 ) ;
#36047 = AXIS2_PLACEMENT_3D ( 'NONE', #121764, #119841, #100828 ) ;
#36048 = AXIS2_PLACEMENT_3D ( 'NONE', #121901, #91800, #13220 ) ;
#36049 = ORIENTED_EDGE ( 'NONE', *, *, #15701, .T. ) ;
#36050 = PLANE ( 'NONE',  #33452 ) ;
#36051 = CARTESIAN_POINT ( 'NONE',  ( -6.050000000000020250, 12.50000000000000000, -6.776507416713040577 ) ) ;
#36052 = DIRECTION ( 'NONE',  ( 0.000000000000000000, -0.000000000000000000, 1.000000000000000000 ) ) ;
#36053 = CIRCLE ( 'NONE', #94613, 0.06509327318403745899 ) ;
#36054 = CARTESIAN_POINT ( 'NONE',  ( -0.6500000000000389910, 12.50000000000000000, -1.883746621131363597 ) ) ;
#36055 = VERTEX_POINT ( 'NONE', #112707 ) ;
#36056 = DIRECTION ( 'NONE',  ( 0.000000000000000000, 0.000000000000000000, -1.000000000000000000 ) ) ;
#36057 = DIRECTION ( 'NONE',  ( 0.000000000000000000, 0.000000000000000000, 1.000000000000000000 ) ) ;
#36058 = VECTOR ( 'NONE', #95482, 1000.000000000000000 ) ;
#36059 = EDGE_LOOP ( 'NONE', ( #84541, #104760, #33414, #124802 ) ) ;
#36060 = DIRECTION ( 'NONE',  ( 0.000000000000000000, 0.000000000000000000, 1.000000000000000000 ) ) ;
#36061 = FACE_BOUND ( 'NONE', #12103, .T. ) ;
#36062 = DIRECTION ( 'NONE',  ( 0.000000000000000000, -0.000000000000000000, 1.000000000000000000 ) ) ;
#36063 = ORIENTED_EDGE ( 'NONE', *, *, #45022, .F. ) ;
#36064 = PLANE ( 'NONE',  #121802 ) ;
#36065 = DIRECTION ( 'NONE',  ( 0.000000000000000000, 1.000000000000000000, 0.000000000000000000 ) ) ;
#36066 = EDGE_LOOP ( 'NONE', ( #115074, #66647 ) ) ;
#36067 = ORIENTED_EDGE ( 'NONE', *, *, #101309, .T. ) ;
#36068 = CARTESIAN_POINT ( 'NONE',  ( 185.8750000000000000, 8.891194145520236347, 5.444286225454521982E-16 ) ) ;
#36069 = ORIENTED_EDGE ( 'NONE', *, *, #38758, .F. ) ;
#36070 = CARTESIAN_POINT ( 'NONE',  ( 184.5000000000000000, -6.267304879582558996, 4.236192450104883100 ) ) ;
#36071 = DIRECTION ( 'NONE',  ( 0.000000000000000000, 0.000000000000000000, 1.000000000000000000 ) ) ;
#36072 = ADVANCED_FACE ( 'NONE', ( #61014 ), #51220, .T. ) ;
#36073 = VECTOR ( 'NONE', #32394, 1000.000000000000000 ) ;
#36074 = CARTESIAN_POINT ( 'NONE',  ( -3.950000000000029932, 2.500000000000000000, -6.148780366869526226 ) ) ;
#36075 = DIRECTION ( 'NONE',  ( 0.000000000000000000, 0.000000000000000000, -1.000000000000000000 ) ) ;
#36076 = CIRCLE ( 'NONE', #119690, 0.1000000000000002554 ) ;
#36077 = CARTESIAN_POINT ( 'NONE',  ( 14.39999999999989555, 2.500000000000000000, -0.3464101615137782364 ) ) ;
#36078 = EDGE_CURVE ( 'NONE', #3072, #26527, #80221, .T. ) ;
#36079 = VECTOR ( 'NONE', #42599, 1000.000000000000000 ) ;
#36081 = ORIENTED_EDGE ( 'NONE', *, *, #74111, .F. ) ;
#36080 = VECTOR ( 'NONE', #10402, 1000.000000000000000 ) ;
#36082 = CARTESIAN_POINT ( 'NONE',  ( -9.350000000000006750, 12.50000000000000000, -2.511473670974877948 ) ) ;
#36083 = DIRECTION ( 'NONE',  ( 0.000000000000000000, -0.9999939076577903929, 0.003490651415223739937 ) ) ;
#36084 = LINE ( 'NONE', #66175, #99454 ) ;
#36085 = VECTOR ( 'NONE', #99705, 1000.000000000000000 ) ;
#36086 = CARTESIAN_POINT ( 'NONE',  ( -5.650000000000019895, 2.500000000000000000, 2.511473670974873507 ) ) ;
#36089 = VERTEX_POINT ( 'NONE', #111390 ) ;
#36088 = ORIENTED_EDGE ( 'NONE', *, *, #74212, .T. ) ;
#36087 = CONICAL_SURFACE ( 'NONE', #17176, 0.09999999999999982514, 0.003490658503988666988 ) ;
#36090 = ADVANCED_FACE ( 'NONE', ( #91127 ), #96918, .T. ) ;
#36091 = FACE_OUTER_BOUND ( 'NONE', #35016, .T. ) ;
#36092 = VERTEX_POINT ( 'NONE', #30297 ) ;
#36093 = ADVANCED_FACE ( 'NONE', ( #61683 ), #80015, .T. ) ;
#36094 = DIRECTION ( 'NONE',  ( 0.000000000000000000, 0.000000000000000000, -1.000000000000000000 ) ) ;
#36095 = DIRECTION ( 'NONE',  ( 0.000000000000000000, 0.000000000000000000, 1.000000000000000000 ) ) ;
#36096 = VECTOR ( 'NONE', #103123, 1000.000000000000000 ) ;
#36097 = ORIENTED_EDGE ( 'NONE', *, *, #125059, .T. ) ;
#36098 = CARTESIAN_POINT ( 'NONE',  ( 7.499999999999960032, 12.50000000000000000, -2.276824562219559311E-15 ) ) ;
#36099 = CARTESIAN_POINT ( 'NONE',  ( 12.89999999999989910, 2.500000000000000000, 0.5928203230275495006 ) ) ;
#36100 = CARTESIAN_POINT ( 'NONE',  ( 11.24999999999990763, 2.500000000000000000, 1.372243186433545370 ) ) ;
#36101 = DIRECTION ( 'NONE',  ( 0.000000000000000000, 0.000000000000000000, -1.000000000000000000 ) ) ;
#36102 = ORIENTED_EDGE ( 'NONE', *, *, #20618, .T. ) ;
#36103 = EDGE_CURVE ( 'NONE', #90584, #115529, #32232, .T. ) ;
#36104 = DIRECTION ( 'NONE',  ( 0.000000000000000000, 0.000000000000000000, -1.000000000000000000 ) ) ;
#36105 = DIRECTION ( 'NONE',  ( 0.000000000000000000, 0.000000000000000000, 1.000000000000000000 ) ) ;
#36106 = CARTESIAN_POINT ( 'NONE',  ( 186.3177083336747160, 4.367472073101515306, 7.564683531250000925 ) ) ;
#36107 = FACE_OUTER_BOUND ( 'NONE', #122428, .T. ) ;
#36108 = EDGE_CURVE ( 'NONE', #4340, #87979, #11913, .T. ) ;
#36109 = DIRECTION ( 'NONE',  ( -0.000000000000000000, -1.000000000000000000, -0.000000000000000000 ) ) ;
#36110 = CONICAL_SURFACE ( 'NONE', #109247, 0.1000000000000002554, 0.003490658503988666988 ) ;
#36111 = ORIENTED_EDGE ( 'NONE', *, *, #7111, .T. ) ;
#36112 = ORIENTED_EDGE ( 'NONE', *, *, #14807, .F. ) ;
#36113 = FACE_OUTER_BOUND ( 'NONE', #49214, .T. ) ;
#36114 = EDGE_LOOP ( 'NONE', ( #71242, #16864 ) ) ;
#36115 = CARTESIAN_POINT ( 'NONE',  ( 16.55874544816223448, 0.4845305829267578801, 6.091953208799004926 ) ) ;
#36117 = ORIENTED_EDGE ( 'NONE', *, *, #15399, .F. ) ;
#36116 = ORIENTED_EDGE ( 'NONE', *, *, #115661, .T. ) ;
#36118 = VERTEX_POINT ( 'NONE', #148 ) ;
#36119 = CARTESIAN_POINT ( 'NONE',  ( 3.099999999999945466, 2.500000000000000000, -3.983716857408426293 ) ) ;
#36120 = AXIS2_PLACEMENT_3D ( 'NONE', #118754, #120693, #121330 ) ;
#36121 =( GEOMETRIC_REPRESENTATION_CONTEXT ( 3 ) GLOBAL_UNCERTAINTY_ASSIGNED_CONTEXT ( ( #72987 ) ) GLOBAL_UNIT_ASSIGNED_CONTEXT ( ( #16004, #35040, #14064 ) ) REPRESENTATION_CONTEXT ( 'NONE', 'WORKASPACE' ) );
#36122 = LINE ( 'NONE', #104836, #105312 ) ;
#36123 = DIRECTION ( 'NONE',  ( -0.000000000000000000, -1.000000000000000000, -0.000000000000000000 ) ) ;
#36124 = CARTESIAN_POINT ( 'NONE',  ( 13.94999999999989804, 2.500000000000000000, 1.918653347947321564 ) ) ;
#36125 = CARTESIAN_POINT ( 'NONE',  ( 8.949999999999919353, 12.50000000000000000, 2.446380397790835826 ) ) ;
#36126 = VERTEX_POINT ( 'NONE', #51857 ) ;
#36127 = AXIS2_PLACEMENT_3D ( 'NONE', #93040, #13809, #54387 ) ;
#36128 = AXIS2_PLACEMENT_3D ( 'NONE', #120976, #31326, #90869 ) ;
#36129 = CARTESIAN_POINT ( 'NONE',  ( -2.499999999999996447, 2.500000000000000000, 4.230127018922196669 ) ) ;
#36130 = EDGE_LOOP ( 'NONE', ( #21744, #77276 ) ) ;
#36131 = VECTOR ( 'NONE', #67456, 1000.000000000000000 ) ;
#36132 = EDGE_LOOP ( 'NONE', ( #15616, #114676, #117990, #44042 ) ) ;
#36133 = ORIENTED_EDGE ( 'NONE', *, *, #98924, .T. ) ;
#36134 = AXIS2_PLACEMENT_3D ( 'NONE', #20404, #89137, #90408 ) ;
#36135 = EDGE_LOOP ( 'NONE', ( #123384, #90819, #3856, #23855 ) ) ;
#36136 = CARTESIAN_POINT ( 'NONE',  ( -13.14999999999999147, 12.50000000000000000, 2.576566944158914740 ) ) ;
#36137 = EDGE_LOOP ( 'NONE', ( #107114, #36930, #121102, #70757 ) ) ;
#36138 = VERTEX_POINT ( 'NONE', #91768 ) ;
#36139 = AXIS2_PLACEMENT_3D ( 'NONE', #71959, #113810, #122349 ) ;
#36140 = CARTESIAN_POINT ( 'NONE',  ( -11.69999999999999929, 12.50000000000000000, -4.265033745738161741 ) ) ;
#36141 = CARTESIAN_POINT ( 'NONE',  ( 4.199999999999939782, 2.500000000000000000, -2.276824562219559311E-15 ) ) ;
#36142 = CARTESIAN_POINT ( 'NONE',  ( -1.250000000000036193, 2.500000000000000000, 5.902370205355745192 ) ) ;
#36143 = AXIS2_PLACEMENT_3D ( 'NONE', #19304, #60559, #38329 ) ;
#36144 = DIRECTION ( 'NONE',  ( 0.000000000000000000, 0.000000000000000000, 1.000000000000000000 ) ) ;
#36145 = CIRCLE ( 'NONE', #117669, 0.06509327318403745899 ) ;
#36146 = AXIS2_PLACEMENT_3D ( 'NONE', #80546, #103401, #110634 ) ;
#36147 = EDGE_CURVE ( 'NONE', #13514, #63649, #113656, .T. ) ;
#36148 = DIRECTION ( 'NONE',  ( 0.000000000000000000, 0.000000000000000000, 1.000000000000000000 ) ) ;
#36149 = ORIENTED_EDGE ( 'NONE', *, *, #97974, .F. ) ;
#36150 = ADVANCED_FACE ( 'NONE', ( #110123 ), #73949, .T. ) ;
#36151 = CIRCLE ( 'NONE', #56951, 0.06509327318403745899 ) ;
#36152 = EDGE_CURVE ( 'NONE', #54054, #79693, #90670, .T. ) ;
#36153 = DIRECTION ( 'NONE',  ( 0.000000000000000000, -0.000000000000000000, 1.000000000000000000 ) ) ;
#36154 = EDGE_CURVE ( 'NONE', #111830, #31107, #72140, .T. ) ;
#36155 = VERTEX_POINT ( 'NONE', #90463 ) ;
#36156 = DIRECTION ( 'NONE',  ( 0.000000000000000000, 1.000000000000000000, 0.000000000000000000 ) ) ;
#36157 = EDGE_LOOP ( 'NONE', ( #126404, #108385, #117041, #55018 ) ) ;
#36158 = AXIS2_PLACEMENT_3D ( 'NONE', #10939, #79709, #12246 ) ;
#36159 = CARTESIAN_POINT ( 'NONE',  ( -8.550000000000013145, 2.500000000000000000, 2.511473670974873507 ) ) ;
#36160 = EDGE_CURVE ( 'NONE', #104949, #17389, #17492, .T. ) ;
#36161 = VERTEX_POINT ( 'NONE', #121871 ) ;
#36162 = ORIENTED_EDGE ( 'NONE', *, *, #40193, .T. ) ;
#36163 = FACE_OUTER_BOUND ( 'NONE', #50120, .T. ) ;
#36164 = DIRECTION ( 'NONE',  ( 0.000000000000000000, -0.000000000000000000, 1.000000000000000000 ) ) ;
#36165 = EDGE_CURVE ( 'NONE', #86890, #71724, #61448, .T. ) ;
#36166 = ADVANCED_FACE ( 'NONE', ( #115239 ), #88510, .T. ) ;
#36167 = DIRECTION ( 'NONE',  ( 0.000000000000000000, 0.000000000000000000, -1.000000000000000000 ) ) ;
#36168 = CARTESIAN_POINT ( 'NONE',  ( -1.250000000000035749, 12.50000000000000000, -7.253104124594891289 ) ) ;
#36169 = CARTESIAN_POINT ( 'NONE',  ( -6.250000000000017764, 2.500000000000000000, 7.288010851410849256 ) ) ;
#36170 = VERTEX_POINT ( 'NONE', #26260 ) ;
#36171 = CARTESIAN_POINT ( 'NONE',  ( -8.750000000000008882, 12.50000000000000000, 1.472243186433545459 ) ) ;
#36173 = CONICAL_SURFACE ( 'NONE', #29900, 0.09999999999999999167, 0.003490658503988666988 ) ;
#36172 = DIRECTION ( 'NONE',  ( 0.000000000000000000, 1.000000000000000000, 0.000000000000000000 ) ) ;
#36174 = AXIS2_PLACEMENT_3D ( 'NONE', #73993, #105386, #44529 ) ;
#36175 = DIRECTION ( 'NONE',  ( 0.000000000000000000, 0.000000000000000000, 1.000000000000000000 ) ) ;
#36176 = CARTESIAN_POINT ( 'NONE',  ( -11.64999999999999680, 2.500000000000000000, 7.188010851410848723 ) ) ;
#36177 = PLANE ( 'NONE',  #62585 ) ;
#36178 = EDGE_LOOP ( 'NONE', ( #82732, #124968 ) ) ;
#36179 = AXIS2_PLACEMENT_3D ( 'NONE', #79024, #99300, #111693 ) ;
#36180 = VECTOR ( 'NONE', #100763, 1000.000000000000000 ) ;
#36181 = ORIENTED_EDGE ( 'NONE', *, *, #40226, .T. ) ;
#36182 = VECTOR ( 'NONE', #49648, 1000.000000000000000 ) ;
#36183 = AXIS2_PLACEMENT_3D ( 'NONE', #127281, #27767, #17281 ) ;
#36184 = DIRECTION ( 'NONE',  ( 0.000000000000000000, 1.000000000000000000, 0.000000000000000000 ) ) ;
#36185 = ORIENTED_EDGE ( 'NONE', *, *, #52568, .F. ) ;
#36186 = CARTESIAN_POINT ( 'NONE',  ( -6.650000000000019007, 12.50000000000000000, -5.802370205355749988 ) ) ;
#36187 = FACE_OUTER_BOUND ( 'NONE', #15313, .T. ) ;
#36188 = CONICAL_SURFACE ( 'NONE', #50844, 0.1000000000000000472, 0.003490658503988666988 ) ;
#36189 = CIRCLE ( 'NONE', #34127, 0.06509327318403745899 ) ;
#36190 = AXIS2_PLACEMENT_3D ( 'NONE', #127291, #104415, #87336 ) ;
#36191 = VECTOR ( 'NONE', #119015, 1000.000000000000000 ) ;
#36192 = AXIS2_PLACEMENT_3D ( 'NONE', #71877, #50951, #82343 ) ;
#36193 = VERTEX_POINT ( 'NONE', #24960 ) ;
#36194 = CARTESIAN_POINT ( 'NONE',  ( 186.0000000000000000, 0.000000000000000000, 7.700000000000000178 ) ) ;
#36195 = CARTESIAN_POINT ( 'NONE',  ( 0.5999999999999555689, 2.500000000000000000, 4.776537180435972196 ) ) ;
#36196 = DIRECTION ( 'NONE',  ( -4.274815082592931898E-19, -0.9999939076577903929, -0.003490651415223739937 ) ) ;
#36197 = DIRECTION ( 'NONE',  ( 0.000000000000000000, 0.000000000000000000, -1.000000000000000000 ) ) ;
#36198 = ORIENTED_EDGE ( 'NONE', *, *, #24759, .T. ) ;
#36199 = AXIS2_PLACEMENT_3D ( 'NONE', #87813, #26990, #26345 ) ;
#36200 = PLANE ( 'NONE',  #375 ) ;
#36201 = LINE ( 'NONE', #13958, #55972 ) ;
#36202 = EDGE_LOOP ( 'NONE', ( #83443, #3376 ) ) ;
#36203 = CARTESIAN_POINT ( 'NONE',  ( 0.000000000000000000, -0.5000000000000000000, 0.000000000000000000 ) ) ;
#36204 = DIRECTION ( 'NONE',  ( -1.000000000000000000, -0.000000000000000000, -0.000000000000000000 ) ) ;
#36205 = DIRECTION ( 'NONE',  ( -0.000000000000000000, -1.000000000000000000, -0.000000000000000000 ) ) ;
#36206 = AXIS2_PLACEMENT_3D ( 'NONE', #38133, #66298, #75470 ) ;
#36207 = EDGE_CURVE ( 'NONE', #55939, #4440, #84408, .T. ) ;
#36208 = ORIENTED_EDGE ( 'NONE', *, *, #37325, .T. ) ;
#36209 = LINE ( 'NONE', #58428, #109606 ) ;
#36210 = ORIENTED_EDGE ( 'NONE', *, *, #5937, .T. ) ;
#36211 = LINE ( 'NONE', #89163, #35404 ) ;
#36212 = CARTESIAN_POINT ( 'NONE',  ( -9.350000000000006750, 2.500000000000000000, 2.611473670974873151 ) ) ;
#36213 = CARTESIAN_POINT ( 'NONE',  ( -12.49999999999999289, 12.50000000000000000, 5.022947341949748790 ) ) ;
#36214 = CONICAL_SURFACE ( 'NONE', #2735, 0.09999999999999982514, 0.003490658503988666988 ) ;
#36215 = ORIENTED_EDGE ( 'NONE', *, *, #35919, .T. ) ;
#36216 = AXIS2_PLACEMENT_3D ( 'NONE', #21244, #71642, #72931 ) ;
#36217 = AXIS2_PLACEMENT_3D ( 'NONE', #77286, #127675, #79868 ) ;
#36218 = CARTESIAN_POINT ( 'NONE',  ( 6.249999999999930722, 2.500000000000000000, 7.088010851410848190 ) ) ;
#36219 = DIRECTION ( 'NONE',  ( 0.000000000000000000, 0.000000000000000000, -1.000000000000000000 ) ) ;
#36220 = EDGE_LOOP ( 'NONE', ( #39395, #66330, #82392, #70243 ) ) ;
#36221 = ORIENTED_EDGE ( 'NONE', *, *, #11522, .T. ) ;
#36222 = CONICAL_SURFACE ( 'NONE', #126085, 0.1000000000000002554, 0.003490658503988666988 ) ;
#36223 = FACE_OUTER_BOUND ( 'NONE', #65100, .T. ) ;
#36224 = AXIS2_PLACEMENT_3D ( 'NONE', #121729, #25966, #46238 ) ;
#36225 = AXIS2_PLACEMENT_3D ( 'NONE', #60342, #117942, #69486 ) ;
#36226 = EDGE_LOOP ( 'NONE', ( #5655, #108563 ) ) ;
#36227 = LINE ( 'NONE', #37518, #2481 ) ;
#36228 = DIRECTION ( 'NONE',  ( 0.000000000000000000, 1.000000000000000000, 0.000000000000000000 ) ) ;
#36229 = ORIENTED_EDGE ( 'NONE', *, *, #110080, .F. ) ;
#36230 = CARTESIAN_POINT ( 'NONE',  ( -4.350000000000023626, 2.500000000000000000, 6.841600689897072485 ) ) ;
#36231 = CARTESIAN_POINT ( 'NONE',  ( 13.34999999999990017, 2.500000000000000000, 2.265063509461097357 ) ) ;
#36232 = CIRCLE ( 'NONE', #19489, 0.1000000000000002554 ) ;
#36233 = VERTEX_POINT ( 'NONE', #63606 ) ;
#36234 = DIRECTION ( 'NONE',  ( -0.000000000000000000, -1.000000000000000000, -0.000000000000000000 ) ) ;
#36235 = FACE_OUTER_BOUND ( 'NONE', #49503, .T. ) ;
#36236 = CIRCLE ( 'NONE', #11174, 0.09999999999999982514 ) ;
#36237 = CIRCLE ( 'NONE', #73880, 0.06509327318403745899 ) ;
#36238 = AXIS2_PLACEMENT_3D ( 'NONE', #37872, #117697, #8400 ) ;
#36239 = DIRECTION ( 'NONE',  ( 0.000000000000000000, 0.000000000000000000, -1.000000000000000000 ) ) ;
#36240 = LINE ( 'NONE', #94486, #82176 ) ;
#36241 = CARTESIAN_POINT ( 'NONE',  ( 6.449999999999933564, 12.50000000000000000, -6.841600689897078702 ) ) ;
#36242 = AXIS2_PLACEMENT_3D ( 'NONE', #6265, #44269, #105124 ) ;
#36243 = CARTESIAN_POINT ( 'NONE',  ( -12.09999999999999609, 2.500000000000000000, 4.330127018922196314 ) ) ;
#36244 = EDGE_CURVE ( 'NONE', #52125, #76693, #64239, .T. ) ;
#36245 = EDGE_CURVE ( 'NONE', #14798, #86952, #101144, .T. ) ;
#36246 = ORIENTED_EDGE ( 'NONE', *, *, #117163, .T. ) ;
#36247 = ORIENTED_EDGE ( 'NONE', *, *, #107368, .T. ) ;
#36248 = ORIENTED_EDGE ( 'NONE', *, *, #94990, .T. ) ;
#36249 = ORIENTED_EDGE ( 'NONE', *, *, #60271, .F. ) ;
#36250 = DIRECTION ( 'NONE',  ( 0.000000000000000000, -0.9999939076577903929, 0.003490651415223739937 ) ) ;
#36251 = CARTESIAN_POINT ( 'NONE',  ( -5.000000000000023093, 12.50000000000000000, 0.6928203230275494784 ) ) ;
#36252 = DIRECTION ( 'NONE',  ( -0.000000000000000000, 1.000000000000000000, -0.000000000000000000 ) ) ;
#36253 = ORIENTED_EDGE ( 'NONE', *, *, #107201, .T. ) ;
#36254 = EDGE_CURVE ( 'NONE', #86066, #107157, #105244, .T. ) ;
#36255 = FACE_BOUND ( 'NONE', #30367, .T. ) ;
#36256 = EDGE_CURVE ( 'NONE', #89857, #82534, #125718, .T. ) ;
#36257 = DIRECTION ( 'NONE',  ( 0.000000000000000000, -0.9999939076577903929, 0.003490651415223739937 ) ) ;
#36258 = DIRECTION ( 'NONE',  ( -4.274815082592931898E-19, -0.9999939076577903929, -0.003490651415223739937 ) ) ;
#36259 = DIRECTION ( 'NONE',  ( 0.000000000000000000, 1.000000000000000000, 0.000000000000000000 ) ) ;
#36260 = DIRECTION ( 'NONE',  ( 1.000000000000000000, -0.000000000000000000, -0.000000000000000000 ) ) ;
#36261 = CARTESIAN_POINT ( 'NONE',  ( 8.549999999999918998, 12.50000000000000000, 6.841600689897072485 ) ) ;
#36262 = EDGE_CURVE ( 'NONE', #29188, #9068, #19571, .T. ) ;
#36263 = CARTESIAN_POINT ( 'NONE',  ( 8.349999999999919709, 12.50000000000000000, 5.802370205355744659 ) ) ;
#36264 = EDGE_CURVE ( 'NONE', #40264, #31157, #36317, .T. ) ;
#36265 = DIRECTION ( 'NONE',  ( -0.000000000000000000, -1.000000000000000000, -0.000000000000000000 ) ) ;
#36266 = CARTESIAN_POINT ( 'NONE',  ( 12.89999999999990266, 2.500000000000000000, 3.637306695894644726 ) ) ;
#36267 = CIRCLE ( 'NONE', #40474, 0.1000000000000002554 ) ;
#36268 = EDGE_CURVE ( 'NONE', #48509, #108123, #35439, .T. ) ;
#36269 = CARTESIAN_POINT ( 'NONE',  ( -13.34999999999999076, 2.500000000000000000, 2.857883832488652853 ) ) ;
#36270 = ADVANCED_FACE ( 'NONE', ( #83252 ), #97023, .T. ) ;
#36271 = ADVANCED_FACE ( 'NONE', ( #75991 ), #55068, .T. ) ;
#36272 = DIRECTION ( 'NONE',  ( 0.000000000000000000, 1.000000000000000000, 0.000000000000000000 ) ) ;
#36273 = CIRCLE ( 'NONE', #63448, 0.06509327318403745899 ) ;
#36275 = ORIENTED_EDGE ( 'NONE', *, *, #93721, .T. ) ;
#36274 = CONICAL_SURFACE ( 'NONE', #40485, 0.1000000000000002554, 0.003490658503988666988 ) ;
#36276 = ORIENTED_EDGE ( 'NONE', *, *, #100392, .F. ) ;
#36277 = ORIENTED_EDGE ( 'NONE', *, *, #71746, .T. ) ;
#36278 = AXIS2_PLACEMENT_3D ( 'NONE', #9013, #107223, #28677 ) ;
#36279 = ORIENTED_EDGE ( 'NONE', *, *, #122846, .F. ) ;
#36280 = DIRECTION ( 'NONE',  ( 0.000000000000000000, 0.000000000000000000, 1.000000000000000000 ) ) ;
#36281 = ORIENTED_EDGE ( 'NONE', *, *, #123019, .F. ) ;
#36282 = VECTOR ( 'NONE', #93155, 1000.000000000000000 ) ;
#36283 = CARTESIAN_POINT ( 'NONE',  ( 12.93920187831608892, 1.500000000000000444, -10.00000000000000000 ) ) ;
#36284 = ORIENTED_EDGE ( 'NONE', *, *, #52247, .F. ) ;
#36285 = EDGE_CURVE ( 'NONE', #61216, #48774, #38563, .T. ) ;
#36286 = ORIENTED_EDGE ( 'NONE', *, *, #20763, .F. ) ;
#36287 = DIRECTION ( 'NONE',  ( 0.000000000000000000, 0.000000000000000000, 1.000000000000000000 ) ) ;
#36288 = AXIS2_PLACEMENT_3D ( 'NONE', #16347, #26197, #56287 ) ;
#36289 = CIRCLE ( 'NONE', #126148, 0.06509327318403745899 ) ;
#36290 = VECTOR ( 'NONE', #50036, 1000.000000000000000 ) ;
#36292 = CARTESIAN_POINT ( 'NONE',  ( 2.500000000000002220, -2.500000000000000444, 10.00000000000000178 ) ) ;
#36291 = PRODUCT_DEFINITION_CONTEXT ( 'detailed design', #4514, 'design' ) ;
#36293 = DIRECTION ( 'NONE',  ( -4.274815082592931898E-19, -0.9999939076577903929, -0.003490651415223739937 ) ) ;
#36294 = CARTESIAN_POINT ( 'NONE',  ( 12.09999999999990550, 12.50000000000000000, -5.022947341949754119 ) ) ;
#36295 = CIRCLE ( 'NONE', #86430, 0.06509327318403745899 ) ;
#36296 = DIRECTION ( 'NONE',  ( 0.000000000000000000, 1.000000000000000000, 0.000000000000000000 ) ) ;
#36297 = CIRCLE ( 'NONE', #61319, 0.06509327318403743123 ) ;
#36298 = VERTEX_POINT ( 'NONE', #5308 ) ;
#36299 = VERTEX_POINT ( 'NONE', #113334 ) ;
#36300 = ORIENTED_EDGE ( 'NONE', *, *, #61124, .F. ) ;
#36301 = ORIENTED_EDGE ( 'NONE', *, *, #126260, .F. ) ;
#36302 = DIRECTION ( 'NONE',  ( -0.000000000000000000, -1.000000000000000000, -0.000000000000000000 ) ) ;
#36303 = ORIENTED_EDGE ( 'NONE', *, *, #2274, .F. ) ;
#36304 = VERTEX_POINT ( 'NONE', #15774 ) ;
#36305 = VECTOR ( 'NONE', #45228, 1000.000000000000000 ) ;
#36306 = DIRECTION ( 'NONE',  ( 0.000000000000000000, 0.000000000000000000, 1.000000000000000000 ) ) ;
#36307 = CARTESIAN_POINT ( 'NONE',  ( -5.200000000000022382, 2.500000000000000000, 4.576537180435972019 ) ) ;
#36308 = DIRECTION ( 'NONE',  ( 0.000000000000000000, 0.000000000000000000, 1.000000000000000000 ) ) ;
#36309 = CARTESIAN_POINT ( 'NONE',  ( -1.250000000000001554, 12.50000000000000000, 6.495190528383297135 ) ) ;
#36310 = LINE ( 'NONE', #13416, #12619 ) ;
#36311 = DIRECTION ( 'NONE',  ( -4.274815082592931898E-19, -0.9999939076577903929, -0.003490651415223739937 ) ) ;
#36312 = EDGE_CURVE ( 'NONE', #40294, #68357, #105345, .T. ) ;
#36314 = EDGE_LOOP ( 'NONE', ( #1930, #113902, #22307, #16619 ) ) ;
#36313 = CONICAL_SURFACE ( 'NONE', #23676, 0.1000000000000000472, 0.003490658503988666988 ) ;
#36315 = EDGE_CURVE ( 'NONE', #85897, #75229, #99093, .T. ) ;
#36316 = DIRECTION ( 'NONE',  ( 0.000000000000000000, -0.9999939076577903929, 0.003490651415223739937 ) ) ;
#36317 = CIRCLE ( 'NONE', #126276, 0.1000000000000000472 ) ;
#36318 = VECTOR ( 'NONE', #42001, 1000.000000000000000 ) ;
#36319 = VERTEX_POINT ( 'NONE', #95638 ) ;
#36321 = EDGE_CURVE ( 'NONE', #77871, #82944, #48920, .T. ) ;
#36320 = CARTESIAN_POINT ( 'NONE',  ( 0.5999999999999547917, 2.500000000000000000, 3.883716857408420431 ) ) ;
#36322 = ORIENTED_EDGE ( 'NONE', *, *, #74269, .F. ) ;
#36323 = DIRECTION ( 'NONE',  ( 0.000000000000000000, 0.000000000000000000, -1.000000000000000000 ) ) ;
#36324 = CARTESIAN_POINT ( 'NONE',  ( -14.54999999999998472, 12.50000000000000000, -2.165063509461099489 ) ) ;
#36325 = ORIENTED_EDGE ( 'NONE', *, *, #1698, .T. ) ;
#36326 = DIRECTION ( 'NONE',  ( 0.000000000000000000, 0.000000000000000000, -1.000000000000000000 ) ) ;
#36327 = EDGE_CURVE ( 'NONE', #37524, #27204, #74041, .T. ) ;
#36329 = CIRCLE ( 'NONE', #44724, 0.06509327318403745899 ) ;
#36328 = CARTESIAN_POINT ( 'NONE',  ( 3.749999999999976907, 2.500000000000000000, 2.065063509461097624 ) ) ;
#36330 = ORIENTED_EDGE ( 'NONE', *, *, #32287, .F. ) ;
#36331 = ADVANCED_FACE ( 'NONE', ( #93074 ), #46860, .T. ) ;
#36332 = CIRCLE ( 'NONE', #115713, 0.1000000000000000472 ) ;
#36333 = EDGE_CURVE ( 'NONE', #17919, #7073, #32310, .T. ) ;
#36334 = AXIS2_PLACEMENT_3D ( 'NONE', #62270, #73354, #12502 ) ;
#36335 = EDGE_CURVE ( 'NONE', #127093, #110872, #10320, .T. ) ;
#36336 = CARTESIAN_POINT ( 'NONE',  ( 9.549999999999915445, 12.50000000000000000, -2.165063509461101710 ) ) ;
#36337 = VERTEX_POINT ( 'NONE', #46521 ) ;
#36338 = ORIENTED_EDGE ( 'NONE', *, *, #59850, .T. ) ;
#36339 = CARTESIAN_POINT ( 'NONE',  ( 8.099999999999923261, 2.500000000000000000, 4.576537180435972019 ) ) ;
#36340 = FACE_OUTER_BOUND ( 'NONE', #53450, .T. ) ;
#36341 = CARTESIAN_POINT ( 'NONE',  ( 186.9218750003414016, 0.000000000000000000, 7.564683531250000925 ) ) ;
#36342 = AXIS2_PLACEMENT_3D ( 'NONE', #116252, #37708, #35148 ) ;
#36343 = CARTESIAN_POINT ( 'NONE',  ( 105.0000000000000142, 8.500000000000000000, 0.2500000000000003886 ) ) ;
#36344 = EDGE_CURVE ( 'NONE', #63527, #104908, #71992, .T. ) ;
#36345 = DIRECTION ( 'NONE',  ( 0.000000000000000000, 1.000000000000000000, 0.000000000000000000 ) ) ;
#36346 = AXIS2_PLACEMENT_3D ( 'NONE', #98990, #29600, #70180 ) ;
#36347 = CONICAL_SURFACE ( 'NONE', #73881, 0.1000000000000002554, 0.003490658503988666988 ) ;
#36348 = CARTESIAN_POINT ( 'NONE',  ( 9.599999999999914380, 12.50000000000000000, -5.022947341949754119 ) ) ;
#36349 = CIRCLE ( 'NONE', #84349, 0.09999999999999982514 ) ;
#36350 = ORIENTED_EDGE ( 'NONE', *, *, #60815, .T. ) ;
#36351 = CIRCLE ( 'NONE', #92772, 0.06509327318403745899 ) ;
#36352 = CARTESIAN_POINT ( 'NONE',  ( -1.650000000000034328, 2.500000000000000000, -6.495190528383302464 ) ) ;
#36353 = ORIENTED_EDGE ( 'NONE', *, *, #23441, .F. ) ;
#36354 = DIRECTION ( 'NONE',  ( 0.000000000000000000, 0.000000000000000000, 1.000000000000000000 ) ) ;
#36355 = EDGE_CURVE ( 'NONE', #78070, #90721, #129480, .T. ) ;
#36356 = PLANE ( 'NONE',  #73655 ) ;
#36357 = DIRECTION ( 'NONE',  ( -4.274815082592931898E-19, -0.9999939076577903929, -0.003490651415223739937 ) ) ;
#36358 = ORIENTED_EDGE ( 'NONE', *, *, #73394, .F. ) ;
#36359 = CARTESIAN_POINT ( 'NONE',  ( 12.04999999999990834, 12.50000000000000000, -2.099970236277064473 ) ) ;
#36360 = DIRECTION ( 'NONE',  ( -4.274815082592931898E-19, -0.9999939076577903929, -0.003490651415223739937 ) ) ;
#36361 = AXIS2_PLACEMENT_3D ( 'NONE', #12293, #24065, #121601 ) ;
#36362 = EDGE_LOOP ( 'NONE', ( #127268, #21059, #16395, #30662 ) ) ;
#36363 = FACE_OUTER_BOUND ( 'NONE', #9043, .T. ) ;
#36364 = AXIS2_PLACEMENT_3D ( 'NONE', #123287, #32993, #92530 ) ;
#36365 = AXIS2_PLACEMENT_3D ( 'NONE', #89441, #91372, #30546 ) ;
#36366 = EDGE_CURVE ( 'NONE', #107907, #44142, #88708, .T. ) ;
#36367 = ORIENTED_EDGE ( 'NONE', *, *, #17438, .T. ) ;
#36368 = ORIENTED_EDGE ( 'NONE', *, *, #119197, .T. ) ;
#36369 = CARTESIAN_POINT ( 'NONE',  ( -2.950000000000033484, 12.50000000000000000, -6.495190528383302464 ) ) ;
#36370 = VECTOR ( 'NONE', #94543, 1000.000000000000000 ) ;
#36371 = ORIENTED_EDGE ( 'NONE', *, *, #31744, .F. ) ;
#36372 = CARTESIAN_POINT ( 'NONE',  ( 12.89999999999990266, 2.500000000000000000, -3.537306695894649966 ) ) ;
#36373 = DIRECTION ( 'NONE',  ( -0.000000000000000000, 1.000000000000000000, -0.000000000000000000 ) ) ;
#36374 = DIRECTION ( 'NONE',  ( 0.000000000000000000, 0.000000000000000000, -1.000000000000000000 ) ) ;
#36376 = EDGE_LOOP ( 'NONE', ( #80683, #65530 ) ) ;
#36375 = AXIS2_PLACEMENT_3D ( 'NONE', #30734, #70630, #11047 ) ;
#36377 = VECTOR ( 'NONE', #26163, 1000.000000000000000 ) ;
#36378 = FACE_BOUND ( 'NONE', #80539, .T. ) ;
#36380 = VERTEX_POINT ( 'NONE', #6572 ) ;
#36379 = CARTESIAN_POINT ( 'NONE',  ( -11.64999999999999680, 2.500000000000000000, -6.495190528383298911 ) ) ;
#36381 = AXIS2_PLACEMENT_3D ( 'NONE', #123693, #34721, #114529 ) ;
#36382 = DIRECTION ( 'NONE',  ( -0.000000000000000000, -1.000000000000000000, -0.000000000000000000 ) ) ;
#36383 = EDGE_CURVE ( 'NONE', #55213, #14119, #56344, .T. ) ;
#36384 = DIRECTION ( 'NONE',  ( 0.000000000000000000, 0.000000000000000000, 1.000000000000000000 ) ) ;
#36385 = VERTEX_POINT ( 'NONE', #110445 ) ;
#36386 = VERTEX_POINT ( 'NONE', #90811 ) ;
#36387 = ORIENTED_EDGE ( 'NONE', *, *, #34396, .T. ) ;
#36388 = DIRECTION ( 'NONE',  ( -0.000000000000000000, 1.000000000000000000, -0.000000000000000000 ) ) ;
#36389 = FACE_OUTER_BOUND ( 'NONE', #115900, .T. ) ;
#36390 = CARTESIAN_POINT ( 'NONE',  ( -4.150000000000024336, 2.500000000000000000, 1.472243186433545459 ) ) ;
#36391 = FACE_BOUND ( 'NONE', #73501, .T. ) ;
#36392 = ORIENTED_EDGE ( 'NONE', *, *, #3023, .T. ) ;
#36393 = CARTESIAN_POINT ( 'NONE',  ( 185.9843750003414016, -8.734944146203032389, -1.604583208406768146E-15 ) ) ;
#36394 = DIRECTION ( 'NONE',  ( 0.000000000000000000, -0.9999939076577903929, 0.003490651415223739937 ) ) ;
#36395 = CARTESIAN_POINT ( 'NONE',  ( -5.450000000000019718, 2.500000000000000000, 6.495190528383297135 ) ) ;
#36396 = AXIS2_PLACEMENT_3D ( 'NONE', #49753, #48439, #18966 ) ;
#36397 = CARTESIAN_POINT ( 'NONE',  ( 1.699999999999951994, 12.50000000000000000, -4.395220292106239768 ) ) ;
#36398 = DIRECTION ( 'NONE',  ( -0.000000000000000000, -1.000000000000000000, -0.000000000000000000 ) ) ;
#36399 = DIRECTION ( 'NONE',  ( 0.000000000000000000, -0.000000000000000000, 1.000000000000000000 ) ) ;
#36400 = DIRECTION ( 'NONE',  ( 0.000000000000000000, 1.000000000000000000, 0.000000000000000000 ) ) ;
#36401 = CARTESIAN_POINT ( 'NONE',  ( 12.69999999999990337, 2.500000000000000000, -4.676537180435978769 ) ) ;
#36402 = AXIS2_PLACEMENT_3D ( 'NONE', #106102, #16399, #96259 ) ;
#36403 = AXIS2_PLACEMENT_3D ( 'NONE', #62299, #72116, #102217 ) ;
#36404 = CARTESIAN_POINT ( 'NONE',  ( 8.349999999999919709, 2.500000000000000000, -2.165063509461101710 ) ) ;
#36405 = EDGE_CURVE ( 'NONE', #122680, #119243, #63582, .T. ) ;
#36406 = VERTEX_POINT ( 'NONE', #41095 ) ;
#36407 = ORIENTED_EDGE ( 'NONE', *, *, #82452, .F. ) ;
#36408 = ORIENTED_EDGE ( 'NONE', *, *, #28169, .F. ) ;
#36409 = EDGE_LOOP ( 'NONE', ( #34937, #53870, #103938, #13561 ) ) ;
#36410 = ORIENTED_EDGE ( 'NONE', *, *, #112470, .T. ) ;
#36411 = CARTESIAN_POINT ( 'NONE',  ( -9.800000000000006040, 2.500000000000000000, 0.2464101615137735679 ) ) ;
#36412 = DIRECTION ( 'NONE',  ( -4.274815082592931898E-19, -0.9999939076577903929, -0.003490651415223739937 ) ) ;
#36413 = ORIENTED_EDGE ( 'NONE', *, *, #93211, .F. ) ;
#36414 = FACE_BOUND ( 'NONE', #37277, .T. ) ;
#36415 = AXIS2_PLACEMENT_3D ( 'NONE', #18175, #40423, #30604 ) ;
#36416 = DIRECTION ( 'NONE',  ( -0.000000000000000000, -1.000000000000000000, -0.000000000000000000 ) ) ;
#36417 = AXIS2_PLACEMENT_3D ( 'NONE', #68951, #67653, #87924 ) ;
#36418 = CARTESIAN_POINT ( 'NONE',  ( 14.14999999999989200, 12.50000000000000000, -2.165063509461101710 ) ) ;
#36419 = ADVANCED_FACE ( 'NONE', ( #100615 ), #53119, .T. ) ;
#36420 = CARTESIAN_POINT ( 'NONE',  ( 1.249999999999952038, 12.50000000000000000, 2.857883832488649301 ) ) ;
#36421 = ADVANCED_FACE ( 'NONE', ( #120281 ), #103296, .T. ) ;
#36422 = CARTESIAN_POINT ( 'NONE',  ( 14.14999999999989733, 2.500000000000000000, 2.857883832488649301 ) ) ;
#36423 = EDGE_CURVE ( 'NONE', #5118, #107, #7123, .T. ) ;
#36424 = DIRECTION ( 'NONE',  ( 0.000000000000000000, 1.000000000000000000, 0.000000000000000000 ) ) ;
#36425 = EDGE_CURVE ( 'NONE', #30237, #18179, #86553, .T. ) ;
#36426 = ORIENTED_EDGE ( 'NONE', *, *, #22588, .T. ) ;
#36427 = CARTESIAN_POINT ( 'NONE',  ( 16.88398462908939024, -2.500000000000000000, 4.430583899596162389 ) ) ;
#36428 = VERTEX_POINT ( 'NONE', #79074 ) ;
#36429 = VECTOR ( 'NONE', #45234, 1000.000000000000000 ) ;
#36430 = AXIS2_PLACEMENT_3D ( 'NONE', #12405, #92924, #90976 ) ;
#36431 = AXIS2_PLACEMENT_3D ( 'NONE', #117980, #9970, #109457 ) ;
#36432 = ORIENTED_EDGE ( 'NONE', *, *, #36007, .T. ) ;
#36433 = ORIENTED_EDGE ( 'NONE', *, *, #68518, .T. ) ;
#36434 = CARTESIAN_POINT ( 'NONE',  ( -10.60000000000000142, 2.500000000000000000, 0.4464101615137736623 ) ) ;
#36435 = DIRECTION ( 'NONE',  ( -0.000000000000000000, 1.000000000000000000, -0.000000000000000000 ) ) ;
#36437 = AXIS2_PLACEMENT_3D ( 'NONE', #106266, #114159, #84691 ) ;
#36436 = FACE_OUTER_BOUND ( 'NONE', #81082, .T. ) ;
#36438 = ORIENTED_EDGE ( 'NONE', *, *, #6779, .F. ) ;
#36439 = EDGE_CURVE ( 'NONE', #119031, #22231, #51071, .T. ) ;
#36440 = CARTESIAN_POINT ( 'NONE',  ( 16.31260002278204979, 1.500000000000484945, -6.357732714000876584 ) ) ;
#36441 = AXIS2_PLACEMENT_3D ( 'NONE', #3059, #90782, #10902 ) ;
#36442 = EDGE_CURVE ( 'NONE', #76941, #93392, #20789, .T. ) ;
#36443 = CARTESIAN_POINT ( 'NONE',  ( 14.59999999999989484, 12.50000000000000000, -0.7579135962115916003 ) ) ;
#36444 = EDGE_CURVE ( 'NONE', #84243, #73744, #30141, .T. ) ;
#36445 = DIRECTION ( 'NONE',  ( -0.000000000000000000, -1.000000000000000000, -0.000000000000000000 ) ) ;
#36446 = CARTESIAN_POINT ( 'NONE',  ( 186.9843750003414300, -8.734944146203032389, -1.604583208406768146E-15 ) ) ;
#36447 = CARTESIAN_POINT ( 'NONE',  ( 11.04999999999991189, 12.50000000000000000, 6.148780366869520897 ) ) ;
#36448 = DIRECTION ( 'NONE',  ( 0.000000000000000000, -0.000000000000000000, 1.000000000000000000 ) ) ;
#36449 = ORIENTED_EDGE ( 'NONE', *, *, #80789, .T. ) ;
#36450 = DIRECTION ( 'NONE',  ( 0.000000000000000000, 0.000000000000000000, 1.000000000000000000 ) ) ;
#36451 = ORIENTED_EDGE ( 'NONE', *, *, #58566, .F. ) ;
#36453 = ORIENTED_EDGE ( 'NONE', *, *, #12295, .T. ) ;
#36452 = CIRCLE ( 'NONE', #1208, 0.1000000000000002554 ) ;
#36454 = DIRECTION ( 'NONE',  ( 0.000000000000000000, 0.000000000000000000, 1.000000000000000000 ) ) ;
#36455 = AXIS2_PLACEMENT_3D ( 'NONE', #83646, #101354, #52251 ) ;
#36456 = VECTOR ( 'NONE', #112293, 1000.000000000000000 ) ;
#36457 = CARTESIAN_POINT ( 'NONE',  ( 7.949999999999922018, 2.500000000000000000, -2.065063509461102065 ) ) ;
#36458 = CARTESIAN_POINT ( 'NONE',  ( 8.749999999999918288, 2.500000000000000000, -1.572243186433550211 ) ) ;
#36459 = ORIENTED_EDGE ( 'NONE', *, *, #22663, .T. ) ;
#36460 = ORIENTED_EDGE ( 'NONE', *, *, #47799, .F. ) ;
#36461 = CARTESIAN_POINT ( 'NONE',  ( 11.64999999999990798, 12.50000000000000000, 7.188010851410848723 ) ) ;
#36462 = CIRCLE ( 'NONE', #107448, 0.06509327318403745899 ) ;
#36463 = CONICAL_SURFACE ( 'NONE', #92795, 0.1000000000000002554, 0.003490658503988666988 ) ;
#36464 = VECTOR ( 'NONE', #63061, 1000.000000000000000 ) ;
#36465 = DIRECTION ( 'NONE',  ( 0.000000000000000000, 0.000000000000000000, -1.000000000000000000 ) ) ;
#36466 = CARTESIAN_POINT ( 'NONE',  ( 1.249999999999988454, 12.50000000000000000, 2.165063509461097713 ) ) ;
#36467 = ORIENTED_EDGE ( 'NONE', *, *, #63327, .T. ) ;
#36468 = ORIENTED_EDGE ( 'NONE', *, *, #57850, .F. ) ;
#36469 = DIRECTION ( 'NONE',  ( 0.000000000000000000, -0.9999939076577903929, 0.003490651415223739937 ) ) ;
#36470 = ORIENTED_EDGE ( 'NONE', *, *, #16294, .F. ) ;
#36471 = CARTESIAN_POINT ( 'NONE',  ( 8.549999999999920774, 2.500000000000000000, -2.511473670974877948 ) ) ;
#36472 = AXIS2_PLACEMENT_3D ( 'NONE', #67887, #108456, #59395 ) ;
#36473 = VECTOR ( 'NONE', #56877, 1000.000000000000000 ) ;
#36474 = AXIS2_PLACEMENT_3D ( 'NONE', #67424, #79229, #57649 ) ;
#36475 = PLANE ( 'NONE',  #88854 ) ;
#36476 = ORIENTED_EDGE ( 'NONE', *, *, #121353, .F. ) ;
#36477 = CARTESIAN_POINT ( 'NONE',  ( -0.6000000000000323963, 12.50000000000000000, -0.3464101615137759604 ) ) ;
#36478 = DIRECTION ( 'NONE',  ( 0.000000000000000000, 1.000000000000000000, 0.000000000000000000 ) ) ;
#36479 = DIRECTION ( 'NONE',  ( -0.000000000000000000, -1.000000000000000000, -0.000000000000000000 ) ) ;
#36480 = EDGE_CURVE ( 'NONE', #84566, #75902, #67773, .T. ) ;
#36481 = CARTESIAN_POINT ( 'NONE',  ( -5.600000000000020073, 12.50000000000000000, -0.3464101615137782364 ) ) ;
#36482 = ORIENTED_EDGE ( 'NONE', *, *, #54469, .F. ) ;
#36483 = EDGE_CURVE ( 'NONE', #110257, #57396, #90757, .T. ) ;
#36484 = DIRECTION ( 'NONE',  ( -4.274815082592931898E-19, -0.9999939076577903929, -0.003490651415223739937 ) ) ;
#36486 = ADVANCED_FACE ( 'NONE', ( #26900 ), #66800, .T. ) ;
#36485 = LINE ( 'NONE', #107118, #39499 ) ;
#36487 = ORIENTED_EDGE ( 'NONE', *, *, #99287, .F. ) ;
#36488 = ORIENTED_EDGE ( 'NONE', *, *, #37937, .F. ) ;
#36489 = CARTESIAN_POINT ( 'NONE',  ( 185.5052083336747444, -6.551208109652278289, 3.782341765624995134 ) ) ;
#36490 = FACE_OUTER_BOUND ( 'NONE', #72358, .T. ) ;
#36491 = DIRECTION ( 'NONE',  ( 0.000000000000000000, -0.9999939076577903929, 0.003490651415223739937 ) ) ;
#36492 = FACE_OUTER_BOUND ( 'NONE', #69605, .T. ) ;
#36493 = VECTOR ( 'NONE', #123250, 1000.000000000000000 ) ;
#36494 = CARTESIAN_POINT ( 'NONE',  ( 7.499999999999961808, 2.500000000000000000, -4.230127018922201998 ) ) ;
#36495 = EDGE_CURVE ( 'NONE', #18083, #61323, #7234, .T. ) ;
#36496 = DIRECTION ( 'NONE',  ( 0.000000000000000000, 0.000000000000000000, 1.000000000000000000 ) ) ;
#36497 = FACE_OUTER_BOUND ( 'NONE', #104976, .T. ) ;
#36498 = CARTESIAN_POINT ( 'NONE',  ( -8.750000000000012434, 12.50000000000000000, -5.802370205355744659 ) ) ;
#36499 = DIRECTION ( 'NONE',  ( 0.000000000000000000, 0.000000000000000000, -1.000000000000000000 ) ) ;
#36501 = CONICAL_SURFACE ( 'NONE', #109644, 0.1000000000000002554, 0.003490658503988666988 ) ;
#36500 = CARTESIAN_POINT ( 'NONE',  ( 14.34999999999989662, 2.500000000000000000, 2.511473670974873507 ) ) ;
#36502 = EDGE_LOOP ( 'NONE', ( #105730, #69787 ) ) ;
#36503 = CONICAL_SURFACE ( 'NONE', #32311, 0.09999999999999982514, 0.003490658503988666988 ) ;
#36504 = ORIENTED_EDGE ( 'NONE', *, *, #86080, .T. ) ;
#36505 = DIRECTION ( 'NONE',  ( -0.000000000000000000, -1.000000000000000000, -0.000000000000000000 ) ) ;
#36506 = EDGE_LOOP ( 'NONE', ( #39226, #52185 ) ) ;
#36507 = DIRECTION ( 'NONE',  ( 0.000000000000000000, 1.000000000000000000, 0.000000000000000000 ) ) ;
#36508 = DIRECTION ( 'NONE',  ( 0.000000000000000000, 1.000000000000000000, 0.000000000000000000 ) ) ;
#36509 = DIRECTION ( 'NONE',  ( 0.000000000000000000, 1.000000000000000000, 0.000000000000000000 ) ) ;
#36510 = EDGE_LOOP ( 'NONE', ( #19281, #123579 ) ) ;
#36511 = FACE_OUTER_BOUND ( 'NONE', #27255, .T. ) ;
#36512 = AXIS2_PLACEMENT_3D ( 'NONE', #87732, #127667, #8521 ) ;
#36513 = FACE_OUTER_BOUND ( 'NONE', #102155, .T. ) ;
#36515 = ORIENTED_EDGE ( 'NONE', *, *, #74204, .T. ) ;
#36514 = LINE ( 'NONE', #54830, #56417 ) ;
#36516 = DIRECTION ( 'NONE',  ( 0.000000000000000000, 0.000000000000000000, 1.000000000000000000 ) ) ;
#36517 = ORIENTED_EDGE ( 'NONE', *, *, #45709, .T. ) ;
#36518 = AXIS2_PLACEMENT_3D ( 'NONE', #1912, #21568, #70030 ) ;
#36519 = VECTOR ( 'NONE', #95962, 1000.000000000000000 ) ;
#36521 = ORIENTED_EDGE ( 'NONE', *, *, #16460, .T. ) ;
#36520 = EDGE_CURVE ( 'NONE', #58017, #92342, #32206, .T. ) ;
#36522 = VERTEX_POINT ( 'NONE', #111069 ) ;
#36523 = EDGE_LOOP ( 'NONE', ( #106441, #107156 ) ) ;
#36524 = CARTESIAN_POINT ( 'NONE',  ( 108.0000000000000142, 8.500000000000000000, -0.2500000000000000000 ) ) ;
#36525 = CONICAL_SURFACE ( 'NONE', #103320, 0.1000000000000002554, 0.003490658503988666988 ) ;
#36526 = DIRECTION ( 'NONE',  ( 0.000000000000000000, 1.000000000000000000, 0.000000000000000000 ) ) ;
#36527 = FACE_OUTER_BOUND ( 'NONE', #75274, .T. ) ;
#36528 = CIRCLE ( 'NONE', #15563, 0.1000000000000002554 ) ;
#36529 = DIRECTION ( 'NONE',  ( -0.000000000000000000, -1.000000000000000000, -0.000000000000000000 ) ) ;
#36530 = ORIENTED_EDGE ( 'NONE', *, *, #44447, .F. ) ;
#36531 = DIRECTION ( 'NONE',  ( -4.274815082592931898E-19, -0.9999939076577903929, -0.003490651415223739937 ) ) ;
#36533 = EDGE_LOOP ( 'NONE', ( #73395, #34139 ) ) ;
#36532 = ADVANCED_FACE ( 'NONE', ( #103862 ), #19662, .T. ) ;
#36534 = CARTESIAN_POINT ( 'NONE',  ( 43.06166283093421043, -3.066941195868620351, -4.904920240848436030 ) ) ;
#36535 = DIRECTION ( 'NONE',  ( 0.000000000000000000, 0.000000000000000000, 1.000000000000000000 ) ) ;
#36536 = FACE_OUTER_BOUND ( 'NONE', #11455, .T. ) ;
#36537 = CARTESIAN_POINT ( 'NONE',  ( 19.51231976789167888, -0.5900868802299801263, 4.348342248683190192 ) ) ;
#36538 = EDGE_CURVE ( 'NONE', #41232, #25471, #78263, .T. ) ;
#36539 = VERTEX_POINT ( 'NONE', #3713 ) ;
#36540 = ORIENTED_EDGE ( 'NONE', *, *, #122149, .T. ) ;
#36541 = CONICAL_SURFACE ( 'NONE', #111737, 0.1000000000000002554, 0.003490658503988666988 ) ;
#36542 = ORIENTED_EDGE ( 'NONE', *, *, #70111, .F. ) ;
#36543 = CARTESIAN_POINT ( 'NONE',  ( -5.450000000000023270, 2.500000000000000000, -2.165063509461101710 ) ) ;
#36545 = AXIS2_PLACEMENT_3D ( 'NONE', #106331, #124032, #16638 ) ;
#36544 = DIRECTION ( 'NONE',  ( -0.000000000000000000, -1.000000000000000000, -0.000000000000000000 ) ) ;
#36546 = VECTOR ( 'NONE', #68444, 1000.000000000000000 ) ;
#36547 = EDGE_CURVE ( 'NONE', #92822, #89168, #113679, .T. ) ;
#36548 = DIRECTION ( 'NONE',  ( 0.000000000000000000, -0.000000000000000000, 1.000000000000000000 ) ) ;
#36549 = FACE_BOUND ( 'NONE', #38075, .T. ) ;
#36550 = DIRECTION ( 'NONE',  ( 0.000000000000000000, 1.000000000000000000, 0.000000000000000000 ) ) ;
#36551 = FACE_OUTER_BOUND ( 'NONE', #115487, .T. ) ;
#36552 = CARTESIAN_POINT ( 'NONE',  ( 1.049999999999954081, 12.50000000000000000, -6.083687093685488989 ) ) ;
#36553 = CARTESIAN_POINT ( 'NONE',  ( -7.700000000000014388, 12.50000000000000000, -0.3464101615137782364 ) ) ;
#36554 = AXIS2_PLACEMENT_3D ( 'NONE', #74570, #26120, #114487 ) ;
#36555 = AXIS2_PLACEMENT_3D ( 'NONE', #45489, #15990, #55929 ) ;
#36556 = CARTESIAN_POINT ( 'NONE',  ( 184.9218750003414016, 0.000000000000000000, 7.564683531250000925 ) ) ;
#36557 = VECTOR ( 'NONE', #79635, 1000.000000000000000 ) ;
#36558 = DIRECTION ( 'NONE',  ( 0.000000000000000000, -0.9999939076577903929, 0.003490651415223739937 ) ) ;
#36559 = FACE_OUTER_BOUND ( 'NONE', #25541, .T. ) ;
#36560 = CIRCLE ( 'NONE', #72144, 0.06509327318403745899 ) ;
#36561 = VECTOR ( 'NONE', #40615, 1000.000000000000000 ) ;
#36562 = DIRECTION ( 'NONE',  ( 0.000000000000000000, 0.000000000000000000, 1.000000000000000000 ) ) ;
#36563 = ADVANCED_FACE ( 'NONE', ( #124132 ), #2949, .T. ) ;
#36564 = ORIENTED_EDGE ( 'NONE', *, *, #33932, .F. ) ;
#36565 = EDGE_LOOP ( 'NONE', ( #128480, #45498 ) ) ;
#36566 = ORIENTED_EDGE ( 'NONE', *, *, #2706, .T. ) ;
#36567 = ORIENTED_EDGE ( 'NONE', *, *, #124733, .T. ) ;
#36568 = AXIS2_PLACEMENT_3D ( 'NONE', #4402, #82372, #5070 ) ;
#36569 = DIRECTION ( 'NONE',  ( -0.000000000000000000, -1.000000000000000000, -0.000000000000000000 ) ) ;
#36570 = FACE_BOUND ( 'NONE', #78323, .T. ) ;
#36571 = CARTESIAN_POINT ( 'NONE',  ( -8.150000000000012790, 12.50000000000000000, -1.753560074763288679 ) ) ;
#36572 = DIRECTION ( 'NONE',  ( 0.000000000000000000, 0.000000000000000000, -1.000000000000000000 ) ) ;
#36573 = EDGE_CURVE ( 'NONE', #122182, #67250, #128444, .T. ) ;
#36574 = ORIENTED_EDGE ( 'NONE', *, *, #95360, .T. ) ;
#36575 = ADVANCED_FACE ( 'NONE', ( #4332 ), #41735, .T. ) ;
#36576 = CARTESIAN_POINT ( 'NONE',  ( 0.6499999999999561684, 2.500000000000000000, -2.511473670974877948 ) ) ;
#36577 = ADVANCED_FACE ( 'NONE', ( #1771 ), #92755, .T. ) ;
#36578 = DIRECTION ( 'NONE',  ( 0.000000000000000000, 1.000000000000000000, 0.000000000000000000 ) ) ;
#36579 = ADVANCED_FACE ( 'NONE', ( #102553 ), #54110, .T. ) ;
#36580 = EDGE_CURVE ( 'NONE', #8551, #16094, #42772, .T. ) ;
#36582 = EDGE_LOOP ( 'NONE', ( #73348, #32390, #84064, #107464 ) ) ;
#36581 = AXIS2_PLACEMENT_3D ( 'NONE', #36251, #46066, #126559 ) ;
#36583 = CARTESIAN_POINT ( 'NONE',  ( -4.800000000000024691, 12.50000000000000000, 4.611443907251934426 ) ) ;
#36584 = CARTESIAN_POINT ( 'NONE',  ( -1.850000000000033396, 2.500000000000000000, -6.841600689897077814 ) ) ;
#36585 = ADVANCED_FACE ( 'NONE', ( #21422 ), #40708, .T. ) ;
#36586 = EDGE_LOOP ( 'NONE', ( #78246, #36325 ) ) ;
#36587 = DIRECTION ( 'NONE',  ( 0.000000000000000000, 1.000000000000000000, 0.000000000000000000 ) ) ;
#36588 = EDGE_CURVE ( 'NONE', #92462, #84837, #80406, .T. ) ;
#36589 = DIRECTION ( 'NONE',  ( -4.274815082592931898E-19, -0.9999939076577903929, -0.003490651415223739937 ) ) ;
#36590 = AXIS2_PLACEMENT_3D ( 'NONE', #60701, #118961, #48950 ) ;
#36591 = EDGE_CURVE ( 'NONE', #4806, #84139, #126364, .T. ) ;
#36592 = ORIENTED_EDGE ( 'NONE', *, *, #52247, .T. ) ;
#36593 = CARTESIAN_POINT ( 'NONE',  ( -2.100000000000033396, 2.500000000000000000, -3.537306695894649966 ) ) ;
#36594 = EDGE_CURVE ( 'NONE', #89245, #91598, #57414, .T. ) ;
#36595 = CARTESIAN_POINT ( 'NONE',  ( 5.849999999999933920, 12.50000000000000000, 5.737276932171707422 ) ) ;
#36596 = ORIENTED_EDGE ( 'NONE', *, *, #6883, .T. ) ;
#36597 = DIRECTION ( 'NONE',  ( 0.000000000000000000, 0.000000000000000000, -1.000000000000000000 ) ) ;
#36598 = ORIENTED_EDGE ( 'NONE', *, *, #9699, .F. ) ;
#36599 = ORIENTED_EDGE ( 'NONE', *, *, #6268, .F. ) ;
#36600 = ADVANCED_FACE ( 'NONE', ( #91452 ), #38653, .T. ) ;
#36601 = CARTESIAN_POINT ( 'NONE',  ( 6.899999999999926636, 2.500000000000000000, -0.3464101615137782364 ) ) ;
#36602 = EDGE_CURVE ( 'NONE', #88265, #93018, #83584, .T. ) ;
#36603 = EDGE_LOOP ( 'NONE', ( #123187, #101783, #21429, #71995 ) ) ;
#36604 = DIRECTION ( 'NONE',  ( 0.000000000000000000, 0.000000000000000000, -1.000000000000000000 ) ) ;
#36605 = CARTESIAN_POINT ( 'NONE',  ( -2.050000000000033129, 2.500000000000000000, 2.065063509461097624 ) ) ;
#36606 = VECTOR ( 'NONE', #30901, 1000.000000000000000 ) ;
#36607 = ORIENTED_EDGE ( 'NONE', *, *, #60109, .F. ) ;
#36608 = DIRECTION ( 'NONE',  ( -0.000000000000000000, 1.000000000000000000, -0.000000000000000000 ) ) ;
#36609 = FACE_OUTER_BOUND ( 'NONE', #64717, .T. ) ;
#36610 = DIRECTION ( 'NONE',  ( 0.000000000000000000, 1.000000000000000000, 0.000000000000000000 ) ) ;
#36611 = CARTESIAN_POINT ( 'NONE',  ( -6.650000000000014566, 2.500000000000000000, 2.065063509461097624 ) ) ;
#36612 = DIRECTION ( 'NONE',  ( 0.000000000000000000, 1.000000000000000000, 0.000000000000000000 ) ) ;
#36613 = DIRECTION ( 'NONE',  ( 0.000000000000000000, 0.000000000000000000, 1.000000000000000000 ) ) ;
#36614 = ORIENTED_EDGE ( 'NONE', *, *, #110015, .T. ) ;
#36615 = ORIENTED_EDGE ( 'NONE', *, *, #39849, .F. ) ;
#36616 = FACE_OUTER_BOUND ( 'NONE', #39133, .T. ) ;
#36617 = AXIS2_PLACEMENT_3D ( 'NONE', #90628, #59263, #99175 ) ;
#36618 = DIRECTION ( 'NONE',  ( -4.274815082592931898E-19, -0.9999939076577903929, -0.003490651415223739937 ) ) ;
#36619 = DIRECTION ( 'NONE',  ( 0.000000000000000000, 0.000000000000000000, 1.000000000000000000 ) ) ;
#36621 = ORIENTED_EDGE ( 'NONE', *, *, #8218, .T. ) ;
#36620 = EDGE_LOOP ( 'NONE', ( #17534, #429, #21031, #86754 ) ) ;
#36622 = ORIENTED_EDGE ( 'NONE', *, *, #114309, .F. ) ;
#36623 = CARTESIAN_POINT ( 'NONE',  ( -5.600000000000023626, 2.500000000000000000, -3.983716857408426293 ) ) ;
#36624 = CARTESIAN_POINT ( 'NONE',  ( 4.399999999999940847, 2.500000000000000000, -4.676537180435977881 ) ) ;
#36625 = DIRECTION ( 'NONE',  ( 0.000000000000000000, 0.000000000000000000, 1.000000000000000000 ) ) ;
#36626 = APPLICATION_PROTOCOL_DEFINITION ( 'draft international standard', 'automotive_design', 1998, #56335 ) ;
#36627 = CARTESIAN_POINT ( 'NONE',  ( -9.350000000000006750, 2.500000000000000000, -2.511473670974877948 ) ) ;
#36628 = LINE ( 'NONE', #37264, #56470 ) ;
#36629 = DIRECTION ( 'NONE',  ( 0.000000000000000000, 1.000000000000000000, 0.000000000000000000 ) ) ;
#36630 = CARTESIAN_POINT ( 'NONE',  ( 1.249999999999953815, 12.50000000000000000, 1.407149913249508000 ) ) ;
#36631 = DIRECTION ( 'NONE',  ( -0.000000000000000000, -1.000000000000000000, -0.000000000000000000 ) ) ;
#36632 = CIRCLE ( 'NONE', #74270, 0.1000000000000002554 ) ;
#36633 = DIRECTION ( 'NONE',  ( 0.000000000000000000, 0.000000000000000000, -1.000000000000000000 ) ) ;
#36634 = ORIENTED_EDGE ( 'NONE', *, *, #67973, .F. ) ;
#36635 = EDGE_CURVE ( 'NONE', #53209, #41131, #23960, .T. ) ;
#36636 = AXIS2_PLACEMENT_3D ( 'NONE', #40276, #90653, #29808 ) ;
#36637 = CIRCLE ( 'NONE', #82696, 0.1000000000000002554 ) ;
#36638 = ADVANCED_FACE ( 'NONE', ( #35761 ), #74141, .T. ) ;
#36639 = CARTESIAN_POINT ( 'NONE',  ( 4.149999999999939959, 2.500000000000000000, 1.472243186433545459 ) ) ;
#36640 = CIRCLE ( 'NONE', #28305, 0.09999999999999982514 ) ;
#36641 = VERTEX_POINT ( 'NONE', #45589 ) ;
#36642 = ORIENTED_EDGE ( 'NONE', *, *, #29798, .T. ) ;
#36643 = CARTESIAN_POINT ( 'NONE',  ( -0.6000000000000388356, 2.500000000000000000, 4.676537180435972552 ) ) ;
#36644 = DIRECTION ( 'NONE',  ( -4.274815082592931898E-19, -0.9999939076577903929, -0.003490651415223739937 ) ) ;
#36645 = DIRECTION ( 'NONE',  ( 0.000000000000000000, 1.000000000000000000, 0.000000000000000000 ) ) ;
#36646 = CIRCLE ( 'NONE', #120159, 0.09999999999999982514 ) ;
#36647 = FACE_OUTER_BOUND ( 'NONE', #24847, .T. ) ;
#36648 = AXIS2_PLACEMENT_3D ( 'NONE', #3110, #32588, #92112 ) ;
#36649 = CARTESIAN_POINT ( 'NONE',  ( 185.0000000000000000, 0.000000000000000000, 7.700000000000000178 ) ) ;
#36650 = FACE_OUTER_BOUND ( 'NONE', #84029, .T. ) ;
#36651 = CARTESIAN_POINT ( 'NONE',  ( -4.600000000000025402, 2.500000000000000000, -0.1000000000000023925 ) ) ;
#36652 = ORIENTED_EDGE ( 'NONE', *, *, #118124, .T. ) ;
#36653 = DIRECTION ( 'NONE',  ( -0.000000000000000000, 1.000000000000000000, -0.000000000000000000 ) ) ;
#36654 = AXIS2_PLACEMENT_3D ( 'NONE', #67876, #96677, #116967 ) ;
#36655 = DIRECTION ( 'NONE',  ( 0.000000000000000000, 1.000000000000000000, 0.000000000000000000 ) ) ;
#36657 = EDGE_LOOP ( 'NONE', ( #7278, #113874, #110452, #115694 ) ) ;
#36656 = CIRCLE ( 'NONE', #126522, 0.1000000000000002554 ) ;
#36658 = AXIS2_PLACEMENT_3D ( 'NONE', #40938, #56816, #40274 ) ;
#36659 = EDGE_LOOP ( 'NONE', ( #34942, #98969 ) ) ;
#36660 = ORIENTED_EDGE ( 'NONE', *, *, #69446, .T. ) ;
#36661 = VERTEX_POINT ( 'NONE', #6910 ) ;
#36662 = VERTEX_POINT ( 'NONE', #56029 ) ;
#36663 = PLANE ( 'NONE',  #77580 ) ;
#36664 = PLANE ( 'NONE',  #28965 ) ;
#36665 = ORIENTED_EDGE ( 'NONE', *, *, #2797, .T. ) ;
#36666 = CARTESIAN_POINT ( 'NONE',  ( -9.400000000000009237, 2.500000000000000000, -4.776537180435973973 ) ) ;
#36667 = DIRECTION ( 'NONE',  ( -4.274815082592931898E-19, -0.9999939076577903929, -0.003490651415223739937 ) ) ;
#36668 = CARTESIAN_POINT ( 'NONE',  ( -10.40000000000000213, 12.50000000000000000, -2.276824562219559311E-15 ) ) ;
#36669 = ORIENTED_EDGE ( 'NONE', *, *, #11639, .F. ) ;
#36670 = FACE_OUTER_BOUND ( 'NONE', #113950, .T. ) ;
#36671 = AXIS2_PLACEMENT_3D ( 'NONE', #127050, #104799, #105470 ) ;
#36672 = CARTESIAN_POINT ( 'NONE',  ( 4.999999999999935163, 2.500000000000000000, 0.7928203230275495672 ) ) ;
#36673 = EDGE_CURVE ( 'NONE', #92388, #31556, #14792, .T. ) ;
#36674 = ORIENTED_EDGE ( 'NONE', *, *, #83785, .T. ) ;
#36675 = ORIENTED_EDGE ( 'NONE', *, *, #31422, .F. ) ;
#36676 = EDGE_LOOP ( 'NONE', ( #28514, #72336 ) ) ;
#36677 = DIRECTION ( 'NONE',  ( 0.000000000000000000, 0.000000000000000000, -1.000000000000000000 ) ) ;
#36678 = CONICAL_SURFACE ( 'NONE', #63854, 0.1000000000000002554, 0.003490658503988666988 ) ;
#36679 = CONICAL_SURFACE ( 'NONE', #109822, 0.1000000000000000472, 0.003490658503988666988 ) ;
#36680 = DIRECTION ( 'NONE',  ( 0.000000000000000000, 0.000000000000000000, 1.000000000000000000 ) ) ;
#36682 = VERTEX_POINT ( 'NONE', #46877 ) ;
#36681 = EDGE_CURVE ( 'NONE', #109041, #118850, #64329, .T. ) ;
#36683 = CARTESIAN_POINT ( 'NONE',  ( 12.04999999999990479, 12.50000000000000000, 2.230156782645134950 ) ) ;
#36684 = CARTESIAN_POINT ( 'NONE',  ( 0.3999999999999555023, 2.500000000000000000, 4.330127018922196314 ) ) ;
#36685 = CARTESIAN_POINT ( 'NONE',  ( -5.800000000000018474, 2.500000000000000000, 4.330127018922196314 ) ) ;
#36686 = DIRECTION ( 'NONE',  ( 0.000000000000000000, 0.000000000000000000, 1.000000000000000000 ) ) ;
#36687 = EDGE_CURVE ( 'NONE', #82798, #75397, #67863, .T. ) ;
#36688 = CIRCLE ( 'NONE', #84697, 0.06509327318403745899 ) ;
#36689 = ORIENTED_EDGE ( 'NONE', *, *, #109582, .F. ) ;
#36690 = DIRECTION ( 'NONE',  ( 0.000000000000000000, -0.000000000000000000, 1.000000000000000000 ) ) ;
#36691 = AXIS2_PLACEMENT_3D ( 'NONE', #67264, #107228, #17548 ) ;
#36692 = ORIENTED_EDGE ( 'NONE', *, *, #101131, .T. ) ;
#36693 = EDGE_LOOP ( 'NONE', ( #58638, #7277, #76172, #51177 ) ) ;
#36694 = VERTEX_POINT ( 'NONE', #25946 ) ;
#36695 = ADVANCED_FACE ( 'NONE', ( #75665 ), #26023, .T. ) ;
#36696 = CARTESIAN_POINT ( 'NONE',  ( -3.300000000000027800, 2.500000000000000000, -4.230127018922201998 ) ) ;
#36697 = FACE_BOUND ( 'NONE', #122090, .T. ) ;
#36698 = CARTESIAN_POINT ( 'NONE',  ( 186.2812500006828031, 0.000000000000000000, 7.700000000000000178 ) ) ;
#36699 = CARTESIAN_POINT ( 'NONE',  ( 1.849999999999949685, 12.50000000000000000, 1.753560074763284016 ) ) ;
#36700 = CARTESIAN_POINT ( 'NONE',  ( -3.350000000000028955, 2.500000000000000000, -2.265063509461101798 ) ) ;
#36701 = CONICAL_SURFACE ( 'NONE', #112004, 0.09999999999999982514, 0.003490658503988666988 ) ;
#36702 = CONICAL_SURFACE ( 'NONE', #124529, 0.1000000000000000472, 0.003490658503988666988 ) ;
#36703 = EDGE_LOOP ( 'NONE', ( #90753, #41753, #79156, #65612 ) ) ;
#36704 = PLANE ( 'NONE',  #48105 ) ;
#36705 = CARTESIAN_POINT ( 'NONE',  ( 6.249999999999932498, 12.50000000000000000, -2.857883832488653741 ) ) ;
#36706 = CARTESIAN_POINT ( 'NONE',  ( 7.899999999999923084, 2.500000000000000000, 0.7928203230275495672 ) ) ;
#36707 = CARTESIAN_POINT ( 'NONE',  ( 4.149999999999939959, 2.500000000000000000, -2.165063509461101710 ) ) ;
#36708 = EDGE_LOOP ( 'NONE', ( #94960, #68030 ) ) ;
#36709 = CARTESIAN_POINT ( 'NONE',  ( -6.250000000000017764, 2.500000000000000000, 2.757883832488649656 ) ) ;
#36710 = DIRECTION ( 'NONE',  ( 0.000000000000000000, 0.000000000000000000, 1.000000000000000000 ) ) ;
#36711 = CONICAL_SURFACE ( 'NONE', #126590, 0.1000000000000002554, 0.003490658503988666988 ) ;
#36712 = EDGE_LOOP ( 'NONE', ( #2304, #44984 ) ) ;
#36713 = LINE ( 'NONE', #87074, #43922 ) ;
#36714 = CARTESIAN_POINT ( 'NONE',  ( -10.85000000000000142, 12.50000000000000000, -1.472243186433546125 ) ) ;
#36715 = FACE_BOUND ( 'NONE', #40382, .T. ) ;
#36716 = LINE ( 'NONE', #58288, #45180 ) ;
#36717 = EDGE_CURVE ( 'NONE', #96763, #52365, #21916, .T. ) ;
#36718 = CONICAL_SURFACE ( 'NONE', #11662, 0.1000000000000002554, 0.003490658503988666988 ) ;
#36719 = ORIENTED_EDGE ( 'NONE', *, *, #65041, .T. ) ;
#36720 = CARTESIAN_POINT ( 'NONE',  ( -0.4000000000000392131, 2.500000000000000000, -4.430127018922202176 ) ) ;
#36721 = DIRECTION ( 'NONE',  ( -0.000000000000000000, -1.000000000000000000, -0.000000000000000000 ) ) ;
#36722 = CIRCLE ( 'NONE', #51402, 0.06509327318403745899 ) ;
#36723 = ORIENTED_EDGE ( 'NONE', *, *, #115878, .T. ) ;
#36724 = VERTEX_POINT ( 'NONE', #75042 ) ;
#36725 = EDGE_CURVE ( 'NONE', #31609, #22180, #90856, .T. ) ;
#36726 = CARTESIAN_POINT ( 'NONE',  ( 186.7916666666666572, 4.445597072760120838, -7.699999999999998401 ) ) ;
#36727 = ADVANCED_FACE ( 'NONE', ( #125429 ), #3035, .T. ) ;
#36728 = ORIENTED_EDGE ( 'NONE', *, *, #72215, .T. ) ;
#36729 = CARTESIAN_POINT ( 'NONE',  ( 185.2135416670080588, 4.367472073101518859, -7.564683531249999149 ) ) ;
#36730 = CARTESIAN_POINT ( 'NONE',  ( 8.149999999999923972, 2.500000000000000000, 2.611473670974873151 ) ) ;
#36731 = DIRECTION ( 'NONE',  ( 0.000000000000000000, 0.000000000000000000, 1.000000000000000000 ) ) ;
#36732 = EDGE_CURVE ( 'NONE', #46460, #42124, #78352, .T. ) ;
#36733 = ADVANCED_FACE ( 'NONE', ( #57333 ), #116875, .T. ) ;
#36734 = DIRECTION ( 'NONE',  ( -0.000000000000000000, -1.000000000000000000, -0.000000000000000000 ) ) ;
#36735 = ADVANCED_FACE ( 'NONE', ( #66495 ), #34491, .T. ) ;
#36736 = CIRCLE ( 'NONE', #70178, 0.06509327318403745899 ) ;
#36737 = VECTOR ( 'NONE', #30955, 1000.000000000000000 ) ;
#36738 = ORIENTED_EDGE ( 'NONE', *, *, #32968, .T. ) ;
#36739 = CIRCLE ( 'NONE', #63917, 0.1000000000000000056 ) ;
#36740 = DIRECTION ( 'NONE',  ( 0.000000000000000000, 0.000000000000000000, 1.000000000000000000 ) ) ;
#36741 = ADVANCED_FACE ( 'NONE', ( #96589 ), #86782, .T. ) ;
#36742 = CARTESIAN_POINT ( 'NONE',  ( 12.04999999999990479, 12.50000000000000000, -6.560283801567339701 ) ) ;
#36743 = CARTESIAN_POINT ( 'NONE',  ( -4.800000000000026468, 2.500000000000000000, -4.776537180435978414 ) ) ;
#36744 = AXIS2_PLACEMENT_3D ( 'NONE', #75921, #24252, #34740 ) ;
#36745 = LINE ( 'NONE', #68109, #107323 ) ;
#36746 = VERTEX_POINT ( 'NONE', #107059 ) ;
#36747 = DIRECTION ( 'NONE',  ( 0.000000000000000000, 1.000000000000000000, 0.000000000000000000 ) ) ;
#36748 = ORIENTED_EDGE ( 'NONE', *, *, #89628, .F. ) ;
#36749 = DIRECTION ( 'NONE',  ( 0.000000000000000000, 1.000000000000000000, 0.000000000000000000 ) ) ;
#36750 = CARTESIAN_POINT ( 'NONE',  ( 1.649999999999951505, 2.500000000000000000, 2.757883832488649656 ) ) ;
#36751 = EDGE_CURVE ( 'NONE', #48843, #38503, #92925, .T. ) ;
#36752 = ORIENTED_EDGE ( 'NONE', *, *, #126846, .F. ) ;
#36753 = PLANE ( 'NONE',  #38909 ) ;
#36754 = CARTESIAN_POINT ( 'NONE',  ( 87.49999999999998579, -4.871203238224193655, -5.733266569811711122 ) ) ;
#36755 = DIRECTION ( 'NONE',  ( -4.274815082592931898E-19, -0.9999939076577903929, -0.003490651415223739937 ) ) ;
#36756 = CARTESIAN_POINT ( 'NONE',  ( -11.84999999999999609, 2.500000000000000000, 6.941600689897073018 ) ) ;
#36757 = ORIENTED_EDGE ( 'NONE', *, *, #126600, .T. ) ;
#36758 = DIRECTION ( 'NONE',  ( 0.000000000000000000, 0.000000000000000000, -1.000000000000000000 ) ) ;
#36759 = DIRECTION ( 'NONE',  ( -4.274815082592931898E-19, -0.9999939076577903929, -0.003490651415223739937 ) ) ;
#36760 = CARTESIAN_POINT ( 'NONE',  ( 187.0260416670080588, -6.551208109652273848, -3.782341765625003571 ) ) ;
#36761 = DIRECTION ( 'NONE',  ( -0.000000000000000000, -1.000000000000000000, -0.000000000000000000 ) ) ;
#36762 = VECTOR ( 'NONE', #29489, 1000.000000000000000 ) ;
#36763 = PLANE ( 'NONE',  #116292 ) ;
#36764 = ORIENTED_EDGE ( 'NONE', *, *, #88281, .F. ) ;
#36765 = ORIENTED_EDGE ( 'NONE', *, *, #73106, .T. ) ;
#36766 = CARTESIAN_POINT ( 'NONE',  ( -13.34999999999999076, 12.50000000000000000, 1.472243186433549456 ) ) ;
#36767 = ORIENTED_EDGE ( 'NONE', *, *, #75759, .T. ) ;
#36768 = CARTESIAN_POINT ( 'NONE',  ( 2.499999999999947153, 12.50000000000000000, -3.637306695894650055 ) ) ;
#36770 = VERTEX_POINT ( 'NONE', #87424 ) ;
#36769 = ORIENTED_EDGE ( 'NONE', *, *, #49020, .T. ) ;
#36771 = CIRCLE ( 'NONE', #61903, 0.1000000000000002554 ) ;
#36772 = VERTEX_POINT ( 'NONE', #114317 ) ;
#36773 = DIRECTION ( 'NONE',  ( -0.000000000000000000, -1.000000000000000000, -0.000000000000000000 ) ) ;
#36774 = AXIS2_PLACEMENT_3D ( 'NONE', #110122, #47991, #129148 ) ;
#36775 = VECTOR ( 'NONE', #5461, 1000.000000000000000 ) ;
#36776 = CARTESIAN_POINT ( 'NONE',  ( 13.74999999999989697, 2.500000000000000000, 2.957883832488649389 ) ) ;
#36777 = CARTESIAN_POINT ( 'NONE',  ( -3.749999999999994671, 2.500000000000000000, -6.395190528383301931 ) ) ;
#36778 = CIRCLE ( 'NONE', #126649, 0.1000000000000000472 ) ;
#36779 = DIRECTION ( 'NONE',  ( 0.000000000000000000, 1.000000000000000000, 0.000000000000000000 ) ) ;
#36780 = DIRECTION ( 'NONE',  ( -0.000000000000000000, 1.000000000000000000, -0.000000000000000000 ) ) ;
#36781 = CARTESIAN_POINT ( 'NONE',  ( 9.999999999999911182, 12.50000000000000000, -3.637306695894650055 ) ) ;
#36782 = ORIENTED_EDGE ( 'NONE', *, *, #113737, .T. ) ;
#36783 = DIRECTION ( 'NONE',  ( 0.000000000000000000, 1.000000000000000000, 0.000000000000000000 ) ) ;
#36784 = ORIENTED_EDGE ( 'NONE', *, *, #39977, .F. ) ;
#36785 = AXIS2_PLACEMENT_3D ( 'NONE', #63415, #84340, #122347 ) ;
#36786 = VERTEX_POINT ( 'NONE', #24654 ) ;
#36787 = ORIENTED_EDGE ( 'NONE', *, *, #43414, .T. ) ;
#36788 = ADVANCED_FACE ( 'NONE', ( #37699 ), #36501, .T. ) ;
#36789 = ORIENTED_EDGE ( 'NONE', *, *, #91351, .F. ) ;
#36790 = CIRCLE ( 'NONE', #34739, 0.06509327318403745899 ) ;
#36791 = CARTESIAN_POINT ( 'NONE',  ( -7.900000000000014566, 12.50000000000000000, -2.276824562219559311E-15 ) ) ;
#36792 = VERTEX_POINT ( 'NONE', #20644 ) ;
#36793 = ORIENTED_EDGE ( 'NONE', *, *, #34539, .T. ) ;
#36794 = ADVANCED_FACE ( 'NONE', ( #9525 ), #72090, .T. ) ;
#36795 = AXIS2_PLACEMENT_3D ( 'NONE', #60246, #18358, #39948 ) ;
#36796 = CARTESIAN_POINT ( 'NONE',  ( 4.199999999999941558, 12.50000000000000000, -4.330127018922201643 ) ) ;
#36797 = DIRECTION ( 'NONE',  ( 0.000000000000000000, 0.000000000000000000, 1.000000000000000000 ) ) ;
#36798 = CARTESIAN_POINT ( 'NONE',  ( -9.150000000000009237, 2.500000000000000000, -1.372243186433550033 ) ) ;
#36799 = DIRECTION ( 'NONE',  ( 0.000000000000000000, 0.000000000000000000, 1.000000000000000000 ) ) ;
#36800 = ORIENTED_EDGE ( 'NONE', *, *, #33082, .F. ) ;
#36801 = CARTESIAN_POINT ( 'NONE',  ( 7.099999999999926814, 12.50000000000000000, -0.6928203230275541413 ) ) ;
#36802 = ORIENTED_EDGE ( 'NONE', *, *, #78593, .F. ) ;
#36803 = LINE ( 'NONE', #96335, #31725 ) ;
#36804 = ORIENTED_EDGE ( 'NONE', *, *, #34101, .F. ) ;
#36805 = LINE ( 'NONE', #127749, #113156 ) ;
#36806 = EDGE_LOOP ( 'NONE', ( #3578, #86017, #108697, #31705 ) ) ;
#36807 = ORIENTED_EDGE ( 'NONE', *, *, #110312, .F. ) ;
#36808 = CARTESIAN_POINT ( 'NONE',  ( -4.150000000000024336, 12.50000000000000000, 2.165063509461097713 ) ) ;
#36809 = DIRECTION ( 'NONE',  ( 0.000000000000000000, -0.000000000000000000, 1.000000000000000000 ) ) ;
#36810 = CIRCLE ( 'NONE', #109965, 0.1000000000000000472 ) ;
#36811 = CARTESIAN_POINT ( 'NONE',  ( 11.64999999999990443, 12.50000000000000000, -5.737276932171712751 ) ) ;
#36813 = DIRECTION ( 'NONE',  ( 0.000000000000000000, -0.000000000000000000, 1.000000000000000000 ) ) ;
#36812 = AXIS2_PLACEMENT_3D ( 'NONE', #60335, #82543, #100247 ) ;
#36814 = CARTESIAN_POINT ( 'NONE',  ( 21.24754738303276724, -0.7337760880902383098, -4.182111650399352953 ) ) ;
#36815 = ORIENTED_EDGE ( 'NONE', *, *, #116805, .T. ) ;
#36816 =( BOUNDED_CURVE ( )  B_SPLINE_CURVE ( 2, ( #12495, #11847, #52421, #33449, #82545, #115849, #75924 ),
 .UNSPECIFIED., .F., .F. ) 
 B_SPLINE_CURVE_WITH_KNOTS ( ( 3, 2, 2, 3 ),
 ( 0.000000000000000000, 0.02380952380952383249, 0.04761904761904766498, 0.07142857142857149400 ),
 .UNSPECIFIED. ) 
 CURVE ( )  GEOMETRIC_REPRESENTATION_ITEM ( )  RATIONAL_B_SPLINE_CURVE ( ( 1.000000000000000000, 0.8660254037844387076, 1.000000000000000000, 0.8660254037844387076, 1.000000000000000000, 0.8660254037844383745, 1.000000000000000444 ) ) 
 REPRESENTATION_ITEM ( '' )  );
#36817 = DIRECTION ( 'NONE',  ( -0.000000000000000000, -1.000000000000000000, -0.000000000000000000 ) ) ;
#36818 = LINE ( 'NONE', #76729, #82806 ) ;
#36819 = CARTESIAN_POINT ( 'NONE',  ( -10.84999999999999964, 2.500000000000000000, 5.902370205355745192 ) ) ;
#36820 = CARTESIAN_POINT ( 'NONE',  ( -3.550000000000031797, 12.50000000000000000, -6.148780366869526226 ) ) ;
#36821 = AXIS2_PLACEMENT_3D ( 'NONE', #17530, #57479, #18178 ) ;
#36822 = DIRECTION ( 'NONE',  ( -4.274815082592931898E-19, -0.9999939076577903929, -0.003490651415223739937 ) ) ;
#36823 = ADVANCED_FACE ( 'NONE', ( #29180 ), #101331, .T. ) ;
#36824 = ORIENTED_EDGE ( 'NONE', *, *, #97425, .T. ) ;
#36825 = ORIENTED_EDGE ( 'NONE', *, *, #95348, .T. ) ;
#36826 = FACE_OUTER_BOUND ( 'NONE', #76767, .T. ) ;
#36827 = ORIENTED_EDGE ( 'NONE', *, *, #35690, .T. ) ;
#36828 = AXIS2_PLACEMENT_3D ( 'NONE', #97010, #55800, #87818 ) ;
#36829 = DIRECTION ( 'NONE',  ( -0.000000000000000000, 1.000000000000000000, -0.000000000000000000 ) ) ;
#36831 = ADVANCED_FACE ( 'NONE', ( #10778 ), #51161, .T. ) ;
#36830 = CARTESIAN_POINT ( 'NONE',  ( -6.050000000000020250, 2.500000000000000000, -2.511473670974877948 ) ) ;
#36833 = ORIENTED_EDGE ( 'NONE', *, *, #26084, .F. ) ;
#36832 = EDGE_CURVE ( 'NONE', #93842, #18830, #107588, .T. ) ;
#36834 = CARTESIAN_POINT ( 'NONE',  ( 186.5416666666666856, -4.445597072760122614, 7.699999999999998401 ) ) ;
#36835 = DIRECTION ( 'NONE',  ( 0.000000000000000000, -0.9999939076577903929, 0.003490651415223739937 ) ) ;
#36836 = CARTESIAN_POINT ( 'NONE',  ( -6.249999999999984901, 2.500000000000000000, -6.495190528383302464 ) ) ;
#36837 = CARTESIAN_POINT ( 'NONE',  ( -1.650000000000035660, 2.500000000000000000, 2.757883832488649656 ) ) ;
#36838 = EDGE_CURVE ( 'NONE', #39278, #111575, #18037, .T. ) ;
#36839 = CARTESIAN_POINT ( 'NONE',  ( -1.850000000000033396, 2.500000000000000000, -6.148780366869526226 ) ) ;
#36840 = ORIENTED_EDGE ( 'NONE', *, *, #4456, .F. ) ;
#36841 = CARTESIAN_POINT ( 'NONE',  ( -10.65000000000000391, 2.500000000000000000, -6.841600689897075149 ) ) ;
#36842 = DIRECTION ( 'NONE',  ( 0.000000000000000000, -0.9999939076577903929, 0.003490651415223739937 ) ) ;
#36843 = ADVANCED_FACE ( 'NONE', ( #8855 ), #57988, .T. ) ;
#36844 = ORIENTED_EDGE ( 'NONE', *, *, #84750, .F. ) ;
#36845 = EDGE_CURVE ( 'NONE', #50744, #79454, #32399, .T. ) ;
#36846 = FACE_OUTER_BOUND ( 'NONE', #21386, .T. ) ;
#36847 = AXIS2_PLACEMENT_3D ( 'NONE', #52838, #81647, #92774 ) ;
#36848 = CARTESIAN_POINT ( 'NONE',  ( -1.650000000000035660, 2.500000000000000000, 2.857883832488649301 ) ) ;
#36849 = DIRECTION ( 'NONE',  ( 0.000000000000000000, 0.000000000000000000, 1.000000000000000000 ) ) ;
#36850 = ORIENTED_EDGE ( 'NONE', *, *, #74047, .F. ) ;
#36851 = VECTOR ( 'NONE', #88278, 1000.000000000000000 ) ;
#36852 = CARTESIAN_POINT ( 'NONE',  ( 9.349999999999919709, 2.500000000000000000, 2.511473670974873507 ) ) ;
#36853 = CIRCLE ( 'NONE', #120468, 0.1000000000000002554 ) ;
#36854 = ORIENTED_EDGE ( 'NONE', *, *, #49126, .T. ) ;
#36855 = DIRECTION ( 'NONE',  ( 0.000000000000000000, 1.000000000000000000, 0.000000000000000000 ) ) ;
#36856 = DIRECTION ( 'NONE',  ( -0.000000000000000000, -1.000000000000000000, -0.000000000000000000 ) ) ;
#36857 = CARTESIAN_POINT ( 'NONE',  ( 13.09999999999990195, 2.500000000000000000, -4.676537180435978769 ) ) ;
#36858 = CIRCLE ( 'NONE', #34810, 0.1000000000000002554 ) ;
#36859 = ORIENTED_EDGE ( 'NONE', *, *, #66676, .F. ) ;
#36860 = CARTESIAN_POINT ( 'NONE',  ( -7.300000000000014921, 2.500000000000000000, 4.676537180435972552 ) ) ;
#36861 = AXIS2_PLACEMENT_3D ( 'NONE', #16238, #56175, #96107 ) ;
#36862 = CARTESIAN_POINT ( 'NONE',  ( 186.7500000000000000, 9.429780353434619030E-16, -7.700000000000000178 ) ) ;
#36863 = EDGE_LOOP ( 'NONE', ( #74409, #120241 ) ) ;
#36864 = EDGE_LOOP ( 'NONE', ( #44972, #17199 ) ) ;
#36866 = CIRCLE ( 'NONE', #78647, 0.06509327318403741736 ) ;
#36865 = DIRECTION ( 'NONE',  ( 0.000000000000000000, 0.000000000000000000, 1.000000000000000000 ) ) ;
#36868 = CONICAL_SURFACE ( 'NONE', #110032, 0.1000000000000002554, 0.003490658503988666988 ) ;
#36867 = CIRCLE ( 'NONE', #34831, 0.06509327318403745899 ) ;
#36869 = VERTEX_POINT ( 'NONE', #118828 ) ;
#36870 = DIRECTION ( 'NONE',  ( 0.000000000000000000, 0.000000000000000000, 1.000000000000000000 ) ) ;
#36871 = DIRECTION ( 'NONE',  ( 0.000000000000000000, 0.000000000000000000, -1.000000000000000000 ) ) ;
#36872 = ORIENTED_EDGE ( 'NONE', *, *, #62137, .F. ) ;
#36873 = ORIENTED_EDGE ( 'NONE', *, *, #73166, .T. ) ;
#36874 = DIRECTION ( 'NONE',  ( 0.000000000000000000, 1.000000000000000000, 0.000000000000000000 ) ) ;
#36875 = DIRECTION ( 'NONE',  ( -0.000000000000000000, 1.000000000000000000, -0.000000000000000000 ) ) ;
#36876 = ORIENTED_EDGE ( 'NONE', *, *, #64156, .F. ) ;
#36877 = EDGE_CURVE ( 'NONE', #49835, #32336, #122263, .T. ) ;
#36878 = CARTESIAN_POINT ( 'NONE',  ( 13.14999999999990088, 2.500000000000000000, 2.611473670974873151 ) ) ;
#36879 = DIRECTION ( 'NONE',  ( -4.274815082592931898E-19, -0.9999939076577903929, -0.003490651415223739937 ) ) ;
#36880 = CARTESIAN_POINT ( 'NONE',  ( -3.750000000000026201, 2.500000000000000000, 5.902370205355745192 ) ) ;
#36881 = DIRECTION ( 'NONE',  ( 0.000000000000000000, -0.9999939076577903929, 0.003490651415223739937 ) ) ;
#36882 = ADVANCED_FACE ( 'NONE', ( #48817 ), #1058, .T. ) ;
#36883 = CARTESIAN_POINT ( 'NONE',  ( 1.849999999999948130, 2.500000000000000000, 6.148780366869520009 ) ) ;
#36884 = DIRECTION ( 'NONE',  ( -0.000000000000000000, 1.000000000000000000, -0.000000000000000000 ) ) ;
#36885 = EDGE_CURVE ( 'NONE', #118223, #67418, #38351, .T. ) ;
#36886 = EDGE_CURVE ( 'NONE', #3107, #75929, #108360, .T. ) ;
#36887 = ORIENTED_EDGE ( 'NONE', *, *, #58968, .T. ) ;
#36888 = VERTEX_POINT ( 'NONE', #50735 ) ;
#36890 = ORIENTED_EDGE ( 'NONE', *, *, #8523, .F. ) ;
#36889 = EDGE_CURVE ( 'NONE', #34079, #29998, #107675, .T. ) ;
#36891 = EDGE_LOOP ( 'NONE', ( #113849, #79687 ) ) ;
#36892 = DIRECTION ( 'NONE',  ( 0.000000000000000000, 0.000000000000000000, 1.000000000000000000 ) ) ;
#36893 = CARTESIAN_POINT ( 'NONE',  ( -6.050000000000018474, 12.50000000000000000, 6.841600689897072485 ) ) ;
#36894 = CARTESIAN_POINT ( 'NONE',  ( -7.900000000000014566, 2.500000000000000000, -0.7928203230275542301 ) ) ;
#36895 = ORIENTED_EDGE ( 'NONE', *, *, #77345, .F. ) ;
#36896 = FACE_BOUND ( 'NONE', #38851, .T. ) ;
#36897 = FACE_OUTER_BOUND ( 'NONE', #16738, .T. ) ;
#36898 = DIRECTION ( 'NONE',  ( 0.000000000000000000, 1.000000000000000000, 0.000000000000000000 ) ) ;
#36899 = EDGE_CURVE ( 'NONE', #45123, #117938, #124403, .T. ) ;
#36900 = PLANE ( 'NONE',  #43016 ) ;
#36901 = EDGE_CURVE ( 'NONE', #44118, #3657, #65898, .T. ) ;
#36902 = VECTOR ( 'NONE', #24836, 1000.000000000000000 ) ;
#36903 = PLANE ( 'NONE',  #99296 ) ;
#36904 = VECTOR ( 'NONE', #32662, 1000.000000000000000 ) ;
#36905 = DIRECTION ( 'NONE',  ( 0.000000000000000000, 0.000000000000000000, -1.000000000000000000 ) ) ;
#36906 = DIRECTION ( 'NONE',  ( -0.000000000000000000, 1.000000000000000000, -0.000000000000000000 ) ) ;
#36907 = DIRECTION ( 'NONE',  ( 0.000000000000000000, 0.000000000000000000, -1.000000000000000000 ) ) ;
#36908 = LINE ( 'NONE', #108205, #84779 ) ;
#36909 = FACE_OUTER_BOUND ( 'NONE', #118563, .T. ) ;
#36910 = DIRECTION ( 'NONE',  ( 0.000000000000000000, 1.000000000000000000, 0.000000000000000000 ) ) ;
#36912 = AXIS2_PLACEMENT_3D ( 'NONE', #59095, #98351, #75649 ) ;
#36911 = AXIS2_PLACEMENT_3D ( 'NONE', #109431, #11218, #79966 ) ;
#36913 = ORIENTED_EDGE ( 'NONE', *, *, #13769, .F. ) ;
#36914 = ORIENTED_EDGE ( 'NONE', *, *, #87975, .F. ) ;
#36915 = EDGE_LOOP ( 'NONE', ( #127961, #93799, #73848, #71347 ) ) ;
#36916 = EDGE_LOOP ( 'NONE', ( #14662, #37841 ) ) ;
#36917 = CARTESIAN_POINT ( 'NONE',  ( 17.48307833624011209, -2.102402844586175323, -4.293715869774332283 ) ) ;
#36918 = DIRECTION ( 'NONE',  ( 0.000000000000000000, 0.000000000000000000, 1.000000000000000000 ) ) ;
#36920 = ORIENTED_EDGE ( 'NONE', *, *, #23266, .F. ) ;
#36919 = ORIENTED_EDGE ( 'NONE', *, *, #72625, .F. ) ;
#36921 = VERTEX_POINT ( 'NONE', #99849 ) ;
#36922 = LINE ( 'NONE', #106922, #10279 ) ;
#36924 = AXIS2_PLACEMENT_3D ( 'NONE', #120566, #70814, #5919 ) ;
#36923 = AXIS2_PLACEMENT_3D ( 'NONE', #118574, #119229, #110689 ) ;
#36925 = AXIS2_PLACEMENT_3D ( 'NONE', #3282, #24854, #123058 ) ;
#36926 = CARTESIAN_POINT ( 'NONE',  ( 6.714630671503883264, -2.499999999999365397, 9.763603585388606731 ) ) ;
#36927 = CARTESIAN_POINT ( 'NONE',  ( 11.24999999999990763, 2.500000000000000000, -7.188010851410854052 ) ) ;
#36928 = CARTESIAN_POINT ( 'NONE',  ( -8.550000000000007816, 2.500000000000000000, 6.148780366869520009 ) ) ;
#36929 = CARTESIAN_POINT ( 'NONE',  ( 0.5999999999999555689, 12.50000000000000000, 4.676537180435972552 ) ) ;
#36930 = ORIENTED_EDGE ( 'NONE', *, *, #79877, .F. ) ;
#36931 = ORIENTED_EDGE ( 'NONE', *, *, #83144, .T. ) ;
#36932 = ORIENTED_EDGE ( 'NONE', *, *, #64013, .T. ) ;
#36933 = ORIENTED_EDGE ( 'NONE', *, *, #79862, .T. ) ;
#36934 = DIRECTION ( 'NONE',  ( 0.000000000000000000, 0.000000000000000000, 1.000000000000000000 ) ) ;
#36935 = ORIENTED_EDGE ( 'NONE', *, *, #95915, .T. ) ;
#36936 = AXIS2_PLACEMENT_3D ( 'NONE', #78455, #58164, #47692 ) ;
#36937 = ORIENTED_EDGE ( 'NONE', *, *, #38473, .T. ) ;
#36939 = DIRECTION ( 'NONE',  ( -4.274815082592931898E-19, -0.9999939076577903929, -0.003490651415223739937 ) ) ;
#36938 = AXIS2_PLACEMENT_3D ( 'NONE', #34343, #55884, #84706 ) ;
#36940 = ADVANCED_FACE ( 'NONE', ( #10172 ), #119459, .T. ) ;
#36941 = CARTESIAN_POINT ( 'NONE',  ( -11.44999999999999751, 2.500000000000000000, 2.611473670974873151 ) ) ;
#36943 = AXIS2_PLACEMENT_3D ( 'NONE', #68388, #30430, #29134 ) ;
#36942 = LINE ( 'NONE', #25826, #91761 ) ;
#36944 = DIRECTION ( 'NONE',  ( 0.000000000000000000, 0.000000000000000000, 1.000000000000000000 ) ) ;
#36945 = FACE_OUTER_BOUND ( 'NONE', #12601, .T. ) ;
#36946 = CIRCLE ( 'NONE', #108029, 0.06509327318403745899 ) ;
#36947 = ORIENTED_EDGE ( 'NONE', *, *, #29468, .F. ) ;
#36949 = AXIS2_PLACEMENT_3D ( 'NONE', #75341, #67261, #38515 ) ;
#36948 = CARTESIAN_POINT ( 'NONE',  ( 9.349999999999916156, 12.50000000000000000, -1.818653347947326138 ) ) ;
#36950 = ORIENTED_EDGE ( 'NONE', *, *, #93458, .T. ) ;
#36951 = AXIS2_PLACEMENT_3D ( 'NONE', #81881, #60967, #112014 ) ;
#36952 = CARTESIAN_POINT ( 'NONE',  ( 6.849999999999929479, 2.500000000000000000, -1.818653347947326138 ) ) ;
#36953 = VERTEX_POINT ( 'NONE', #50112 ) ;
#36954 = CARTESIAN_POINT ( 'NONE',  ( 115.5000000000000000, -2.000000000000000000, -4.999999999999997335 ) ) ;
#36955 = DIRECTION ( 'NONE',  ( 0.000000000000000000, 1.000000000000000000, 0.000000000000000000 ) ) ;
#36956 = EDGE_LOOP ( 'NONE', ( #55595, #6218 ) ) ;
#36957 = CARTESIAN_POINT ( 'NONE',  ( -2.900000000000029221, 2.500000000000000000, -5.022947341949754119 ) ) ;
#36958 = CONICAL_SURFACE ( 'NONE', #110103, 0.09999999999999982514, 0.003490658503988666988 ) ;
#36959 = DIRECTION ( 'NONE',  ( -0.000000000000000000, -1.000000000000000000, -0.000000000000000000 ) ) ;
#36960 = EDGE_LOOP ( 'NONE', ( #39028, #125873, #6625, #105908 ) ) ;
#36961 = AXIS2_PLACEMENT_3D ( 'NONE', #84664, #115382, #93843 ) ;
#36963 = AXIS2_PLACEMENT_3D ( 'NONE', #28201, #77937, #71178 ) ;
#36962 = AXIS2_PLACEMENT_3D ( 'NONE', #1026, #1660, #40977 ) ;
#36964 = DIRECTION ( 'NONE',  ( 0.000000000000000000, 1.000000000000000000, 0.000000000000000000 ) ) ;
#36965 = VERTEX_POINT ( 'NONE', #89999 ) ;
#36966 = ORIENTED_EDGE ( 'NONE', *, *, #95769, .T. ) ;
#36967 = CARTESIAN_POINT ( 'NONE',  ( 13.34999999999989662, 12.50000000000000000, -2.857883832488653741 ) ) ;
#36968 = CARTESIAN_POINT ( 'NONE',  ( -2.300000000000032685, 2.500000000000000000, -0.3464101615137783474 ) ) ;
#36969 = CARTESIAN_POINT ( 'NONE',  ( 185.6718750003414016, 9.264065473108010111E-16, -7.564683531250000925 ) ) ;
#36970 = CARTESIAN_POINT ( 'NONE',  ( 11.84999999999990727, 2.500000000000000000, -1.918653347947326004 ) ) ;
#36971 = CARTESIAN_POINT ( 'NONE',  ( 2.899999999999945732, 12.50000000000000000, -4.330127018922201643 ) ) ;
#36972 = DIRECTION ( 'NONE',  ( 0.000000000000000000, 1.000000000000000000, 0.000000000000000000 ) ) ;
#36973 = AXIS2_PLACEMENT_3D ( 'NONE', #5014, #15479, #63954 ) ;
#36974 = ORIENTED_EDGE ( 'NONE', *, *, #52279, .F. ) ;
#36975 = DIRECTION ( 'NONE',  ( 0.000000000000000000, 0.000000000000000000, 1.000000000000000000 ) ) ;
#36976 = EDGE_CURVE ( 'NONE', #109372, #71330, #51266, .T. ) ;
#36977 = ORIENTED_EDGE ( 'NONE', *, *, #68458, .F. ) ;
#36978 = EDGE_CURVE ( 'NONE', #64891, #224, #82130, .T. ) ;
#36979 = PLANE ( 'NONE',  #37103 ) ;
#36980 = CARTESIAN_POINT ( 'NONE',  ( 10.64999999999991331, 2.500000000000000000, -2.411473670974877859 ) ) ;
#36981 = DIRECTION ( 'NONE',  ( -0.000000000000000000, -1.000000000000000000, -0.000000000000000000 ) ) ;
#36982 = DIRECTION ( 'NONE',  ( -0.000000000000000000, -1.000000000000000000, -0.000000000000000000 ) ) ;
#36983 = EDGE_CURVE ( 'NONE', #27754, #74400, #57503, .T. ) ;
#36984 = DIRECTION ( 'NONE',  ( 0.000000000000000000, 1.000000000000000000, 0.000000000000000000 ) ) ;
#36985 = ORIENTED_EDGE ( 'NONE', *, *, #10221, .F. ) ;
#36986 = CIRCLE ( 'NONE', #3624, 0.06509327318403745899 ) ;
#36987 = AXIS2_PLACEMENT_3D ( 'NONE', #9458, #70312, #49399 ) ;
#36988 = DIRECTION ( 'NONE',  ( 0.000000000000000000, 1.000000000000000000, 0.000000000000000000 ) ) ;
#36989 = CARTESIAN_POINT ( 'NONE',  ( 6.049999999999932321, 2.500000000000000000, -1.718653347947326049 ) ) ;
#36990 = EDGE_CURVE ( 'NONE', #72747, #43219, #115987, .T. ) ;
#36991 = ADVANCED_FACE ( 'NONE', ( #32419 ), #55443, .T. ) ;
#36992 = ADVANCED_FACE ( 'NONE', ( #40945 ), #63790, .T. ) ;
#36993 = EDGE_CURVE ( 'NONE', #118684, #102955, #5253, .T. ) ;
#36994 = EDGE_LOOP ( 'NONE', ( #64081, #44697, #23454, #53946 ) ) ;
#36996 = AXIS2_PLACEMENT_3D ( 'NONE', #61681, #101593, #22403 ) ;
#36995 = CONICAL_SURFACE ( 'NONE', #22439, 0.09999999999999982514, 0.003490658503988666988 ) ;
#36997 = CARTESIAN_POINT ( 'NONE',  ( -9.600000000000008527, 2.500000000000000000, -3.637306695894645614 ) ) ;
#36998 = EDGE_LOOP ( 'NONE', ( #89988, #31729, #90378, #100131 ) ) ;
#36999 = VERTEX_POINT ( 'NONE', #2936 ) ;
#37000 = CARTESIAN_POINT ( 'NONE',  ( -14.14999999999998792, 12.50000000000000000, 2.857883832488652853 ) ) ;
#37001 = ADVANCED_FACE ( 'NONE', ( #12724 ), #110928, .T. ) ;
#37002 = VERTEX_POINT ( 'NONE', #12094 ) ;
#37003 = LINE ( 'NONE', #68380, #73737 ) ;
#37004 = LINE ( 'NONE', #78225, #58936 ) ;
#37006 = VECTOR ( 'NONE', #77265, 1000.000000000000000 ) ;
#37005 = CIRCLE ( 'NONE', #112314, 0.09999999999999982514 ) ;
#37007 = CARTESIAN_POINT ( 'NONE',  ( 0.8499999999999550138, 2.500000000000000000, -5.902370205355750521 ) ) ;
#37008 = ORIENTED_EDGE ( 'NONE', *, *, #5883, .F. ) ;
#37009 = VECTOR ( 'NONE', #31730, 1000.000000000000000 ) ;
#37010 = FACE_BOUND ( 'NONE', #94498, .T. ) ;
#37012 = ORIENTED_EDGE ( 'NONE', *, *, #113142, .F. ) ;
#37011 = DIRECTION ( 'NONE',  ( 0.000000000000000000, -0.9999939076577903929, 0.003490651415223739937 ) ) ;
#37013 = CARTESIAN_POINT ( 'NONE',  ( 1.899999999999951283, 2.500000000000000000, -0.4464101615137782142 ) ) ;
#37014 = CARTESIAN_POINT ( 'NONE',  ( -4.600000000000025402, 12.50000000000000000, -0.06509327318403980434 ) ) ;
#37015 = VERTEX_POINT ( 'NONE', #42882 ) ;
#37016 = ORIENTED_EDGE ( 'NONE', *, *, #39020, .T. ) ;
#37017 = VERTEX_POINT ( 'NONE', #11452 ) ;
#37018 = DIRECTION ( 'NONE',  ( 0.000000000000000000, -0.9999939076577903929, 0.003490651415223739937 ) ) ;
#37019 = CARTESIAN_POINT ( 'NONE',  ( -5.600000000000020073, 2.500000000000000000, -0.4464101615137782142 ) ) ;
#37020 = DIRECTION ( 'NONE',  ( -4.274815082592931898E-19, -0.9999939076577903929, -0.003490651415223739937 ) ) ;
#37021 = EDGE_CURVE ( 'NONE', #46732, #110704, #34538, .T. ) ;
#37022 = FACE_BOUND ( 'NONE', #75223, .T. ) ;
#37023 = EDGE_LOOP ( 'NONE', ( #62015, #51658 ) ) ;
#37024 = CONICAL_SURFACE ( 'NONE', #16062, 0.1000000000000002554, 0.003490658503988666988 ) ;
#37025 = CIRCLE ( 'NONE', #114374, 0.1000000000000002554 ) ;
#37026 = DIRECTION ( 'NONE',  ( -0.000000000000000000, 1.000000000000000000, -0.000000000000000000 ) ) ;
#37027 = FACE_OUTER_BOUND ( 'NONE', #63183, .T. ) ;
#37028 = AXIS2_PLACEMENT_3D ( 'NONE', #70873, #112736, #32898 ) ;
#37029 = CARTESIAN_POINT ( 'NONE',  ( -9.550000000000006040, 2.500000000000000000, -2.165063509461101710 ) ) ;
#37030 = VECTOR ( 'NONE', #113472, 1000.000000000000000 ) ;
#37032 = ADVANCED_FACE ( 'NONE', ( #91302 ), #82794, .T. ) ;
#37031 = CARTESIAN_POINT ( 'NONE',  ( 4.799999999999935874, 12.50000000000000000, 4.048810130592458201 ) ) ;
#37033 = DIRECTION ( 'NONE',  ( 0.000000000000000000, 0.000000000000000000, 1.000000000000000000 ) ) ;
#37034 = EDGE_CURVE ( 'NONE', #4134, #44028, #99277, .T. ) ;
#37035 = DIRECTION ( 'NONE',  ( 0.000000000000000000, 0.000000000000000000, 1.000000000000000000 ) ) ;
#37036 = VECTOR ( 'NONE', #51404, 1000.000000000000000 ) ;
#37037 = FACE_OUTER_BOUND ( 'NONE', #128862, .T. ) ;
#37038 = ADVANCED_FACE ( 'NONE', ( #41587 ), #30335, .T. ) ;
#37039 = AXIS2_PLACEMENT_3D ( 'NONE', #37063, #56031, #45591 ) ;
#37040 = AXIS2_PLACEMENT_3D ( 'NONE', #57102, #126497, #16516 ) ;
#37041 = EDGE_CURVE ( 'NONE', #12469, #95314, #65801, .T. ) ;
#37042 = VERTEX_POINT ( 'NONE', #13381 ) ;
#37043 = ORIENTED_EDGE ( 'NONE', *, *, #113826, .F. ) ;
#37044 = ORIENTED_EDGE ( 'NONE', *, *, #13327, .T. ) ;
#37045 = ORIENTED_EDGE ( 'NONE', *, *, #95094, .T. ) ;
#37046 = ORIENTED_EDGE ( 'NONE', *, *, #60683, .F. ) ;
#37047 = CARTESIAN_POINT ( 'NONE',  ( -9.150000000000009237, 2.500000000000000000, 2.757883832488649656 ) ) ;
#37048 = EDGE_CURVE ( 'NONE', #109438, #106434, #26110, .T. ) ;
#37049 = DIRECTION ( 'NONE',  ( 0.000000000000000000, 0.000000000000000000, -1.000000000000000000 ) ) ;
#37051 = EDGE_CURVE ( 'NONE', #82756, #16935, #126465, .T. ) ;
#37050 = VERTEX_POINT ( 'NONE', #123345 ) ;
#37052 = FACE_BOUND ( 'NONE', #89565, .T. ) ;
#37054 = CARTESIAN_POINT ( 'NONE',  ( 12.49999999999990052, 2.500000000000000000, 0.5928203230275495006 ) ) ;
#37053 = AXIS2_PLACEMENT_3D ( 'NONE', #89815, #40084, #108800 ) ;
#37055 = EDGE_CURVE ( 'NONE', #41488, #28130, #90656, .T. ) ;
#37056 = ADVANCED_FACE ( 'NONE', ( #31748 ), #103470, .T. ) ;
#37059 = EDGE_CURVE ( 'NONE', #121575, #88292, #59589, .T. ) ;
#37058 = AXIS2_PLACEMENT_3D ( 'NONE', #73745, #82308, #64580 ) ;
#37057 = CIRCLE ( 'NONE', #32958, 0.06509327318403745899 ) ;
#37060 = CARTESIAN_POINT ( 'NONE',  ( 14.99999999999992895, 12.50000000000000000, 0.06509327318403515528 ) ) ;
#37061 = CARTESIAN_POINT ( 'NONE',  ( 8.949999999999917577, 12.50000000000000000, 6.148780366869520009 ) ) ;
#37062 = DIRECTION ( 'NONE',  ( 0.000000000000000000, 0.000000000000000000, 1.000000000000000000 ) ) ;
#37063 = CARTESIAN_POINT ( 'NONE',  ( 13.09999999999989839, 12.50000000000000000, 0.3464101615137735735 ) ) ;
#37064 = EDGE_LOOP ( 'NONE', ( #74453, #16806, #628, #100582 ) ) ;
#37065 = DIRECTION ( 'NONE',  ( 0.000000000000000000, 0.000000000000000000, 1.000000000000000000 ) ) ;
#37066 = ADVANCED_FACE ( 'NONE', ( #54582 ), #11525, .T. ) ;
#37067 = VERTEX_POINT ( 'NONE', #104967 ) ;
#37068 = ORIENTED_EDGE ( 'NONE', *, *, #78517, .T. ) ;
#37069 = ORIENTED_EDGE ( 'NONE', *, *, #72381, .F. ) ;
#37070 = LINE ( 'NONE', #96597, #78001 ) ;
#37071 = DIRECTION ( 'NONE',  ( 0.000000000000000000, 0.000000000000000000, -1.000000000000000000 ) ) ;
#37072 = CARTESIAN_POINT ( 'NONE',  ( -1.050000000000037792, 2.500000000000000000, 1.818653347947321475 ) ) ;
#37073 = ORIENTED_EDGE ( 'NONE', *, *, #50809, .F. ) ;
#37074 = CONICAL_SURFACE ( 'NONE', #112373, 0.1000000000000002554, 0.003490658503988666988 ) ;
#37075 = CARTESIAN_POINT ( 'NONE',  ( 2.499999999999981792, 2.500000000000000000, 4.330127018922196314 ) ) ;
#37076 = FACE_OUTER_BOUND ( 'NONE', #39619, .T. ) ;
#37077 = DIRECTION ( 'NONE',  ( -0.000000000000000000, -1.000000000000000000, -0.000000000000000000 ) ) ;
#37078 = CARTESIAN_POINT ( 'NONE',  ( 184.2395833340161175, 4.445597072760117285, 7.699999999999999289 ) ) ;
#37079 = DIRECTION ( 'NONE',  ( -4.274815082592931898E-19, -0.9999939076577903929, -0.003490651415223739937 ) ) ;
#37080 = PLANE ( 'NONE',  #69660 ) ;
#37081 = CARTESIAN_POINT ( 'NONE',  ( -5.400000000000020783, 2.500000000000000000, 0.5928203230275495006 ) ) ;
#37082 = VERTEX_POINT ( 'NONE', #44137 ) ;
#37083 = DIRECTION ( 'NONE',  ( 0.000000000000000000, 1.000000000000000000, 0.000000000000000000 ) ) ;
#37084 = AXIS2_PLACEMENT_3D ( 'NONE', #19867, #18569, #47394 ) ;
#37085 = ORIENTED_EDGE ( 'NONE', *, *, #108031, .T. ) ;
#37086 = AXIS2_PLACEMENT_3D ( 'NONE', #102981, #22519, #62436 ) ;
#37087 = EDGE_LOOP ( 'NONE', ( #91564, #45405 ) ) ;
#37088 = CARTESIAN_POINT ( 'NONE',  ( -6.850000000000013856, 2.500000000000000000, 6.741600689897071952 ) ) ;
#37089 = CARTESIAN_POINT ( 'NONE',  ( -9.150000000000009237, 2.500000000000000000, 1.472243186433545459 ) ) ;
#37090 = CARTESIAN_POINT ( 'NONE',  ( 3.349999999999942801, 12.50000000000000000, 2.857883832488649301 ) ) ;
#37091 = ORIENTED_EDGE ( 'NONE', *, *, #762, .T. ) ;
#37094 = ORIENTED_EDGE ( 'NONE', *, *, #115691, .F. ) ;
#37093 = CIRCLE ( 'NONE', #95578, 0.06509327318403745899 ) ;
#37092 = AXIS2_PLACEMENT_3D ( 'NONE', #49730, #83052, #12984 ) ;
#37095 = DIRECTION ( 'NONE',  ( 0.000000000000000000, 0.000000000000000000, 1.000000000000000000 ) ) ;
#37096 = CIRCLE ( 'NONE', #110243, 0.06509327318403741736 ) ;
#37097 = EDGE_CURVE ( 'NONE', #7181, #7665, #84682, .T. ) ;
#37098 = CARTESIAN_POINT ( 'NONE',  ( 26.74600275967221208, 2.978654849834052154, -2.722800557139402500 ) ) ;
#37099 = DIRECTION ( 'NONE',  ( 0.000000000000000000, 1.000000000000000000, 0.000000000000000000 ) ) ;
#37100 = ORIENTED_EDGE ( 'NONE', *, *, #41893, .T. ) ;
#37101 = ORIENTED_EDGE ( 'NONE', *, *, #118716, .F. ) ;
#37102 = CARTESIAN_POINT ( 'NONE',  ( 10.64999999999990976, 12.50000000000000000, -6.841600689897077814 ) ) ;
#37104 = VECTOR ( 'NONE', #60229, 1000.000000000000114 ) ;
#37103 = AXIS2_PLACEMENT_3D ( 'NONE', #76900, #106985, #17299 ) ;
#37105 = ORIENTED_EDGE ( 'NONE', *, *, #47603, .F. ) ;
#37106 = DIRECTION ( 'NONE',  ( -0.000000000000000000, -1.000000000000000000, -0.000000000000000000 ) ) ;
#37107 = CIRCLE ( 'NONE', #53818, 0.1000000000000002554 ) ;
#37108 = DIRECTION ( 'NONE',  ( 0.000000000000000000, 0.000000000000000000, 1.000000000000000000 ) ) ;
#37109 = ORIENTED_EDGE ( 'NONE', *, *, #84735, .F. ) ;
#37110 = CARTESIAN_POINT ( 'NONE',  ( 11.64999999999990443, 2.500000000000000000, 2.857883832488649301 ) ) ;
#37111 = DIRECTION ( 'NONE',  ( 0.000000000000000000, -0.000000000000000000, 1.000000000000000000 ) ) ;
#37112 = CARTESIAN_POINT ( 'NONE',  ( -7.900000000000014566, 12.50000000000000000, -0.7579135962115916003 ) ) ;
#37113 = ADVANCED_FACE ( 'NONE', ( #76827 ), #32488, .T. ) ;
#37114 = CARTESIAN_POINT ( 'NONE',  ( -12.04999999999999538, 2.500000000000000000, 2.165063509461097713 ) ) ;
#37115 = EDGE_LOOP ( 'NONE', ( #82160, #13364, #7011, #123045 ) ) ;
#37117 = CIRCLE ( 'NONE', #41330, 0.06509327318403745899 ) ;
#37116 = CARTESIAN_POINT ( 'NONE',  ( -11.64999999999999680, 12.50000000000000000, 2.857883832488649301 ) ) ;
#37118 = DIRECTION ( 'NONE',  ( -0.000000000000000000, 1.000000000000000000, -0.000000000000000000 ) ) ;
#37119 = CIRCLE ( 'NONE', #76824, 0.09999999999999999167 ) ;
#37120 = EDGE_LOOP ( 'NONE', ( #43824, #86028, #24811, #54507 ) ) ;
#37121 = ORIENTED_EDGE ( 'NONE', *, *, #39273, .F. ) ;
#37122 = CARTESIAN_POINT ( 'NONE',  ( 185.8385416670080872, 6.551208109652274736, 3.782341765625001351 ) ) ;
#37123 = FACE_OUTER_BOUND ( 'NONE', #37213, .T. ) ;
#37124 = DIRECTION ( 'NONE',  ( -0.000000000000000000, 1.000000000000000000, -0.000000000000000000 ) ) ;
#37125 = LINE ( 'NONE', #87484, #20873 ) ;
#37126 = AXIS2_PLACEMENT_3D ( 'NONE', #69247, #119009, #18218 ) ;
#37128 = AXIS2_PLACEMENT_3D ( 'NONE', #121098, #100178, #50423 ) ;
#37127 = CARTESIAN_POINT ( 'NONE',  ( -1.250000000000035749, 2.500000000000000000, -2.857883832488653741 ) ) ;
#37129 = DIRECTION ( 'NONE',  ( 0.000000000000000000, 0.000000000000000000, -1.000000000000000000 ) ) ;
#37130 = AXIS2_PLACEMENT_3D ( 'NONE', #59226, #87354, #29120 ) ;
#37131 = DIRECTION ( 'NONE',  ( 0.000000000000000000, 0.000000000000000000, 1.000000000000000000 ) ) ;
#37132 = LINE ( 'NONE', #6335, #70002 ) ;
#37133 = DIRECTION ( 'NONE',  ( 0.000000000000000000, 1.000000000000000000, 0.000000000000000000 ) ) ;
#37134 = AXIS2_PLACEMENT_3D ( 'NONE', #22434, #61707, #62976 ) ;
#37135 = CONICAL_SURFACE ( 'NONE', #116530, 0.1000000000000000056, 0.003490658503988666988 ) ;
#37136 = CARTESIAN_POINT ( 'NONE',  ( -5.650000000000023448, 2.500000000000000000, -1.818653347947326138 ) ) ;
#37137 = AXIS2_PLACEMENT_3D ( 'NONE', #10679, #29705, #119362 ) ;
#37138 = CIRCLE ( 'NONE', #78910, 0.06509327318403745899 ) ;
#37139 = EDGE_CURVE ( 'NONE', #37472, #118696, #106910, .T. ) ;
#37140 = VERTEX_POINT ( 'NONE', #45437 ) ;
#37141 = CARTESIAN_POINT ( 'NONE',  ( -7.900000000000011013, 12.50000000000000000, 3.572213422710607489 ) ) ;
#37142 = CIRCLE ( 'NONE', #110288, 7.700000000000000178 ) ;
#37143 = DIRECTION ( 'NONE',  ( 0.000000000000000000, 0.000000000000000000, 1.000000000000000000 ) ) ;
#37144 = CARTESIAN_POINT ( 'NONE',  ( 5.399999999999932854, 12.50000000000000000, 3.637306695894644726 ) ) ;
#37145 = CARTESIAN_POINT ( 'NONE',  ( -3.749999999999991118, 2.500000000000000000, -2.165063509461101710 ) ) ;
#37146 = ADVANCED_FACE ( 'NONE', ( #46079 ), #113937, .T. ) ;
#37147 = VERTEX_POINT ( 'NONE', #74246 ) ;
#37148 = CARTESIAN_POINT ( 'NONE',  ( -1.250000000000036193, 12.50000000000000000, 1.472243186433545459 ) ) ;
#37150 = AXIS2_PLACEMENT_3D ( 'NONE', #36848, #45381, #97044 ) ;
#37149 = AXIS2_PLACEMENT_3D ( 'NONE', #67014, #57214, #118061 ) ;
#37151 = CARTESIAN_POINT ( 'NONE',  ( -6.650000000000014566, 12.50000000000000000, 6.495190528383297135 ) ) ;
#37153 = VERTEX_POINT ( 'NONE', #115424 ) ;
#37152 = CARTESIAN_POINT ( 'NONE',  ( 1.649999999999949729, 12.50000000000000000, 5.802370205355744659 ) ) ;
#37154 = ADVANCED_FACE ( 'NONE', ( #96442 ), #109736, .T. ) ;
#37155 = ADVANCED_FACE ( 'NONE', ( #53963 ), #63767, .T. ) ;
#37156 = EDGE_CURVE ( 'NONE', #25512, #89644, #13570, .T. ) ;
#37157 = EDGE_CURVE ( 'NONE', #112116, #121499, #122446, .T. ) ;
#37158 = ADVANCED_FACE ( 'NONE', ( #6754 ), #65993, .T. ) ;
#37159 = EDGE_LOOP ( 'NONE', ( #113047, #42546, #43801, #11606 ) ) ;
#37160 = VERTEX_POINT ( 'NONE', #84704 ) ;
#37161 = ORIENTED_EDGE ( 'NONE', *, *, #1652, .T. ) ;
#37162 = ORIENTED_EDGE ( 'NONE', *, *, #11829, .T. ) ;
#37163 = PLANE ( 'NONE',  #8954 ) ;
#37165 = EDGE_CURVE ( 'NONE', #94349, #43625, #101513, .T. ) ;
#37164 = AXIS2_PLACEMENT_3D ( 'NONE', #98689, #100006, #108525 ) ;
#37166 = CARTESIAN_POINT ( 'NONE',  ( -9.350000000000006750, 2.500000000000000000, 2.511473670974873507 ) ) ;
#37167 = DIRECTION ( 'NONE',  ( 0.000000000000000000, 0.000000000000000000, 1.000000000000000000 ) ) ;
#37168 = ADVANCED_FACE ( 'NONE', ( #15944 ), #124635, .T. ) ;
#37169 = LINE ( 'NONE', #48258, #8065 ) ;
#37171 = ORIENTED_EDGE ( 'NONE', *, *, #45432, .F. ) ;
#37170 = EDGE_CURVE ( 'NONE', #98821, #79461, #26302, .T. ) ;
#37172 = DIRECTION ( 'NONE',  ( 0.000000000000000000, -0.000000000000000000, 1.000000000000000000 ) ) ;
#37173 = ORIENTED_EDGE ( 'NONE', *, *, #80459, .F. ) ;
#37174 = DIRECTION ( 'NONE',  ( 0.000000000000000000, 0.000000000000000000, -1.000000000000000000 ) ) ;
#37175 = CARTESIAN_POINT ( 'NONE',  ( 14.38463633656414942, -2.499999999998971489, -7.683002074691544614 ) ) ;
#37176 = DIRECTION ( 'NONE',  ( 0.000000000000000000, 0.000000000000000000, 1.000000000000000000 ) ) ;
#37177 = CARTESIAN_POINT ( 'NONE',  ( 20.25366426269196296, -2.573118374675439135, 4.179292740210999391 ) ) ;
#37178 = VERTEX_POINT ( 'NONE', #66977 ) ;
#37179 = AXIS2_PLACEMENT_3D ( 'NONE', #114043, #33560, #73459 ) ;
#37180 = AXIS2_PLACEMENT_3D ( 'NONE', #80630, #62278, #120543 ) ;
#37181 = EDGE_LOOP ( 'NONE', ( #33253, #33089, #15732, #13535 ) ) ;
#37182 = ORIENTED_EDGE ( 'NONE', *, *, #46082, .F. ) ;
#37183 = ORIENTED_EDGE ( 'NONE', *, *, #56735, .T. ) ;
#37184 = CARTESIAN_POINT ( 'NONE',  ( 1.449999999999950440, 2.500000000000000000, 6.148780366869520009 ) ) ;
#37185 = CARTESIAN_POINT ( 'NONE',  ( 9.599999999999914380, 12.50000000000000000, -4.957854068765716882 ) ) ;
#37186 = CARTESIAN_POINT ( 'NONE',  ( 14.59999999999989484, 2.500000000000000000, 0.09999999999999772959 ) ) ;
#37187 = FACE_BOUND ( 'NONE', #79665, .T. ) ;
#37188 = DIRECTION ( 'NONE',  ( 0.000000000000000000, 0.000000000000000000, 1.000000000000000000 ) ) ;
#37189 = CARTESIAN_POINT ( 'NONE',  ( -12.04999999999999716, 12.50000000000000000, -6.430097255199260786 ) ) ;
#37190 = AXIS2_PLACEMENT_3D ( 'NONE', #85391, #26480, #119354 ) ;
#37191 = DIRECTION ( 'NONE',  ( 0.000000000000000000, 1.000000000000000000, 0.000000000000000000 ) ) ;
#37192 = DIRECTION ( 'NONE',  ( 0.000000000000000000, 1.000000000000000000, 0.000000000000000000 ) ) ;
#37193 = AXIS2_PLACEMENT_3D ( 'NONE', #13079, #62849, #40002 ) ;
#37194 = CARTESIAN_POINT ( 'NONE',  ( 185.5052083336747444, -6.551208109652278289, 3.782341765624995134 ) ) ;
#37195 = CARTESIAN_POINT ( 'NONE',  ( -8.100000000000013856, 2.500000000000000000, -4.576537180435977348 ) ) ;
#37196 = CARTESIAN_POINT ( 'NONE',  ( 9.149999999999920419, 2.500000000000000000, -5.802370205355749988 ) ) ;
#37197 = CIRCLE ( 'NONE', #35151, 0.1000000000000002554 ) ;
#37198 = DIRECTION ( 'NONE',  ( -0.000000000000000000, -1.000000000000000000, -0.000000000000000000 ) ) ;
#37199 = EDGE_LOOP ( 'NONE', ( #91082, #105335 ) ) ;
#37200 = ORIENTED_EDGE ( 'NONE', *, *, #95725, .F. ) ;
#37201 = ORIENTED_EDGE ( 'NONE', *, *, #58801, .F. ) ;
#37202 = VERTEX_POINT ( 'NONE', #65043 ) ;
#37203 = VECTOR ( 'NONE', #89917, 1000.000000000000000 ) ;
#37204 = CARTESIAN_POINT ( 'NONE',  ( -2.100000000000034728, 12.50000000000000000, 4.330127018922196314 ) ) ;
#37205 = ADVANCED_FACE ( 'NONE', ( #6131 ), #114035, .T. ) ;
#37206 = FACE_BOUND ( 'NONE', #127115, .T. ) ;
#37207 = FACE_OUTER_BOUND ( 'NONE', #124263, .T. ) ;
#37208 = DIRECTION ( 'NONE',  ( 0.000000000000000000, 0.000000000000000000, -1.000000000000000000 ) ) ;
#37209 = EDGE_CURVE ( 'NONE', #100004, #47911, #36908, .T. ) ;
#37210 = CIRCLE ( 'NONE', #24679, 0.06509327318403745899 ) ;
#37211 = EDGE_CURVE ( 'NONE', #5343, #114031, #63855, .T. ) ;
#37212 = AXIS2_PLACEMENT_3D ( 'NONE', #51269, #2787, #33555 ) ;
#37213 = EDGE_LOOP ( 'NONE', ( #20581, #41023, #84398, #101804 ) ) ;
#37214 = LINE ( 'NONE', #117020, #94838 ) ;
#37215 = DIRECTION ( 'NONE',  ( 0.000000000000000000, 1.000000000000000000, 0.000000000000000000 ) ) ;
#37216 = AXIS2_PLACEMENT_3D ( 'NONE', #37575, #77481, #27729 ) ;
#37217 = ORIENTED_EDGE ( 'NONE', *, *, #96363, .T. ) ;
#37218 = LINE ( 'NONE', #70370, #40770 ) ;
#37219 = DIRECTION ( 'NONE',  ( -4.274815082592931898E-19, -0.9999939076577903929, -0.003490651415223739937 ) ) ;
#37220 = ADVANCED_FACE ( 'NONE', ( #118669 ), #19945, .T. ) ;
#37221 = CIRCLE ( 'NONE', #81134, 0.06509327318403745899 ) ;
#37222 = VERTEX_POINT ( 'NONE', #8697 ) ;
#37223 = FACE_OUTER_BOUND ( 'NONE', #1715, .T. ) ;
#37224 = CARTESIAN_POINT ( 'NONE',  ( 2.049999999999950084, 2.500000000000000000, -6.395190528383301931 ) ) ;
#37225 = CIRCLE ( 'NONE', #37134, 0.06509327318403743123 ) ;
#37226 = CONICAL_SURFACE ( 'NONE', #120552, 0.1000000000000002554, 0.003490658503988666988 ) ;
#37227 = EDGE_LOOP ( 'NONE', ( #1174, #9227, #86246, #3573 ) ) ;
#37228 = VECTOR ( 'NONE', #83687, 1000.000000000000000 ) ;
#37229 = CARTESIAN_POINT ( 'NONE',  ( 3.749999999999975131, 12.50000000000000000, 6.495190528383297135 ) ) ;
#37230 = DIRECTION ( 'NONE',  ( -0.000000000000000000, 1.000000000000000000, -0.000000000000000000 ) ) ;
#37231 = VERTEX_POINT ( 'NONE', #119310 ) ;
#37232 = FACE_OUTER_BOUND ( 'NONE', #54123, .T. ) ;
#37233 = ORIENTED_EDGE ( 'NONE', *, *, #65640, .F. ) ;
#37234 = VERTEX_POINT ( 'NONE', #27707 ) ;
#37235 = CIRCLE ( 'NONE', #89539, 0.06509327318403741736 ) ;
#37236 = DIRECTION ( 'NONE',  ( -0.000000000000000000, 1.000000000000000000, -0.000000000000000000 ) ) ;
#37237 = EDGE_CURVE ( 'NONE', #89246, #6208, #18540, .T. ) ;
#37238 = ORIENTED_EDGE ( 'NONE', *, *, #126161, .F. ) ;
#37239 = CARTESIAN_POINT ( 'NONE',  ( 1.249999999999953815, 2.500000000000000000, 1.372243186433545370 ) ) ;
#37240 = FACE_BOUND ( 'NONE', #26648, .T. ) ;
#37242 = CIRCLE ( 'NONE', #53958, 0.09999999999999999167 ) ;
#37241 = CIRCLE ( 'NONE', #108319, 0.06509327318403745899 ) ;
#37243 = ORIENTED_EDGE ( 'NONE', *, *, #85171, .T. ) ;
#37244 = DIRECTION ( 'NONE',  ( 0.000000000000000000, 1.000000000000000000, 0.000000000000000000 ) ) ;
#37245 = ORIENTED_EDGE ( 'NONE', *, *, #80456, .T. ) ;
#37246 = CARTESIAN_POINT ( 'NONE',  ( -8.350000000000012079, 2.500000000000000000, -1.472243186433550122 ) ) ;
#37247 = DIRECTION ( 'NONE',  ( 1.000000000000000000, 0.000000000000000000, 0.000000000000000000 ) ) ;
#37248 = DIRECTION ( 'NONE',  ( 0.000000000000000000, 0.000000000000000000, 1.000000000000000000 ) ) ;
#37249 = CARTESIAN_POINT ( 'NONE',  ( 10.79999999999991012, 2.500000000000000000, 4.330127018922196314 ) ) ;
#37250 = CARTESIAN_POINT ( 'NONE',  ( -8.950000000000009948, 12.50000000000000000, -1.753560074763288679 ) ) ;
#37251 = EDGE_LOOP ( 'NONE', ( #78207, #95643, #13803, #20650 ) ) ;
#37252 = VERTEX_POINT ( 'NONE', #19163 ) ;
#37253 = FACE_OUTER_BOUND ( 'NONE', #48923, .T. ) ;
#37254 = EDGE_CURVE ( 'NONE', #109616, #119283, #7395, .T. ) ;
#37255 = CARTESIAN_POINT ( 'NONE',  ( 20.80940928220343267, -0.7000174339600890860, 4.161255421338324822 ) ) ;
#37256 = DIRECTION ( 'NONE',  ( -0.000000000000000000, -1.000000000000000000, -0.000000000000000000 ) ) ;
#37258 = EDGE_LOOP ( 'NONE', ( #14392, #103133 ) ) ;
#37257 = ORIENTED_EDGE ( 'NONE', *, *, #62717, .T. ) ;
#37259 = ORIENTED_EDGE ( 'NONE', *, *, #69519, .F. ) ;
#37260 = CARTESIAN_POINT ( 'NONE',  ( -12.69999999999999041, 12.50000000000000000, 4.048810130592458201 ) ) ;
#37261 = CARTESIAN_POINT ( 'NONE',  ( -0.6500000000000389910, 12.50000000000000000, -1.753560074763288679 ) ) ;
#37262 = CARTESIAN_POINT ( 'NONE',  ( -7.300000000000016698, 2.500000000000000000, -4.676537180435978769 ) ) ;
#37263 = DIRECTION ( 'NONE',  ( 0.000000000000000000, -0.9999939076577903929, 0.003490651415223739937 ) ) ;
#37264 = CARTESIAN_POINT ( 'NONE',  ( -6.450000000000014388, 2.500000000000000000, 6.048780366869521252 ) ) ;
#37265 = CIRCLE ( 'NONE', #53977, 0.09999999999999982514 ) ;
#37266 = AXIS2_PLACEMENT_3D ( 'NONE', #114505, #115127, #86984 ) ;
#37267 = CARTESIAN_POINT ( 'NONE',  ( -3.750000000000027534, 12.50000000000000000, -1.537336459617587581 ) ) ;
#37268 = DIRECTION ( 'NONE',  ( 0.000000000000000000, 0.000000000000000000, 1.000000000000000000 ) ) ;
#37269 = DIRECTION ( 'NONE',  ( 0.000000000000000000, -0.000000000000000000, 1.000000000000000000 ) ) ;
#37270 = AXIS2_PLACEMENT_3D ( 'NONE', #58156, #9026, #48984 ) ;
#37271 = ADVANCED_FACE ( 'NONE', ( #59124 ), #82650, .T. ) ;
#37272 = DIRECTION ( 'NONE',  ( 0.000000000000000000, 1.000000000000000000, 0.000000000000000000 ) ) ;
#37274 = VERTEX_POINT ( 'NONE', #39505 ) ;
#37273 = CONICAL_SURFACE ( 'NONE', #120784, 0.1000000000000002554, 0.003490658503988666988 ) ;
#37275 = CIRCLE ( 'NONE', #83337, 0.1000000000000000472 ) ;
#37276 = CARTESIAN_POINT ( 'NONE',  ( -15.39999999999997904, 12.50000000000000000, -0.6928203230275519209 ) ) ;
#37277 = EDGE_LOOP ( 'NONE', ( #3210, #43076 ) ) ;
#37278 = ORIENTED_EDGE ( 'NONE', *, *, #59161, .F. ) ;
#37279 = CARTESIAN_POINT ( 'NONE',  ( 11.64999999999990266, 12.50000000000000000, -6.560283801567339701 ) ) ;
#37280 = DIRECTION ( 'NONE',  ( 0.000000000000000000, 1.000000000000000000, 0.000000000000000000 ) ) ;
#37281 = CARTESIAN_POINT ( 'NONE',  ( 13.29999999999990301, 2.500000000000000000, 4.430127018922196847 ) ) ;
#37282 = CIRCLE ( 'NONE', #129327, 0.1000000000000002554 ) ;
#37283 = PLANE ( 'NONE',  #25359 ) ;
#37284 = VECTOR ( 'NONE', #102676, 1000.000000000000000 ) ;
#37285 = DIRECTION ( 'NONE',  ( 0.000000000000000000, 1.000000000000000000, 0.000000000000000000 ) ) ;
#37286 = DIRECTION ( 'NONE',  ( -4.274815082592931898E-19, -0.9999939076577903929, -0.003490651415223739937 ) ) ;
#37287 = CARTESIAN_POINT ( 'NONE',  ( 5.649999999999932854, 2.500000000000000000, 1.918653347947321564 ) ) ;
#37288 = ORIENTED_EDGE ( 'NONE', *, *, #123583, .F. ) ;
#37289 = DIRECTION ( 'NONE',  ( 0.000000000000000000, 0.000000000000000000, 1.000000000000000000 ) ) ;
#37290 = DIRECTION ( 'NONE',  ( 0.000000000000000000, 1.000000000000000000, 0.000000000000000000 ) ) ;
#37291 = AXIS2_PLACEMENT_3D ( 'NONE', #96762, #48324, #88215 ) ;
#37292 = ORIENTED_EDGE ( 'NONE', *, *, #110057, .T. ) ;
#37293 = EDGE_CURVE ( 'NONE', #77665, #48600, #72276, .T. ) ;
#37294 = VERTEX_POINT ( 'NONE', #67628 ) ;
#37295 = ORIENTED_EDGE ( 'NONE', *, *, #50425, .F. ) ;
#37296 = ORIENTED_EDGE ( 'NONE', *, *, #110254, .T. ) ;
#37297 = CARTESIAN_POINT ( 'NONE',  ( 6.249999999999932498, 12.50000000000000000, -5.802370205355749988 ) ) ;
#37298 = CARTESIAN_POINT ( 'NONE',  ( -10.40000000000000213, 2.500000000000000000, -2.276824562219559311E-15 ) ) ;
#37299 = EDGE_CURVE ( 'NONE', #100004, #118058, #78543, .T. ) ;
#37300 = CIRCLE ( 'NONE', #3835, 0.06509327318403745899 ) ;
#37301 = ORIENTED_EDGE ( 'NONE', *, *, #80337, .F. ) ;
#37302 = DIRECTION ( 'NONE',  ( 0.000000000000000000, 1.000000000000000000, 0.000000000000000000 ) ) ;
#37303 = CARTESIAN_POINT ( 'NONE',  ( 2.500000000000002220, 2.750000000000000000, -9.999999999999998224 ) ) ;
#37304 =( GEOMETRIC_REPRESENTATION_CONTEXT ( 3 ) GLOBAL_UNCERTAINTY_ASSIGNED_CONTEXT ( ( #99057 ) ) GLOBAL_UNIT_ASSIGNED_CONTEXT ( ( #67478, #9879, #49821 ) ) REPRESENTATION_CONTEXT ( 'NONE', 'WORKASPACE' ) );
#37305 = CARTESIAN_POINT ( 'NONE',  ( 2.299999999999946976, 2.500000000000000000, 4.676537180435972552 ) ) ;
#37306 = EDGE_LOOP ( 'NONE', ( #25296, #74863, #29032, #12026 ) ) ;
#37307 = ADVANCED_FACE ( 'NONE', ( #37553 ), #48019, .T. ) ;
#37308 = EDGE_CURVE ( 'NONE', #67061, #128241, #47365, .T. ) ;
#37309 = EDGE_CURVE ( 'NONE', #93927, #65479, #80586, .T. ) ;
#37310 = CARTESIAN_POINT ( 'NONE',  ( 9.599999999999914380, 12.50000000000000000, 5.022947341949748790 ) ) ;
#37311 = EDGE_CURVE ( 'NONE', #108239, #55973, #86828, .T. ) ;
#37312 = AXIS2_PLACEMENT_3D ( 'NONE', #2967, #84085, #93923 ) ;
#37313 = DIRECTION ( 'NONE',  ( 0.000000000000000000, 1.000000000000000000, 0.000000000000000000 ) ) ;
#37314 = ORIENTED_EDGE ( 'NONE', *, *, #29185, .F. ) ;
#37315 = CIRCLE ( 'NONE', #89528, 0.1000000000000000472 ) ;
#37316 = VERTEX_POINT ( 'NONE', #87904 ) ;
#37318 = ORIENTED_EDGE ( 'NONE', *, *, #42184, .F. ) ;
#37317 = ADVANCED_FACE ( 'NONE', ( #59788 ), #5352, .T. ) ;
#37319 = DIRECTION ( 'NONE',  ( 0.000000000000000000, 0.000000000000000000, 1.000000000000000000 ) ) ;
#37320 = EDGE_CURVE ( 'NONE', #125752, #10577, #17869, .T. ) ;
#37321 = AXIS2_PLACEMENT_3D ( 'NONE', #5329, #5964, #15131 ) ;
#37322 = ADVANCED_FACE ( 'NONE', ( #68277 ), #93225, .T. ) ;
#37323 = CARTESIAN_POINT ( 'NONE',  ( -6.450000000000019718, 2.500000000000000000, -6.248780366869526759 ) ) ;
#37324 = ADVANCED_FACE ( 'NONE', ( #12697 ), #123316, .T. ) ;
#37325 = EDGE_CURVE ( 'NONE', #30816, #26142, #34629, .T. ) ;
#37326 = ORIENTED_EDGE ( 'NONE', *, *, #77740, .T. ) ;
#37327 = FACE_OUTER_BOUND ( 'NONE', #20868, .T. ) ;
#37329 = AXIS2_PLACEMENT_3D ( 'NONE', #73402, #102854, #13182 ) ;
#37328 = DIRECTION ( 'NONE',  ( 0.000000000000000000, 0.000000000000000000, 1.000000000000000000 ) ) ;
#37330 = DIRECTION ( 'NONE',  ( 0.000000000000000000, 0.000000000000000000, 1.000000000000000000 ) ) ;
#37331 = CARTESIAN_POINT ( 'NONE',  ( 3.000000000000000000, 0.000000000000000000, 6.000000000000005329 ) ) ;
#37332 = EDGE_CURVE ( 'NONE', #112983, #64387, #99367, .T. ) ;
#37333 = VERTEX_POINT ( 'NONE', #114145 ) ;
#37334 = AXIS2_PLACEMENT_3D ( 'NONE', #6968, #65912, #105845 ) ;
#37335 = CARTESIAN_POINT ( 'NONE',  ( 0.3999999999999559464, 12.50000000000000000, -4.330127018922201643 ) ) ;
#37336 = VERTEX_POINT ( 'NONE', #121377 ) ;
#37337 = VERTEX_POINT ( 'NONE', #43485 ) ;
#37338 = CARTESIAN_POINT ( 'NONE',  ( -3.350000000000028955, 12.50000000000000000, -2.099970236277064473 ) ) ;
#37339 = VERTEX_POINT ( 'NONE', #63104 ) ;
#37340 = CARTESIAN_POINT ( 'NONE',  ( -1.650000000000035216, 2.500000000000000000, -5.702370205355749455 ) ) ;
#37341 = FACE_BOUND ( 'NONE', #105654, .T. ) ;
#37342 = DIRECTION ( 'NONE',  ( 0.000000000000000000, 1.000000000000000000, 0.000000000000000000 ) ) ;
#37343 = DIRECTION ( 'NONE',  ( -0.000000000000000000, -1.000000000000000000, -0.000000000000000000 ) ) ;
#37344 = DIRECTION ( 'NONE',  ( 0.000000000000000000, 1.000000000000000000, 0.000000000000000000 ) ) ;
#37345 = VERTEX_POINT ( 'NONE', #81470 ) ;
#37346 = CARTESIAN_POINT ( 'NONE',  ( 4.149999999999939959, 12.50000000000000000, 1.472243186433545459 ) ) ;
#37347 = LINE ( 'NONE', #85774, #2938 ) ;
#37348 = DIRECTION ( 'NONE',  ( 0.000000000000000000, 0.000000000000000000, 1.000000000000000000 ) ) ;
#37349 = DIRECTION ( 'NONE',  ( 0.000000000000000000, 0.000000000000000000, 1.000000000000000000 ) ) ;
#37350 = ORIENTED_EDGE ( 'NONE', *, *, #54697, .F. ) ;
#37351 = DIRECTION ( 'NONE',  ( 0.000000000000000000, 0.000000000000000000, -1.000000000000000000 ) ) ;
#37352 = AXIS2_PLACEMENT_3D ( 'NONE', #53075, #22341, #43274 ) ;
#37353 = AXIS2_PLACEMENT_3D ( 'NONE', #5541, #36959, #85404 ) ;
#37354 = DIRECTION ( 'NONE',  ( 0.000000000000000000, 0.000000000000000000, 1.000000000000000000 ) ) ;
#37355 = CIRCLE ( 'NONE', #29045, 0.06509327318403745899 ) ;
#37356 = ORIENTED_EDGE ( 'NONE', *, *, #43113, .T. ) ;
#37357 = DIRECTION ( 'NONE',  ( -0.000000000000000000, 1.000000000000000000, -0.000000000000000000 ) ) ;
#37358 = CARTESIAN_POINT ( 'NONE',  ( 13.34999999999989662, 2.500000000000000000, -1.472243186433550122 ) ) ;
#37359 = FACE_BOUND ( 'NONE', #101452, .T. ) ;
#37360 = CARTESIAN_POINT ( 'NONE',  ( -6.450000000000017941, 12.50000000000000000, -6.841600689897077814 ) ) ;
#37361 = CIRCLE ( 'NONE', #49888, 0.1000000000000000472 ) ;
#37362 = CONICAL_SURFACE ( 'NONE', #120873, 0.1000000000000002554, 0.003490658503988666988 ) ;
#37363 = EDGE_CURVE ( 'NONE', #6764, #44454, #68047, .T. ) ;
#37364 = CIRCLE ( 'NONE', #87507, 0.06509327318403743123 ) ;
#37365 = ORIENTED_EDGE ( 'NONE', *, *, #46632, .F. ) ;
#37366 = DIRECTION ( 'NONE',  ( -0.000000000000000000, 1.000000000000000000, -0.000000000000000000 ) ) ;
#37367 = CIRCLE ( 'NONE', #116763, 0.06509327318403745899 ) ;
#37368 = EDGE_CURVE ( 'NONE', #120641, #37017, #1599, .T. ) ;
#37369 = VERTEX_POINT ( 'NONE', #122671 ) ;
#37370 = VERTEX_POINT ( 'NONE', #31720 ) ;
#37371 = CARTESIAN_POINT ( 'NONE',  ( -9.800000000000007816, 2.500000000000000000, -3.883716857408422207 ) ) ;
#37372 = CARTESIAN_POINT ( 'NONE',  ( 186.9583333333333428, 4.445597072760117285, 7.699999999999999289 ) ) ;
#37373 = ORIENTED_EDGE ( 'NONE', *, *, #83082, .T. ) ;
#37374 = CARTESIAN_POINT ( 'NONE',  ( -11.84999999999999787, 2.500000000000000000, -6.048780366869523029 ) ) ;
#37375 = FACE_OUTER_BOUND ( 'NONE', #93716, .T. ) ;
#37376 = ADVANCED_FACE ( 'NONE', ( #104322 ), #123952, .F. ) ;
#37377 = AXIS2_PLACEMENT_3D ( 'NONE', #24889, #65445, #16958 ) ;
#37378 = CARTESIAN_POINT ( 'NONE',  ( 129.5000000000000000, 1.500000000000000000, -2.598076211353316900 ) ) ;
#37379 = CONICAL_SURFACE ( 'NONE', #5949, 0.1000000000000000472, 0.003490658503988666988 ) ;
#37380 = EDGE_LOOP ( 'NONE', ( #25089, #100801 ) ) ;
#37381 = CARTESIAN_POINT ( 'NONE',  ( -1.650000000000035216, 2.500000000000000000, -1.472243186433550122 ) ) ;
#37382 = DIRECTION ( 'NONE',  ( -0.000000000000000000, -1.000000000000000000, -0.000000000000000000 ) ) ;
#37383 = PLANE ( 'NONE',  #103564 ) ;
#37384 = VECTOR ( 'NONE', #60332, 1000.000000000000000 ) ;
#37385 = CARTESIAN_POINT ( 'NONE',  ( 18.45986577996938394, 0.7763546025154585140, -4.045836809868015749 ) ) ;
#37386 = EDGE_LOOP ( 'NONE', ( #39535, #76966 ) ) ;
#37387 = CARTESIAN_POINT ( 'NONE',  ( 6.899999999999928413, 2.500000000000000000, -3.983716857408426293 ) ) ;
#37388 = ORIENTED_EDGE ( 'NONE', *, *, #32195, .T. ) ;
#37389 = CARTESIAN_POINT ( 'NONE',  ( 2.099999999999950351, 2.500000000000000000, -2.276824562219559311E-15 ) ) ;
#37390 = CARTESIAN_POINT ( 'NONE',  ( 6.049999999999935874, 2.500000000000000000, -6.841600689897077814 ) ) ;
#37391 = ORIENTED_EDGE ( 'NONE', *, *, #8610, .F. ) ;
#37392 = DIRECTION ( 'NONE',  ( 0.000000000000000000, 1.000000000000000000, 0.000000000000000000 ) ) ;
#37393 = CARTESIAN_POINT ( 'NONE',  ( -0.8500000000000382805, 2.500000000000000000, -2.957883832488653830 ) ) ;
#37394 = FACE_OUTER_BOUND ( 'NONE', #32247, .T. ) ;
#37395 = LINE ( 'NONE', #36756, #73760 ) ;
#37396 = ORIENTED_EDGE ( 'NONE', *, *, #64334, .F. ) ;
#37397 = AXIS2_PLACEMENT_3D ( 'NONE', #118893, #78340, #387 ) ;
#37398 = DIRECTION ( 'NONE',  ( 0.000000000000000000, 0.000000000000000000, 1.000000000000000000 ) ) ;
#37399 = LINE ( 'NONE', #77308, #33456 ) ;
#37400 = CARTESIAN_POINT ( 'NONE',  ( 184.7760416670080588, 6.551208109652274736, 3.782341765625001351 ) ) ;
#37401 = DIRECTION ( 'NONE',  ( 0.000000000000000000, -0.000000000000000000, 1.000000000000000000 ) ) ;
#37402 = AXIS2_PLACEMENT_3D ( 'NONE', #27745, #76864, #36308 ) ;
#37403 = CARTESIAN_POINT ( 'NONE',  ( 10.19999999999991047, 2.500000000000000000, 4.676537180435972552 ) ) ;
#37404 = EDGE_CURVE ( 'NONE', #4260, #124496, #95253, .T. ) ;
#37405 = ORIENTED_EDGE ( 'NONE', *, *, #5369, .F. ) ;
#37406 = VERTEX_POINT ( 'NONE', #113492 ) ;
#37407 = DIRECTION ( 'NONE',  ( 0.000000000000000000, 1.000000000000000000, 0.000000000000000000 ) ) ;
#37408 = ORIENTED_EDGE ( 'NONE', *, *, #88906, .T. ) ;
#37409 = CARTESIAN_POINT ( 'NONE',  ( -0.6500000000000394351, 12.50000000000000000, 2.446380397790835826 ) ) ;
#37411 = EDGE_LOOP ( 'NONE', ( #68690, #63111 ) ) ;
#37410 = ORIENTED_EDGE ( 'NONE', *, *, #62660, .T. ) ;
#37412 = ORIENTED_EDGE ( 'NONE', *, *, #96284, .F. ) ;
#37413 = CIRCLE ( 'NONE', #10212, 0.1000000000000002554 ) ;
#37414 = DIRECTION ( 'NONE',  ( 0.000000000000000000, 0.000000000000000000, 1.000000000000000000 ) ) ;
#37415 = DIRECTION ( 'NONE',  ( 0.000000000000000000, 1.000000000000000000, 0.000000000000000000 ) ) ;
#37416 = DIRECTION ( 'NONE',  ( -4.274815082592931898E-19, -0.9999939076577903929, -0.003490651415223739937 ) ) ;
#37417 =( NAMED_UNIT ( * ) SI_UNIT ( $, .STERADIAN. ) SOLID_ANGLE_UNIT ( ) );
#37419 = CIRCLE ( 'NONE', #10218, 0.09999999999999982514 ) ;
#37418 = CONICAL_SURFACE ( 'NONE', #24884, 0.09999999999999982514, 0.003490658503988666988 ) ;
#37420 = DIRECTION ( 'NONE',  ( 0.000000000000000000, 1.000000000000000000, 0.000000000000000000 ) ) ;
#37421 = CARTESIAN_POINT ( 'NONE',  ( -0.4500000000000397571, 2.500000000000000000, -6.395190528383301931 ) ) ;
#37422 = EDGE_CURVE ( 'NONE', #80982, #95427, #25526, .T. ) ;
#37423 = DIRECTION ( 'NONE',  ( 0.000000000000000000, 1.000000000000000000, 0.000000000000000000 ) ) ;
#37424 = AXIS2_PLACEMENT_3D ( 'NONE', #33816, #52813, #84848 ) ;
#37425 = ORIENTED_EDGE ( 'NONE', *, *, #99457, .F. ) ;
#37426 = EDGE_CURVE ( 'NONE', #96763, #58128, #91928, .T. ) ;
#37427 = CARTESIAN_POINT ( 'NONE',  ( -4.400000000000025224, 2.500000000000000000, 4.676537180435972552 ) ) ;
#37428 = EDGE_LOOP ( 'NONE', ( #45654, #83977, #127279, #73984 ) ) ;
#37430 = AXIS2_PLACEMENT_3D ( 'NONE', #24603, #92045, #43613 ) ;
#37429 = CIRCLE ( 'NONE', #125239, 0.06509327318403745899 ) ;
#37431 = EDGE_LOOP ( 'NONE', ( #78878, #96183 ) ) ;
#37432 = ORIENTED_EDGE ( 'NONE', *, *, #74389, .T. ) ;
#37433 = ORIENTED_EDGE ( 'NONE', *, *, #1864, .F. ) ;
#37434 = DIRECTION ( 'NONE',  ( 0.000000000000000000, 0.000000000000000000, 1.000000000000000000 ) ) ;
#37435 = ORIENTED_EDGE ( 'NONE', *, *, #81302, .F. ) ;
#37436 = ADVANCED_FACE ( 'NONE', ( #14627 ), #36679, .T. ) ;
#37437 = VERTEX_POINT ( 'NONE', #83406 ) ;
#37438 = CARTESIAN_POINT ( 'NONE',  ( -8.300000000000011369, 12.50000000000000000, -4.330127018922201643 ) ) ;
#37439 = CARTESIAN_POINT ( 'NONE',  ( 8.299999999999922551, 2.500000000000000000, -2.385244779468109755E-15 ) ) ;
#37440 = CARTESIAN_POINT ( 'NONE',  ( 1.449999999999952216, 2.500000000000000000, 1.718653347947321386 ) ) ;
#37441 = CARTESIAN_POINT ( 'NONE',  ( -5.400000000000023448, 12.50000000000000000, -5.022947341949754119 ) ) ;
#37443 = CIRCLE ( 'NONE', #81355, 0.06509327318403745899 ) ;
#37442 = DIRECTION ( 'NONE',  ( 0.000000000000000000, 0.000000000000000000, 1.000000000000000000 ) ) ;
#37444 = ORIENTED_EDGE ( 'NONE', *, *, #46024, .F. ) ;
#37445 = LINE ( 'NONE', #118558, #42916 ) ;
#37446 = ORIENTED_EDGE ( 'NONE', *, *, #16403, .T. ) ;
#37447 = FACE_OUTER_BOUND ( 'NONE', #8900, .T. ) ;
#37449 = EDGE_LOOP ( 'NONE', ( #102369, #126192, #67548, #89589 ) ) ;
#37448 = AXIS2_PLACEMENT_3D ( 'NONE', #12319, #21506, #52258 ) ;
#37450 = CARTESIAN_POINT ( 'NONE',  ( -7.500000000000015099, 2.500000000000000000, -0.5928203230275541635 ) ) ;
#37451 = ORIENTED_EDGE ( 'NONE', *, *, #37311, .T. ) ;
#37452 = ORIENTED_EDGE ( 'NONE', *, *, #14793, .F. ) ;
#37454 = CIRCLE ( 'NONE', #54174, 0.06509327318403745899 ) ;
#37453 = DIRECTION ( 'NONE',  ( 0.000000000000000000, 0.000000000000000000, 1.000000000000000000 ) ) ;
#37455 = CARTESIAN_POINT ( 'NONE',  ( 1.899999999999951283, 2.500000000000000000, -3.983716857408426293 ) ) ;
#37456 = AXIS2_PLACEMENT_3D ( 'NONE', #71222, #121602, #31962 ) ;
#37457 = EDGE_CURVE ( 'NONE', #87251, #12173, #76380, .T. ) ;
#37458 = AXIS2_PLACEMENT_3D ( 'NONE', #129034, #100811, #79274 ) ;
#37459 = CARTESIAN_POINT ( 'NONE',  ( 13.09999999999989839, 12.50000000000000000, -0.3464101615137783474 ) ) ;
#37460 = CARTESIAN_POINT ( 'NONE',  ( -9.400000000000007461, 2.500000000000000000, 3.883716857408420431 ) ) ;
#37461 = DIRECTION ( 'NONE',  ( 1.000000000000000000, -0.000000000000000000, -7.228014483236698281E-17 ) ) ;
#37462 = EDGE_LOOP ( 'NONE', ( #17355, #33113, #85266, #9434 ) ) ;
#37463 = CARTESIAN_POINT ( 'NONE',  ( -12.89999999999999147, 12.50000000000000000, -4.395220292106237103 ) ) ;
#37464 = FACE_OUTER_BOUND ( 'NONE', #28018, .T. ) ;
#37465 = ADVANCED_FACE ( 'NONE', ( #52011 ), #63762, .T. ) ;
#37466 = LINE ( 'NONE', #15864, #108692 ) ;
#37467 = DIRECTION ( 'NONE',  ( 0.000000000000000000, 0.000000000000000000, 1.000000000000000000 ) ) ;
#37469 = ADVANCED_FACE ( 'NONE', ( #53937 ), #30426, .T. ) ;
#37468 = CIRCLE ( 'NONE', #14440, 0.06509327318403745899 ) ;
#37470 = DIRECTION ( 'NONE',  ( 0.000000000000000000, 0.000000000000000000, 1.000000000000000000 ) ) ;
#37471 = AXIS2_PLACEMENT_3D ( 'NONE', #90895, #102009, #33289 ) ;
#37472 = VERTEX_POINT ( 'NONE', #82106 ) ;
#37473 = ORIENTED_EDGE ( 'NONE', *, *, #34227, .F. ) ;
#37474 = EDGE_CURVE ( 'NONE', #93025, #118854, #13663, .T. ) ;
#37475 = EDGE_CURVE ( 'NONE', #32318, #46996, #116184, .T. ) ;
#37476 = DIRECTION ( 'NONE',  ( 0.000000000000000000, 0.000000000000000000, -1.000000000000000000 ) ) ;
#37477 = ADVANCED_FACE ( 'NONE', ( #104943 ), #55857, .T. ) ;
#37478 = VERTEX_POINT ( 'NONE', #35593 ) ;
#37479 = DIRECTION ( 'NONE',  ( 0.000000000000000000, 0.000000000000000000, 1.000000000000000000 ) ) ;
#37480 = CARTESIAN_POINT ( 'NONE',  ( 6.249999999999932498, 2.500000000000000000, -2.857883832488653741 ) ) ;
#37481 = EDGE_CURVE ( 'NONE', #97670, #48086, #45175, .T. ) ;
#37482 = CIRCLE ( 'NONE', #110616, 0.06509327318403745899 ) ;
#37483 = VERTEX_POINT ( 'NONE', #26417 ) ;
#37484 = CARTESIAN_POINT ( 'NONE',  ( 186.3750000000000284, 8.891194145520236347, 5.444286225454521982E-16 ) ) ;
#37485 = DIRECTION ( 'NONE',  ( -0.000000000000000000, 1.000000000000000000, -0.000000000000000000 ) ) ;
#37486 = EDGE_CURVE ( 'NONE', #59157, #64666, #55627, .T. ) ;
#37487 = CARTESIAN_POINT ( 'NONE',  ( 8.949999999999917577, 12.50000000000000000, 6.148780366869520009 ) ) ;
#37488 = CARTESIAN_POINT ( 'NONE',  ( 0.1999999999999576006, 2.500000000000000000, -4.576537180435978236 ) ) ;
#37489 = EDGE_LOOP ( 'NONE', ( #112764, #15012 ) ) ;
#37490 = EDGE_CURVE ( 'NONE', #114315, #47981, #80677, .T. ) ;
#37491 = DIRECTION ( 'NONE',  ( 0.000000000000000000, 0.000000000000000000, -1.000000000000000000 ) ) ;
#37492 = DIRECTION ( 'NONE',  ( 0.000000000000000000, 0.000000000000000000, 1.000000000000000000 ) ) ;
#37493 = EDGE_LOOP ( 'NONE', ( #88497, #111785, #37665, #18291 ) ) ;
#37494 = FACE_OUTER_BOUND ( 'NONE', #127774, .T. ) ;
#37495 = AXIS2_PLACEMENT_3D ( 'NONE', #125163, #17772, #106792 ) ;
#37496 = LINE ( 'NONE', #56461, #12089 ) ;
#37497 = DIRECTION ( 'NONE',  ( 0.000000000000000000, 1.000000000000000000, 0.000000000000000000 ) ) ;
#37498 = EDGE_LOOP ( 'NONE', ( #21065, #45007 ) ) ;
#37499 = DIRECTION ( 'NONE',  ( 0.000000000000000000, 0.000000000000000000, 1.000000000000000000 ) ) ;
#37500 = ORIENTED_EDGE ( 'NONE', *, *, #60957, .T. ) ;
#37502 = CIRCLE ( 'NONE', #91872, 0.06509327318403745899 ) ;
#37501 = DIRECTION ( 'NONE',  ( -0.000000000000000000, -1.000000000000000000, -0.000000000000000000 ) ) ;
#37503 = DIRECTION ( 'NONE',  ( -0.000000000000000000, -1.000000000000000000, -0.000000000000000000 ) ) ;
#37504 = DIRECTION ( 'NONE',  ( 0.000000000000000000, 1.000000000000000000, 0.000000000000000000 ) ) ;
#37505 = EDGE_LOOP ( 'NONE', ( #94672, #16477, #115830, #30143 ) ) ;
#37506 = FACE_OUTER_BOUND ( 'NONE', #17984, .T. ) ;
#37508 = AXIS2_PLACEMENT_3D ( 'NONE', #61334, #120886, #1110 ) ;
#37507 = AXIS2_PLACEMENT_3D ( 'NONE', #42292, #52116, #111679 ) ;
#37509 = DIRECTION ( 'NONE',  ( 0.000000000000000000, 1.000000000000000000, 0.000000000000000000 ) ) ;
#37510 = VECTOR ( 'NONE', #69072, 1000.000000000000000 ) ;
#37511 = EDGE_LOOP ( 'NONE', ( #97140, #29606, #74802, #112475 ) ) ;
#37512 = DIRECTION ( 'NONE',  ( -0.000000000000000000, 1.000000000000000000, -0.000000000000000000 ) ) ;
#37513 = ORIENTED_EDGE ( 'NONE', *, *, #59205, .F. ) ;
#37514 = DIRECTION ( 'NONE',  ( 0.000000000000000000, 0.000000000000000000, 1.000000000000000000 ) ) ;
#37515 = MECHANICAL_DESIGN_GEOMETRIC_PRESENTATION_REPRESENTATION (  '', ( #91884 ), #56365 ) ;
#37516 = ADVANCED_FACE ( 'NONE', ( #106255 ), #16560, .T. ) ;
#37517 = VERTEX_POINT ( 'NONE', #87242 ) ;
#37518 = CARTESIAN_POINT ( 'NONE',  ( 6.849999999999929479, 2.500000000000000000, 6.741600689897071952 ) ) ;
#37519 = DIRECTION ( 'NONE',  ( 0.000000000000000000, -0.000000000000000000, 1.000000000000000000 ) ) ;
#37520 = VERTEX_POINT ( 'NONE', #96414 ) ;
#37521 = ORIENTED_EDGE ( 'NONE', *, *, #101108, .T. ) ;
#37522 = CARTESIAN_POINT ( 'NONE',  ( -3.100000000000028511, 2.500000000000000000, 0.2464101615137736789 ) ) ;
#37523 = CARTESIAN_POINT ( 'NONE',  ( 6.249999999999932498, 2.500000000000000000, 5.802370205355744659 ) ) ;
#37524 = VERTEX_POINT ( 'NONE', #27053 ) ;
#37525 = EDGE_CURVE ( 'NONE', #87160, #42019, #97386, .T. ) ;
#37526 = CARTESIAN_POINT ( 'NONE',  ( 10.59999999999990905, 2.500000000000000000, 4.676537180435972552 ) ) ;
#37527 = DIRECTION ( 'NONE',  ( 0.000000000000000000, 1.000000000000000000, 0.000000000000000000 ) ) ;
#37528 = DIRECTION ( 'NONE',  ( 0.000000000000000000, 0.000000000000000000, 1.000000000000000000 ) ) ;
#37529 = CIRCLE ( 'NONE', #66751, 0.06509327318403745899 ) ;
#37530 = FACE_OUTER_BOUND ( 'NONE', #7161, .T. ) ;
#37531 = LINE ( 'NONE', #117326, #97485 ) ;
#37532 = DIRECTION ( 'NONE',  ( 0.000000000000000000, 0.000000000000000000, 1.000000000000000000 ) ) ;
#37533 = CONICAL_SURFACE ( 'NONE', #121145, 0.09999999999999982514, 0.003490658503988666988 ) ;
#37534 = VERTEX_POINT ( 'NONE', #126547 ) ;
#37535 = ORIENTED_EDGE ( 'NONE', *, *, #87920, .T. ) ;
#37536 = EDGE_LOOP ( 'NONE', ( #15351, #25226 ) ) ;
#37537 = ORIENTED_EDGE ( 'NONE', *, *, #118139, .T. ) ;
#37538 = CARTESIAN_POINT ( 'NONE',  ( -11.24999999999999822, 12.50000000000000000, 5.802370205355744659 ) ) ;
#37539 = CARTESIAN_POINT ( 'NONE',  ( 10.44999999999991402, 2.500000000000000000, 6.495190528383297135 ) ) ;
#37540 = CARTESIAN_POINT ( 'NONE',  ( 11.64999999999990621, 12.50000000000000000, -2.165063509461101710 ) ) ;
#37541 = ORIENTED_EDGE ( 'NONE', *, *, #23124, .T. ) ;
#37542 = FACE_BOUND ( 'NONE', #93904, .T. ) ;
#37543 = CARTESIAN_POINT ( 'NONE',  ( -13.74999999999998934, 12.50000000000000000, -1.407149913249510442 ) ) ;
#37544 = CARTESIAN_POINT ( 'NONE',  ( -6.900000000000019007, 2.500000000000000000, -0.4464101615137783252 ) ) ;
#37545 = AXIS2_PLACEMENT_3D ( 'NONE', #24413, #22503, #52580 ) ;
#37546 = AXIS2_PLACEMENT_3D ( 'NONE', #63985, #103914, #94090 ) ;
#37547 = DIRECTION ( 'NONE',  ( 0.000000000000000000, 0.000000000000000000, 1.000000000000000000 ) ) ;
#37548 = AXIS2_PLACEMENT_3D ( 'NONE', #85046, #115799, #74592 ) ;
#37549 = DIRECTION ( 'NONE',  ( -0.000000000000000000, 1.000000000000000000, -0.000000000000000000 ) ) ;
#37550 = CARTESIAN_POINT ( 'NONE',  ( -6.450000000000017941, 12.50000000000000000, -6.906693963081115051 ) ) ;
#37551 = DIRECTION ( 'NONE',  ( 0.000000000000000000, 1.000000000000000000, 0.000000000000000000 ) ) ;
#37552 = DIRECTION ( 'NONE',  ( 0.000000000000000000, 1.000000000000000000, 0.000000000000000000 ) ) ;
#37553 = FACE_OUTER_BOUND ( 'NONE', #101909, .T. ) ;
#37554 = CARTESIAN_POINT ( 'NONE',  ( -5.450000000000019718, 12.50000000000000000, 2.230156782645134950 ) ) ;
#37555 = AXIS2_PLACEMENT_3D ( 'NONE', #76790, #116697, #27044 ) ;
#37556 = DIRECTION ( 'NONE',  ( -0.000000000000000000, 1.000000000000000000, -0.000000000000000000 ) ) ;
#37558 = EDGE_CURVE ( 'NONE', #83877, #31984, #82833, .T. ) ;
#37557 = AXIS2_PLACEMENT_3D ( 'NONE', #93482, #110226, #48737 ) ;
#37559 = VERTEX_POINT ( 'NONE', #36880 ) ;
#37560 = ORIENTED_EDGE ( 'NONE', *, *, #6194, .T. ) ;
#37561 = CIRCLE ( 'NONE', #41774, 0.06509327318403743123 ) ;
#37562 = ORIENTED_EDGE ( 'NONE', *, *, #118709, .T. ) ;
#37563 = ORIENTED_EDGE ( 'NONE', *, *, #14376, .T. ) ;
#37564 = DIRECTION ( 'NONE',  ( 0.000000000000000000, 0.000000000000000000, 1.000000000000000000 ) ) ;
#37565 = CARTESIAN_POINT ( 'NONE',  ( 1.899999999999951283, 2.500000000000000000, -4.676537180435977881 ) ) ;
#37567 = ORIENTED_EDGE ( 'NONE', *, *, #47656, .F. ) ;
#37566 = ORIENTED_EDGE ( 'NONE', *, *, #111682, .T. ) ;
#37568 = VERTEX_POINT ( 'NONE', #116708 ) ;
#37569 = LINE ( 'NONE', #77476, #54198 ) ;
#37570 = ADVANCED_FACE ( 'NONE', ( #66952 ), #116158, .T. ) ;
#37571 = DIRECTION ( 'NONE',  ( 0.000000000000000000, -0.000000000000000000, 1.000000000000000000 ) ) ;
#37572 = FACE_OUTER_BOUND ( 'NONE', #98687, .T. ) ;
#37573 = DIRECTION ( 'NONE',  ( 0.000000000000000000, -0.9999939076577903929, 0.003490651415223739937 ) ) ;
#37574 = VECTOR ( 'NONE', #40804, 1000.000000000000000 ) ;
#37575 = CARTESIAN_POINT ( 'NONE',  ( -3.150000000000030553, 12.50000000000000000, 6.148780366869520009 ) ) ;
#37576 = EDGE_CURVE ( 'NONE', #26610, #111368, #97080, .T. ) ;
#37577 = DIRECTION ( 'NONE',  ( -0.000000000000000000, -1.000000000000000000, -0.000000000000000000 ) ) ;
#37578 = ADVANCED_FACE ( 'NONE', ( #4813 ), #3306, .T. ) ;
#37579 = EDGE_LOOP ( 'NONE', ( #40184, #34771, #26481, #96648 ) ) ;
#37580 = FACE_OUTER_BOUND ( 'NONE', #44056, .T. ) ;
#37581 = ORIENTED_EDGE ( 'NONE', *, *, #118428, .F. ) ;
#37582 = ORIENTED_EDGE ( 'NONE', *, *, #124943, .F. ) ;
#37583 = ORIENTED_EDGE ( 'NONE', *, *, #80617, .F. ) ;
#37584 = ADVANCED_FACE ( 'NONE', ( #34958 ), #76472, .T. ) ;
#37585 = CARTESIAN_POINT ( 'NONE',  ( 6.849999999999927702, 12.50000000000000000, 2.511473670974873507 ) ) ;
#37586 =( BOUNDED_SURFACE ( )  B_SPLINE_SURFACE ( 1, 2, ( 
 ( #61789, #80783, #12651, #59869, #89932, #110227, #31669, #1551, #89295, #110854, #71590, #99769, #111508, #129254, #120691, #120051, #40206, #61128, #10093, #50047, #21864, #101049, #11375, #82046, #256, #30405, #32341, #20563, #51332, #60503, #31049, #100411, #10707, #50662, #90577, #70947, #4759, #114094, #83356, #54512, #74815, #123904, #2847, #93814, #83972, #75444, #3495, #113446, #34262, #44720, #44063, #102977, #73512, #84634, #55176, #63060, #74172, #72884, #115351, #124567, #64975, #63710, #24423, #53885, #114730, #104898, #15221, #112811, #4119, #103637, #64345, #104274, #14584, #94438, #42808, #5416, #13946, #34910, #25066, #53249, #95103, #23787, #122629, #45367, #85271 ),
 ( #125204, #35547, #25707, #65629, #105565, #52590, #13296, #92513, #82719, #32975, #23132, #93181, #43441, #123271, #33606, #16515, #106831, #117278, #117946, #57101, #28950, #95745, #56449, #36834, #47941, #57763, #78700, #37484, #7994, #6053, #87839, #128449, #97029, #6680, #96365, #77393, #36194, #76103, #38116, #27623, #67549, #18467, #116019, #68854, #98305, #97671, #107498, #46009, #47296, #106211, #85903, #46643, #15882, #125832, #127775, #17812, #86558, #78035, #28295, #87197, #26368, #7344, #127149, #38784, #126496, #76748, #68204, #108134, #58413, #66277, #116663, #8625, #48583, #27009, #88490, #66909, #118596, #55815, #17140, #119895, #41984, #101545, #70789, #100883, #110705 ) ),
 .UNSPECIFIED., .F., .F., .F. ) 
 B_SPLINE_SURFACE_WITH_KNOTS ( ( 2, 2 ),
 ( 3, 2, 2, 2, 2, 2, 2, 2, 2, 2, 2, 2, 2, 2, 2, 2, 2, 2, 2, 2, 2, 2, 2, 2, 2, 2, 2, 2, 2, 2, 2, 2, 2, 2, 2, 2, 2, 2, 2, 2, 2, 2, 3 ),
 ( 0.000000000000000000, 1.000000000000000000 ),
 ( 0.000000000000000000, 0.02380952380952380820, 0.04761904761904761640, 0.07142857142857142461, 0.09523809523809523281, 0.1190476190476190410, 0.1428571428571428492, 0.1666666666666666574, 0.1904761904761904656, 0.2142857142857142738, 0.2380952380952380820, 0.2619047619047619180, 0.2857142857142856984, 0.3095238095238095344, 0.3333333333333333148, 0.3571428571428571508, 0.3809523809523809312, 0.4047619047619047672, 0.4285714285714285476, 0.4523809523809523836, 0.4761904761904761640, 0.5000000000000000000, 0.5238095238095238360, 0.5476190476190476719, 0.5714285714285713969, 0.5952380952380952328, 0.6190476190476190688, 0.6428571428571429047, 0.6666666666666666297, 0.6904761904761904656, 0.7142857142857143016, 0.7380952380952381375, 0.7619047619047618625, 0.7857142857142856984, 0.8095238095238095344, 0.8333333333333333703, 0.8571428571428570953, 0.8809523809523809312, 0.9047619047619047672, 0.9285714285714286031, 0.9523809523809523281, 0.9761904761904761640, 1.000000000000000000 ),
 .UNSPECIFIED. ) 
 GEOMETRIC_REPRESENTATION_ITEM ( )  RATIONAL_B_SPLINE_SURFACE ( (
 ( 1.000000000000000000, 0.8660254037844387076, 1.000000000000000000, 0.8660254037844387076, 1.000000000000000000, 0.8660254037844387076, 1.000000000000000000, 0.8660254037844387076, 1.000000000000000000, 0.8660254037844387076, 1.000000000000000000, 0.8660254037844387076, 1.000000000000000000, 0.8660254037844387076, 1.000000000000000000, 0.8660254037844387076, 1.000000000000000000, 0.8660254037844387076, 1.000000000000000000, 0.8660254037844387076, 1.000000000000000000, 0.8660254037844387076, 1.000000000000000000, 0.8660254037844387076, 1.000000000000000000, 0.8660254037844387076, 1.000000000000000000, 0.8660254037844387076, 1.000000000000000000, 0.8660254037844387076, 1.000000000000000000, 0.8660254037844387076, 1.000000000000000000, 0.8660254037844387076, 1.000000000000000000, 0.8660254037844387076, 1.000000000000000000, 0.8660254037844387076, 1.000000000000000000, 0.8660254037844387076, 1.000000000000000000, 0.8660254037844387076, 1.000000000000000000, 0.8660254037844387076, 1.000000000000000000, 0.8660254037844387076, 1.000000000000000000, 0.8660254037844387076, 1.000000000000000000, 0.8660254037844387076, 1.000000000000000000, 0.8660254037844387076, 1.000000000000000000, 0.8660254037844387076, 1.000000000000000000, 0.8660254037844387076, 1.000000000000000000, 0.8660254037844387076, 1.000000000000000000, 0.8660254037844387076, 1.000000000000000000, 0.8660254037844387076, 1.000000000000000000, 0.8660254037844387076, 1.000000000000000000, 0.8660254037844387076, 1.000000000000000000, 0.8660254037844387076, 1.000000000000000000, 0.8660254037844387076, 1.000000000000000000, 0.8660254037844387076, 1.000000000000000000, 0.8660254037844387076, 1.000000000000000000, 0.8660254037844387076, 1.000000000000000000, 0.8660254037844387076, 1.000000000000000000, 0.8660254037844387076, 1.000000000000000000, 0.8660254037844387076, 1.000000000000000000, 0.8660254037844387076, 1.000000000000000000),
 ( 1.000000000000000000, 0.8660254037844387076, 1.000000000000000000, 0.8660254037844387076, 1.000000000000000000, 0.8660254037844387076, 1.000000000000000000, 0.8660254037844387076, 1.000000000000000000, 0.8660254037844387076, 1.000000000000000000, 0.8660254037844387076, 1.000000000000000000, 0.8660254037844387076, 1.000000000000000000, 0.8660254037844387076, 1.000000000000000000, 0.8660254037844387076, 1.000000000000000000, 0.8660254037844387076, 1.000000000000000000, 0.8660254037844387076, 1.000000000000000000, 0.8660254037844387076, 1.000000000000000000, 0.8660254037844387076, 1.000000000000000000, 0.8660254037844387076, 1.000000000000000000, 0.8660254037844387076, 1.000000000000000000, 0.8660254037844387076, 1.000000000000000000, 0.8660254037844387076, 1.000000000000000000, 0.8660254037844387076, 1.000000000000000000, 0.8660254037844387076, 1.000000000000000000, 0.8660254037844387076, 1.000000000000000000, 0.8660254037844387076, 1.000000000000000000, 0.8660254037844387076, 1.000000000000000000, 0.8660254037844387076, 1.000000000000000000, 0.8660254037844387076, 1.000000000000000000, 0.8660254037844387076, 1.000000000000000000, 0.8660254037844387076, 1.000000000000000000, 0.8660254037844387076, 1.000000000000000000, 0.8660254037844387076, 1.000000000000000000, 0.8660254037844387076, 1.000000000000000000, 0.8660254037844387076, 1.000000000000000000, 0.8660254037844387076, 1.000000000000000000, 0.8660254037844387076, 1.000000000000000000, 0.8660254037844387076, 1.000000000000000000, 0.8660254037844387076, 1.000000000000000000, 0.8660254037844387076, 1.000000000000000000, 0.8660254037844387076, 1.000000000000000000, 0.8660254037844387076, 1.000000000000000000, 0.8660254037844387076, 1.000000000000000000, 0.8660254037844387076, 1.000000000000000000, 0.8660254037844387076, 1.000000000000000000, 0.8660254037844387076, 1.000000000000000000, 0.8660254037844387076, 1.000000000000000000) ) ) 
 REPRESENTATION_ITEM ( '' )  SURFACE ( )  );
#37587 = EDGE_LOOP ( 'NONE', ( #103542, #96904 ) ) ;
#37588 = ADVANCED_FACE ( 'NONE', ( #65013 ), #5438, .T. ) ;
#37589 = ORIENTED_EDGE ( 'NONE', *, *, #39262, .T. ) ;
#37590 = FACE_OUTER_BOUND ( 'NONE', #1818, .T. ) ;
#37591 = DIRECTION ( 'NONE',  ( 0.000000000000000000, 0.000000000000000000, -1.000000000000000000 ) ) ;
#37592 = CARTESIAN_POINT ( 'NONE',  ( 10.64999999999990976, 12.50000000000000000, -6.148780366869526226 ) ) ;
#37593 = CARTESIAN_POINT ( 'NONE',  ( 10.44999999999991047, 2.500000000000000000, 2.165063509461097713 ) ) ;
#37594 = DIRECTION ( 'NONE',  ( 0.000000000000000000, 1.000000000000000000, 0.000000000000000000 ) ) ;
#37595 = CIRCLE ( 'NONE', #46001, 0.1000000000000000472 ) ;
#37596 = ORIENTED_EDGE ( 'NONE', *, *, #63257, .F. ) ;
#37597 = DIRECTION ( 'NONE',  ( -0.000000000000000000, 1.000000000000000000, -0.000000000000000000 ) ) ;
#37598 = ORIENTED_EDGE ( 'NONE', *, *, #8608, .F. ) ;
#37599 = CARTESIAN_POINT ( 'NONE',  ( 2.699999999999947331, 12.50000000000000000, -4.741630453620016006 ) ) ;
#37601 = CONICAL_SURFACE ( 'NONE', #83568, 0.1000000000000002554, 0.003490658503988666988 ) ;
#37600 = AXIS2_PLACEMENT_3D ( 'NONE', #14098, #64499, #34423 ) ;
#37602 = ORIENTED_EDGE ( 'NONE', *, *, #57130, .F. ) ;
#37603 = DIRECTION ( 'NONE',  ( -0.000000000000000000, 1.000000000000000000, -0.000000000000000000 ) ) ;
#37604 = CARTESIAN_POINT ( 'NONE',  ( 21.24754738303276724, -0.7337760880902383098, -4.182111650399352953 ) ) ;
#37605 = ORIENTED_EDGE ( 'NONE', *, *, #123327, .F. ) ;
#37606 = CIRCLE ( 'NONE', #129561, 0.06509327318403745899 ) ;
#37607 = CARTESIAN_POINT ( 'NONE',  ( -1.250000000000037970, 2.500000000000000000, 2.857883832488649301 ) ) ;
#37608 = CARTESIAN_POINT ( 'NONE',  ( -11.64999999999999680, 2.500000000000000000, -2.065063509461098068 ) ) ;
#37609 = ORIENTED_EDGE ( 'NONE', *, *, #73892, .F. ) ;
#37611 = AXIS2_PLACEMENT_3D ( 'NONE', #21713, #61642, #101561 ) ;
#37610 = CIRCLE ( 'NONE', #48073, 0.1000000000000000472 ) ;
#37612 = ADVANCED_FACE ( 'NONE', ( #5459 ), #70205, .T. ) ;
#37613 = CARTESIAN_POINT ( 'NONE',  ( 9.399999999999915090, 2.500000000000000000, -3.883716857408426648 ) ) ;
#37614 = ORIENTED_EDGE ( 'NONE', *, *, #45039, .F. ) ;
#37615 = ORIENTED_EDGE ( 'NONE', *, *, #47813, .F. ) ;
#37616 = DIRECTION ( 'NONE',  ( 0.000000000000000000, 1.000000000000000000, 0.000000000000000000 ) ) ;
#37617 = DIRECTION ( 'NONE',  ( 0.000000000000000000, 0.000000000000000000, 1.000000000000000000 ) ) ;
#37618 = EDGE_CURVE ( 'NONE', #88926, #110204, #105804, .T. ) ;
#37619 = CARTESIAN_POINT ( 'NONE',  ( 186.5468750003414300, -8.734944146203032389, -1.604583208406768146E-15 ) ) ;
#37620 = FACE_OUTER_BOUND ( 'NONE', #43495, .T. ) ;
#37621 = EDGE_CURVE ( 'NONE', #121105, #59532, #13751, .T. ) ;
#37622 = CARTESIAN_POINT ( 'NONE',  ( -10.40000000000000213, 12.50000000000000000, -4.330127018922197202 ) ) ;
#37623 = PLANE ( 'NONE',  #655 ) ;
#37624 = EDGE_CURVE ( 'NONE', #104601, #102213, #59764, .T. ) ;
#37625 = ADVANCED_FACE ( 'NONE', ( #58459 ), #51443, .T. ) ;
#37626 = EDGE_CURVE ( 'NONE', #103846, #38154, #91130, .T. ) ;
#37627 = ORIENTED_EDGE ( 'NONE', *, *, #29196, .F. ) ;
#37628 = CARTESIAN_POINT ( 'NONE',  ( -4.550000000000026468, 12.50000000000000000, -6.560283801567339701 ) ) ;
#37629 = AXIS2_PLACEMENT_3D ( 'NONE', #53256, #32350, #82728 ) ;
#37630 = FACE_OUTER_BOUND ( 'NONE', #15160, .T. ) ;
#37631 = CIRCLE ( 'NONE', #96185, 0.1000000000000002554 ) ;
#37632 = VERTEX_POINT ( 'NONE', #147 ) ;
#37633 = EDGE_CURVE ( 'NONE', #51388, #17427, #107854, .T. ) ;
#37634 = CARTESIAN_POINT ( 'NONE',  ( -14.99999999999994671, 2.500000000000000000, 0.000000000000000000 ) ) ;
#37635 = PLANE ( 'NONE',  #5031 ) ;
#37636 = CARTESIAN_POINT ( 'NONE',  ( 11.04999999999991012, 12.50000000000000000, -1.818653347947326138 ) ) ;
#37637 = DIRECTION ( 'NONE',  ( -0.000000000000000000, -1.000000000000000000, -0.000000000000000000 ) ) ;
#37638 = CARTESIAN_POINT ( 'NONE',  ( -15.39999999999997904, 12.50000000000000000, -0.6928203230275519209 ) ) ;
#37639 = ORIENTED_EDGE ( 'NONE', *, *, #60099, .F. ) ;
#37641 = ADVANCED_FACE ( 'NONE', ( #70840 ), #126645, .T. ) ;
#37640 = AXIS2_PLACEMENT_3D ( 'NONE', #11157, #51111, #89091 ) ;
#37642 = EDGE_CURVE ( 'NONE', #44029, #14513, #128501, .T. ) ;
#37643 = CARTESIAN_POINT ( 'NONE',  ( 2.049999999999950084, 2.500000000000000000, -2.165063509461101710 ) ) ;
#37644 = VECTOR ( 'NONE', #86439, 1000.000000000000000 ) ;
#37645 = ORIENTED_EDGE ( 'NONE', *, *, #9624, .F. ) ;
#37646 = CARTESIAN_POINT ( 'NONE',  ( 3.949999999999941558, 12.50000000000000000, -6.213873640053564351 ) ) ;
#37647 = AXIS2_PLACEMENT_3D ( 'NONE', #80620, #79961, #40047 ) ;
#37648 = EDGE_LOOP ( 'NONE', ( #54342, #1454, #43438, #29340 ) ) ;
#37649 = PRODUCT_DEFINITION_SHAPE ( 'NONE', 'NONE',  #5236 ) ;
#37650 = ORIENTED_EDGE ( 'NONE', *, *, #79157, .F. ) ;
#37651 = DIRECTION ( 'NONE',  ( -0.000000000000000000, -1.000000000000000000, -0.000000000000000000 ) ) ;
#37652 = CONICAL_SURFACE ( 'NONE', #77358, 0.1000000000000000472, 0.003490658503988666988 ) ;
#37653 = ORIENTED_EDGE ( 'NONE', *, *, #102157, .F. ) ;
#37654 = LINE ( 'NONE', #36372, #82064 ) ;
#37655 = CARTESIAN_POINT ( 'NONE',  ( 8.749999999999920064, 12.50000000000000000, -2.857883832488653741 ) ) ;
#37656 = CIRCLE ( 'NONE', #22984, 0.06509327318403745899 ) ;
#37657 = DIRECTION ( 'NONE',  ( -4.274815082592931898E-19, -0.9999939076577903929, -0.003490651415223739937 ) ) ;
#37658 = VERTEX_POINT ( 'NONE', #99668 ) ;
#37659 = FACE_BOUND ( 'NONE', #1520, .T. ) ;
#37661 = ORIENTED_EDGE ( 'NONE', *, *, #106115, .T. ) ;
#37660 = LINE ( 'NONE', #19276, #51518 ) ;
#37662 = CIRCLE ( 'NONE', #52318, 0.06509327318403741736 ) ;
#37663 = CARTESIAN_POINT ( 'NONE',  ( -11.24999999999999822, 2.500000000000000000, 1.572243186433545548 ) ) ;
#37664 = DIRECTION ( 'NONE',  ( 0.000000000000000000, 1.000000000000000000, 0.000000000000000000 ) ) ;
#37665 = ORIENTED_EDGE ( 'NONE', *, *, #82669, .T. ) ;
#37667 = EDGE_LOOP ( 'NONE', ( #50089, #99755, #58404, #85578 ) ) ;
#37666 = EDGE_CURVE ( 'NONE', #48297, #125237, #94162, .T. ) ;
#37668 = EDGE_LOOP ( 'NONE', ( #5463, #56220, #14950, #97158 ) ) ;
#37669 = CARTESIAN_POINT ( 'NONE',  ( 0.3999999999999559464, 2.500000000000000000, -4.330127018922201643 ) ) ;
#37670 = DIRECTION ( 'NONE',  ( 0.000000000000000000, 0.000000000000000000, 1.000000000000000000 ) ) ;
#37671 = CARTESIAN_POINT ( 'NONE',  ( -6.050000000000020250, 2.500000000000000000, -6.741600689897078169 ) ) ;
#37672 = FACE_BOUND ( 'NONE', #91917, .T. ) ;
#37673 = ORIENTED_EDGE ( 'NONE', *, *, #126112, .T. ) ;
#37674 = DIRECTION ( 'NONE',  ( -0.000000000000000000, -1.000000000000000000, -0.000000000000000000 ) ) ;
#37675 = CARTESIAN_POINT ( 'NONE',  ( 0.1999999999999567124, 12.50000000000000000, -3.983716857408426293 ) ) ;
#37676 = ORIENTED_EDGE ( 'NONE', *, *, #110636, .T. ) ;
#37677 = ADVANCED_FACE ( 'NONE', ( #92403 ), #86917, .T. ) ;
#37678 = DIRECTION ( 'NONE',  ( 0.000000000000000000, 0.000000000000000000, 1.000000000000000000 ) ) ;
#37680 = DIRECTION ( 'NONE',  ( -4.274815082592931898E-19, -0.9999939076577903929, -0.003490651415223739937 ) ) ;
#37679 = CIRCLE ( 'NONE', #48140, 0.1000000000000000472 ) ;
#37681 = DIRECTION ( 'NONE',  ( 0.000000000000000000, -0.000000000000000000, 1.000000000000000000 ) ) ;
#37682 = CARTESIAN_POINT ( 'NONE',  ( -8.350000000000012079, 12.50000000000000000, -1.472243186433550122 ) ) ;
#37683 = CARTESIAN_POINT ( 'NONE',  ( -8.350000000000008527, 2.500000000000000000, 5.902370205355745192 ) ) ;
#37685 = CIRCLE ( 'NONE', #127565, 0.09999999999999982514 ) ;
#37684 = AXIS2_PLACEMENT_3D ( 'NONE', #93184, #44066, #92517 ) ;
#37686 = EDGE_LOOP ( 'NONE', ( #40307, #53339, #125025, #90609 ) ) ;
#37687 = ORIENTED_EDGE ( 'NONE', *, *, #24616, .F. ) ;
#37688 = ORIENTED_EDGE ( 'NONE', *, *, #72322, .F. ) ;
#37689 = ORIENTED_EDGE ( 'NONE', *, *, #42302, .F. ) ;
#37690 = EDGE_LOOP ( 'NONE', ( #91030, #20740 ) ) ;
#37691 = DIRECTION ( 'NONE',  ( 0.000000000000000000, 0.000000000000000000, 1.000000000000000000 ) ) ;
#37692 = CARTESIAN_POINT ( 'NONE',  ( 0.8499999999999553468, 2.500000000000000000, 1.372243186433545370 ) ) ;
#37693 = ORIENTED_EDGE ( 'NONE', *, *, #74186, .F. ) ;
#37694 = FACE_BOUND ( 'NONE', #37498, .T. ) ;
#37695 = CARTESIAN_POINT ( 'NONE',  ( 4.149999999999936406, 12.50000000000000000, 6.495190528383297135 ) ) ;
#37696 = CIRCLE ( 'NONE', #25074, 0.06509327318403745899 ) ;
#37697 = FACE_OUTER_BOUND ( 'NONE', #60050, .T. ) ;
#37698 = CARTESIAN_POINT ( 'NONE',  ( 184.4999999999999716, -4.613861370277991369, 6.083321009326518869 ) ) ;
#37699 = FACE_OUTER_BOUND ( 'NONE', #80819, .T. ) ;
#37700 = CARTESIAN_POINT ( 'NONE',  ( 11.24999999999994493, 12.50000000000000000, -2.165063509461101710 ) ) ;
#37701 = ORIENTED_EDGE ( 'NONE', *, *, #75144, .T. ) ;
#37702 = CARTESIAN_POINT ( 'NONE',  ( -1.650000000000034328, 12.50000000000000000, -2.857883832488653741 ) ) ;
#37703 = EDGE_LOOP ( 'NONE', ( #43721, #45319 ) ) ;
#37704 = EDGE_LOOP ( 'NONE', ( #75417, #15193, #118937, #51004 ) ) ;
#37705 = VERTEX_POINT ( 'NONE', #101594 ) ;
#37706 = DIRECTION ( 'NONE',  ( 0.000000000000000000, 0.000000000000000000, -1.000000000000000000 ) ) ;
#37707 = CARTESIAN_POINT ( 'NONE',  ( 13.74999999999993072, 12.50000000000000000, -2.165063509461101710 ) ) ;
#37708 = DIRECTION ( 'NONE',  ( -0.000000000000000000, -1.000000000000000000, -0.000000000000000000 ) ) ;
#37709 = ORIENTED_EDGE ( 'NONE', *, *, #22655, .F. ) ;
#37710 = DIRECTION ( 'NONE',  ( -0.000000000000000000, 1.000000000000000000, -0.000000000000000000 ) ) ;
#37711 = VECTOR ( 'NONE', #115806, 1000.000000000000000 ) ;
#37712 = EDGE_CURVE ( 'NONE', #116743, #118512, #95340, .T. ) ;
#37713 = CARTESIAN_POINT ( 'NONE',  ( 14.34999999999989306, 2.500000000000000000, -2.411473670974877859 ) ) ;
#37714 = CONICAL_SURFACE ( 'NONE', #41926, 0.1000000000000002554, 0.003490658503988666988 ) ;
#37715 = DIRECTION ( 'NONE',  ( 0.000000000000000000, 0.000000000000000000, 1.000000000000000000 ) ) ;
#37716 = CARTESIAN_POINT ( 'NONE',  ( 184.2812500006828031, 0.000000000000000000, 7.700000000000000178 ) ) ;
#37717 = CARTESIAN_POINT ( 'NONE',  ( -1.850000000000033840, 2.500000000000000000, 6.741600689897071952 ) ) ;
#37718 = CARTESIAN_POINT ( 'NONE',  ( 2.099999999999948574, 2.500000000000000000, 3.537306695894645081 ) ) ;
#37719 = EDGE_CURVE ( 'NONE', #7038, #13274, #11268, .T. ) ;
#37720 = CARTESIAN_POINT ( 'NONE',  ( -4.400000000000025224, 12.50000000000000000, 0.4115034346978109769 ) ) ;
#37721 = EDGE_CURVE ( 'NONE', #64904, #116433, #82608, .T. ) ;
#37722 = ORIENTED_EDGE ( 'NONE', *, *, #32378, .F. ) ;
#37723 = LINE ( 'NONE', #67143, #100631 ) ;
#37724 = EDGE_LOOP ( 'NONE', ( #2338, #93113, #66190, #51102 ) ) ;
#37725 = EDGE_LOOP ( 'NONE', ( #64706, #42635, #115522, #126990 ) ) ;
#37726 = CARTESIAN_POINT ( 'NONE',  ( -12.69999999999999396, 12.50000000000000000, -3.983716857408423628 ) ) ;
#37727 = EDGE_CURVE ( 'NONE', #127628, #93079, #103529, .T. ) ;
#37728 = EDGE_CURVE ( 'NONE', #89461, #129332, #47232, .T. ) ;
#37729 = FACE_OUTER_BOUND ( 'NONE', #74583, .T. ) ;
#37730 = DIRECTION ( 'NONE',  ( -0.000000000000000000, -1.000000000000000000, -0.000000000000000000 ) ) ;
#37731 = EDGE_CURVE ( 'NONE', #26373, #57597, #113333, .T. ) ;
#37732 = EDGE_LOOP ( 'NONE', ( #39375, #78965 ) ) ;
#37733 = VERTEX_POINT ( 'NONE', #52479 ) ;
#37734 = VECTOR ( 'NONE', #24262, 1000.000000000000000 ) ;
#37735 = DIRECTION ( 'NONE',  ( 0.000000000000000000, 0.000000000000000000, 1.000000000000000000 ) ) ;
#37736 = CONICAL_SURFACE ( 'NONE', #112949, 0.09999999999999982514, 0.003490658503988666988 ) ;
#37737 = CARTESIAN_POINT ( 'NONE',  ( -13.14999999999999147, 2.500000000000000000, -2.511473670974875727 ) ) ;
#37738 = DIRECTION ( 'NONE',  ( 0.000000000000000000, 1.000000000000000000, 0.000000000000000000 ) ) ;
#37739 = ORIENTED_EDGE ( 'NONE', *, *, #99809, .F. ) ;
#37740 = ORIENTED_EDGE ( 'NONE', *, *, #24299, .T. ) ;
#37741 = CARTESIAN_POINT ( 'NONE',  ( 10.64999999999991331, 2.500000000000000000, 6.048780366869521252 ) ) ;
#37742 = AXIS2_PLACEMENT_3D ( 'NONE', #43793, #61494, #13649 ) ;
#37743 = ORIENTED_EDGE ( 'NONE', *, *, #30138, .F. ) ;
#37744 = DIRECTION ( 'NONE',  ( 0.000000000000000000, 0.000000000000000000, 1.000000000000000000 ) ) ;
#37745 = DIRECTION ( 'NONE',  ( 0.000000000000000000, 0.000000000000000000, 1.000000000000000000 ) ) ;
#37746 = ORIENTED_EDGE ( 'NONE', *, *, #38818, .F. ) ;
#37747 = CARTESIAN_POINT ( 'NONE',  ( 4.599999999999940137, 2.500000000000000000, -4.230127018922201998 ) ) ;
#37748 = DIRECTION ( 'NONE',  ( 0.000000000000000000, -0.9999939076577903929, 0.003490651415223739937 ) ) ;
#37749 = AXIS2_PLACEMENT_3D ( 'NONE', #46198, #77579, #66477 ) ;
#37750 = CARTESIAN_POINT ( 'NONE',  ( -9.800000000000006040, 12.50000000000000000, 4.676537180435972552 ) ) ;
#37751 = CARTESIAN_POINT ( 'NONE',  ( -8.550000000000011369, 2.500000000000000000, -2.611473670974877592 ) ) ;
#37752 = ORIENTED_EDGE ( 'NONE', *, *, #27510, .T. ) ;
#37753 = DIRECTION ( 'NONE',  ( 0.000000000000000000, 1.000000000000000000, 0.000000000000000000 ) ) ;
#37754 = ORIENTED_EDGE ( 'NONE', *, *, #124478, .F. ) ;
#37755 = EDGE_LOOP ( 'NONE', ( #61891, #37044, #51594, #112638 ) ) ;
#37756 = DIRECTION ( 'NONE',  ( 0.000000000000000000, 0.000000000000000000, -1.000000000000000000 ) ) ;
#37757 = DIRECTION ( 'NONE',  ( -4.274815082592931898E-19, -0.9999939076577903929, -0.003490651415223739937 ) ) ;
#37758 = DIRECTION ( 'NONE',  ( 0.000000000000000000, -0.000000000000000000, 1.000000000000000000 ) ) ;
#37759 = DIRECTION ( 'NONE',  ( -0.000000000000000000, -1.000000000000000000, -0.000000000000000000 ) ) ;
#37760 = CARTESIAN_POINT ( 'NONE',  ( -5.600000000000020073, 2.500000000000000000, 4.083716857408421497 ) ) ;
#37761 = PLANE ( 'NONE',  #77940 ) ;
#37762 = CARTESIAN_POINT ( 'NONE',  ( 16.32360635139512794, 2.500000000000000000, -4.874197684301369016 ) ) ;
#37763 = CARTESIAN_POINT ( 'NONE',  ( -8.950000000000009948, 12.50000000000000000, -6.841600689897072485 ) ) ;
#37764 = CARTESIAN_POINT ( 'NONE',  ( -4.999999999999986677, 12.50000000000000000, 0.06509327318403515528 ) ) ;
#37766 = EDGE_CURVE ( 'NONE', #62255, #54077, #1447, .T. ) ;
#37765 = CONICAL_SURFACE ( 'NONE', #121375, 0.09999999999999982514, 0.003490658503988666988 ) ;
#37767 = AXIS2_PLACEMENT_3D ( 'NONE', #31020, #82019, #72220 ) ;
#37768 = ADVANCED_FACE ( 'NONE', ( #112706 ), #112064, .T. ) ;
#37769 = VECTOR ( 'NONE', #2970, 1000.000000000000000 ) ;
#37770 = ADVANCED_FACE ( 'NONE', ( #23033 ), #112060, .T. ) ;
#37771 = DIRECTION ( 'NONE',  ( 0.000000000000000000, 0.000000000000000000, 1.000000000000000000 ) ) ;
#37772 = CIRCLE ( 'NONE', #110911, 0.1000000000000000472 ) ;
#37773 = VERTEX_POINT ( 'NONE', #81934 ) ;
#37774 = EDGE_CURVE ( 'NONE', #93396, #37336, #101602, .T. ) ;
#37775 = DIRECTION ( 'NONE',  ( -0.000000000000000000, -1.000000000000000000, -0.000000000000000000 ) ) ;
#37776 = ADVANCED_FACE ( 'NONE', ( #83251 ), #105890, .T. ) ;
#37777 = DIRECTION ( 'NONE',  ( 0.000000000000000000, 0.000000000000000000, -1.000000000000000000 ) ) ;
#37778 = DIRECTION ( 'NONE',  ( 0.000000000000000000, -0.000000000000000000, 1.000000000000000000 ) ) ;
#37779 = DIRECTION ( 'NONE',  ( 0.000000000000000000, 0.000000000000000000, 1.000000000000000000 ) ) ;
#37780 = CARTESIAN_POINT ( 'NONE',  ( 1.899999999999949507, 12.50000000000000000, 3.918623584224383727 ) ) ;
#37781 = VERTEX_POINT ( 'NONE', #73407 ) ;
#37782 = EDGE_CURVE ( 'NONE', #77609, #91178, #59863, .T. ) ;
#37783 = CARTESIAN_POINT ( 'NONE',  ( -0.4000000000000392131, 12.50000000000000000, -4.395220292106239768 ) ) ;
#37784 = EDGE_CURVE ( 'NONE', #81286, #122177, #93282, .T. ) ;
#37785 = DIRECTION ( 'NONE',  ( 0.000000000000000000, -0.000000000000000000, 1.000000000000000000 ) ) ;
#37787 = VERTEX_POINT ( 'NONE', #4019 ) ;
#37786 = DIRECTION ( 'NONE',  ( 0.000000000000000000, 0.000000000000000000, 1.000000000000000000 ) ) ;
#37788 = EDGE_CURVE ( 'NONE', #108866, #39483, #95431, .T. ) ;
#37789 = ORIENTED_EDGE ( 'NONE', *, *, #111177, .F. ) ;
#37790 = VERTEX_POINT ( 'NONE', #111389 ) ;
#37791 = ORIENTED_EDGE ( 'NONE', *, *, #91416, .F. ) ;
#37792 = ORIENTED_EDGE ( 'NONE', *, *, #98150, .T. ) ;
#37793 = DIRECTION ( 'NONE',  ( -4.274815082592931898E-19, -0.9999939076577903929, -0.003490651415223739937 ) ) ;
#37794 = DIRECTION ( 'NONE',  ( 0.000000000000000000, 1.000000000000000000, 0.000000000000000000 ) ) ;
#37795 = DIRECTION ( 'NONE',  ( 0.000000000000000000, 1.000000000000000000, 0.000000000000000000 ) ) ;
#37796 = CARTESIAN_POINT ( 'NONE',  ( 5.199999999999935341, 2.500000000000000000, -0.2464101615137783419 ) ) ;
#37797 = CIRCLE ( 'NONE', #77504, 0.1000000000000002554 ) ;
#37798 = ORIENTED_EDGE ( 'NONE', *, *, #68730, .T. ) ;
#37799 = CIRCLE ( 'NONE', #121415, 0.06509327318403741736 ) ;
#37800 = LINE ( 'NONE', #126829, #96279 ) ;
#37801 = ORIENTED_EDGE ( 'NONE', *, *, #115587, .T. ) ;
#37802 = DIRECTION ( 'NONE',  ( -0.000000000000000000, 1.000000000000000000, -0.000000000000000000 ) ) ;
#37803 = CARTESIAN_POINT ( 'NONE',  ( 14.38463633427091892, -1.499999999999742428, -7.683002070838238495 ) ) ;
#37804 = DIRECTION ( 'NONE',  ( 0.000000000000000000, 0.000000000000000000, -1.000000000000000000 ) ) ;
#37805 = CARTESIAN_POINT ( 'NONE',  ( 12.89999999999990266, 2.500000000000000000, 3.537306695894645081 ) ) ;
#37806 = DIRECTION ( 'NONE',  ( 0.000000000000000000, 0.000000000000000000, 1.000000000000000000 ) ) ;
#37807 = AXIS2_PLACEMENT_3D ( 'NONE', #92048, #2355, #42318 ) ;
#37808 = ORIENTED_EDGE ( 'NONE', *, *, #88399, .F. ) ;
#37809 = AXIS2_PLACEMENT_3D ( 'NONE', #100213, #9896, #99581 ) ;
#37810 = EDGE_LOOP ( 'NONE', ( #100343, #74445 ) ) ;
#37811 = ORIENTED_EDGE ( 'NONE', *, *, #87661, .T. ) ;
#37812 = ORIENTED_EDGE ( 'NONE', *, *, #102449, .F. ) ;
#37813 = CARTESIAN_POINT ( 'NONE',  ( 13.14999999999990088, 2.500000000000000000, 1.818653347947321475 ) ) ;
#37814 = LINE ( 'NONE', #18808, #51950 ) ;
#37815 = CARTESIAN_POINT ( 'NONE',  ( -4.119968255444916849E-14, 2.500000000000000000, 3.637306695894644726 ) ) ;
#37816 = FACE_BOUND ( 'NONE', #68132, .T. ) ;
#37817 = CARTESIAN_POINT ( 'NONE',  ( 0.6499999999999561684, 2.500000000000000000, -2.411473670974877859 ) ) ;
#37818 = CARTESIAN_POINT ( 'NONE',  ( -3.350000000000032507, 2.500000000000000000, -6.495190528383302464 ) ) ;
#37819 = CARTESIAN_POINT ( 'NONE',  ( -2.100000000000034284, 2.500000000000000000, -2.385244779468109755E-15 ) ) ;
#37820 = CARTESIAN_POINT ( 'NONE',  ( 6.449999999999928235, 2.500000000000000000, 2.411473670974873862 ) ) ;
#37821 = AXIS2_PLACEMENT_3D ( 'NONE', #39905, #90251, #30087 ) ;
#37822 = CONICAL_SURFACE ( 'NONE', #90034, 0.1000000000000002554, 0.003490658503988666988 ) ;
#37823 = EDGE_CURVE ( 'NONE', #88819, #124287, #55708, .T. ) ;
#37824 = CARTESIAN_POINT ( 'NONE',  ( 185.1718750003414016, 9.264065473108010111E-16, -7.564683531250000925 ) ) ;
#37825 = CARTESIAN_POINT ( 'NONE',  ( 9.599999999999914380, 2.500000000000000000, -5.122947341949753763 ) ) ;
#37826 = DIRECTION ( 'NONE',  ( 0.000000000000000000, 0.000000000000000000, 1.000000000000000000 ) ) ;
#37827 = CONICAL_SURFACE ( 'NONE', #71267, 0.09999999999999982514, 0.003490658503988666988 ) ;
#37828 = CARTESIAN_POINT ( 'NONE',  ( 3.149999999999946176, 2.500000000000000000, -6.841600689897077814 ) ) ;
#37829 = ORIENTED_EDGE ( 'NONE', *, *, #24437, .T. ) ;
#37830 = CIRCLE ( 'NONE', #100520, 0.1000000000000002554 ) ;
#37831 = ORIENTED_EDGE ( 'NONE', *, *, #47397, .T. ) ;
#37832 = ORIENTED_EDGE ( 'NONE', *, *, #102627, .F. ) ;
#37833 = EDGE_LOOP ( 'NONE', ( #113713, #112076, #44669, #41596 ) ) ;
#37834 = DIRECTION ( 'NONE',  ( 0.000000000000000000, -0.000000000000000000, 1.000000000000000000 ) ) ;
#37835 = FACE_BOUND ( 'NONE', #3401, .T. ) ;
#37836 = LINE ( 'NONE', #128833, #122998 ) ;
#37837 = ORIENTED_EDGE ( 'NONE', *, *, #30085, .T. ) ;
#37838 = CARTESIAN_POINT ( 'NONE',  ( -2.499999999999996003, 2.500000000000000000, -2.276824562219559311E-15 ) ) ;
#37839 = LINE ( 'NONE', #77751, #129401 ) ;
#37840 = CARTESIAN_POINT ( 'NONE',  ( -14.34999999999998543, 12.50000000000000000, -1.818653347947323695 ) ) ;
#37841 = ORIENTED_EDGE ( 'NONE', *, *, #77747, .T. ) ;
#37842 = CARTESIAN_POINT ( 'NONE',  ( -2.950000000000029932, 2.500000000000000000, -2.065063509461102065 ) ) ;
#37843 = DIRECTION ( 'NONE',  ( -0.000000000000000000, 1.000000000000000000, -0.000000000000000000 ) ) ;
#37844 = VERTEX_POINT ( 'NONE', #21749 ) ;
#37845 = CIRCLE ( 'NONE', #2327, 0.09999999999999999167 ) ;
#37846 = ORIENTED_EDGE ( 'NONE', *, *, #67851, .T. ) ;
#37847 = AXIS2_PLACEMENT_3D ( 'NONE', #115318, #34237, #54490 ) ;
#37848 = DIRECTION ( 'NONE',  ( -0.000000000000000000, -1.000000000000000000, -0.000000000000000000 ) ) ;
#37849 = DIRECTION ( 'NONE',  ( 0.000000000000000000, 0.000000000000000000, 1.000000000000000000 ) ) ;
#37850 = EDGE_CURVE ( 'NONE', #98051, #4680, #61682, .T. ) ;
#37851 = DIRECTION ( 'NONE',  ( -0.000000000000000000, -1.000000000000000000, -0.000000000000000000 ) ) ;
#37852 = AXIS2_PLACEMENT_3D ( 'NONE', #27470, #67374, #47784 ) ;
#37853 = FACE_OUTER_BOUND ( 'NONE', #76834, .T. ) ;
#37854 = VERTEX_POINT ( 'NONE', #26259 ) ;
#37855 = DIRECTION ( 'NONE',  ( -0.000000000000000000, 1.000000000000000000, -0.000000000000000000 ) ) ;
#37856 = VERTEX_POINT ( 'NONE', #56343 ) ;
#37857 = AXIS2_PLACEMENT_3D ( 'NONE', #129356, #97928, #128719 ) ;
#37858 = ORIENTED_EDGE ( 'NONE', *, *, #80176, .T. ) ;
#37859 = ADVANCED_FACE ( 'NONE', ( #18839 ), #39030, .T. ) ;
#37860 = DIRECTION ( 'NONE',  ( 0.000000000000000000, 0.000000000000000000, -1.000000000000000000 ) ) ;
#37861 = ADVANCED_FACE ( 'NONE', ( #113992 ), #114212, .T. ) ;
#37862 = ORIENTED_EDGE ( 'NONE', *, *, #29029, .F. ) ;
#37863 = DIRECTION ( 'NONE',  ( 0.000000000000000000, 0.000000000000000000, 1.000000000000000000 ) ) ;
#37864 = FACE_BOUND ( 'NONE', #129466, .T. ) ;
#37865 = ORIENTED_EDGE ( 'NONE', *, *, #19775, .F. ) ;
#37866 = DIRECTION ( 'NONE',  ( 0.000000000000000000, -0.9999939076577903929, 0.003490651415223739937 ) ) ;
#37867 = VERTEX_POINT ( 'NONE', #74062 ) ;
#37868 = DIRECTION ( 'NONE',  ( 0.000000000000000000, -1.000000000000000000, 0.000000000000000000 ) ) ;
#37869 = CARTESIAN_POINT ( 'NONE',  ( -11.64999999999999680, 2.500000000000000000, -2.265063509461097802 ) ) ;
#37870 = EDGE_CURVE ( 'NONE', #120381, #98606, #58778, .T. ) ;
#37871 = ADVANCED_FACE ( 'NONE', ( #75990 ), #5527, .T. ) ;
#37872 = CARTESIAN_POINT ( 'NONE',  ( -9.200000000000006395, 12.50000000000000000, -2.385244779468109755E-15 ) ) ;
#37873 = EDGE_CURVE ( 'NONE', #2890, #74712, #128907, .T. ) ;
#37874 = DIRECTION ( 'NONE',  ( 0.000000000000000000, 0.000000000000000000, 1.000000000000000000 ) ) ;
#37875 = EDGE_CURVE ( 'NONE', #84780, #86820, #48971, .T. ) ;
#37876 = EDGE_CURVE ( 'NONE', #27877, #54474, #64869, .T. ) ;
#37877 = DIRECTION ( 'NONE',  ( 0.000000000000000000, 0.000000000000000000, 1.000000000000000000 ) ) ;
#37878 = EDGE_LOOP ( 'NONE', ( #9663, #86161 ) ) ;
#37879 = VERTEX_POINT ( 'NONE', #54412 ) ;
#37880 = AXIS2_PLACEMENT_3D ( 'NONE', #78467, #67966, #128195 ) ;
#37881 = DIRECTION ( 'NONE',  ( -0.000000000000000000, -1.000000000000000000, -0.000000000000000000 ) ) ;
#37882 = CARTESIAN_POINT ( 'NONE',  ( 18.29531403502771525, -0.5011766475904755325, 4.780851392375801368 ) ) ;
#37883 = CARTESIAN_POINT ( 'NONE',  ( -5.200000000000025935, 2.500000000000000000, -3.883716857408426648 ) ) ;
#37885 = ORIENTED_EDGE ( 'NONE', *, *, #66007, .T. ) ;
#37884 = ORIENTED_EDGE ( 'NONE', *, *, #124967, .T. ) ;
#37886 = ORIENTED_EDGE ( 'NONE', *, *, #74556, .F. ) ;
#37887 = EDGE_CURVE ( 'NONE', #27095, #86001, #97484, .T. ) ;
#37888 = CARTESIAN_POINT ( 'NONE',  ( 12.09999999999990550, 2.500000000000000000, 5.022947341949748790 ) ) ;
#37889 = LINE ( 'NONE', #80408, #4657 ) ;
#37890 = CONICAL_SURFACE ( 'NONE', #2354, 0.1000000000000002554, 0.003490658503988666988 ) ;
#37891 = DIRECTION ( 'NONE',  ( -0.000000000000000000, 1.000000000000000000, -0.000000000000000000 ) ) ;
#37892 = CARTESIAN_POINT ( 'NONE',  ( -0.4500000000000397571, 2.500000000000000000, -6.495190528383302464 ) ) ;
#37893 = DIRECTION ( 'NONE',  ( 1.000000000000000000, -0.000000000000000000, -0.000000000000000000 ) ) ;
#37894 = DIRECTION ( 'NONE',  ( 0.000000000000000000, 0.000000000000000000, -1.000000000000000000 ) ) ;
#37895 = DIRECTION ( 'NONE',  ( 0.000000000000000000, 0.000000000000000000, -1.000000000000000000 ) ) ;
#37897 = AXIS2_PLACEMENT_3D ( 'NONE', #101010, #121299, #61755 ) ;
#37896 = DIRECTION ( 'NONE',  ( -0.000000000000000000, 1.000000000000000000, -0.000000000000000000 ) ) ;
#37898 = VERTEX_POINT ( 'NONE', #5307 ) ;
#37899 = CIRCLE ( 'NONE', #125703, 0.09999999999999982514 ) ;
#37900 = ORIENTED_EDGE ( 'NONE', *, *, #124325, .T. ) ;
#37901 = DIRECTION ( 'NONE',  ( 0.000000000000000000, 0.000000000000000000, 1.000000000000000000 ) ) ;
#37902 = CARTESIAN_POINT ( 'NONE',  ( -1.450000000000035483, 2.500000000000000000, 1.918653347947321564 ) ) ;
#37903 = VERTEX_POINT ( 'NONE', #95000 ) ;
#37904 = VERTEX_POINT ( 'NONE', #94329 ) ;
#37905 = CARTESIAN_POINT ( 'NONE',  ( 186.4843750003414016, -8.734944146203032389, -1.604583208406768146E-15 ) ) ;
#37906 = CARTESIAN_POINT ( 'NONE',  ( 7.499999999999961808, 2.500000000000000000, 4.330127018922196314 ) ) ;
#37907 = FACE_OUTER_BOUND ( 'NONE', #25040, .T. ) ;
#37908 = CONICAL_SURFACE ( 'NONE', #25368, 0.09999999999999999167, 0.003490658503988666988 ) ;
#37909 = DIRECTION ( 'NONE',  ( 0.000000000000000000, 0.000000000000000000, -1.000000000000000000 ) ) ;
#37910 = VECTOR ( 'NONE', #93999, 1000.000000000000000 ) ;
#37911 = CARTESIAN_POINT ( 'NONE',  ( 3.149999999999942624, 2.500000000000000000, 6.048780366869521252 ) ) ;
#37912 = DIRECTION ( 'NONE',  ( -0.000000000000000000, 1.000000000000000000, -0.000000000000000000 ) ) ;
#37913 = CARTESIAN_POINT ( 'NONE',  ( -11.64999999999999680, 2.500000000000000000, 2.957883832488649389 ) ) ;
#37915 = ORIENTED_EDGE ( 'NONE', *, *, #18699, .F. ) ;
#37914 = AXIS2_PLACEMENT_3D ( 'NONE', #93331, #63220, #20725 ) ;
#37916 = DIRECTION ( 'NONE',  ( 0.000000000000000000, 1.000000000000000000, 0.000000000000000000 ) ) ;
#37917 = EDGE_CURVE ( 'NONE', #117010, #54102, #104167, .T. ) ;
#37918 = EDGE_CURVE ( 'NONE', #71367, #100917, #128167, .T. ) ;
#37919 = CONICAL_SURFACE ( 'NONE', #113126, 0.09999999999999999167, 0.003490658503988666988 ) ;
#37920 = ADVANCED_FACE ( 'NONE', ( #65522 ), #66170, .T. ) ;
#37921 = DIRECTION ( 'NONE',  ( -0.000000000000000000, -1.000000000000000000, -0.000000000000000000 ) ) ;
#37922 = ORIENTED_EDGE ( 'NONE', *, *, #28176, .F. ) ;
#37923 = EDGE_CURVE ( 'NONE', #84687, #36770, #82918, .T. ) ;
#37924 = AXIS2_PLACEMENT_3D ( 'NONE', #70204, #40103, #108178 ) ;
#37925 = CIRCLE ( 'NONE', #111054, 0.06509327318403745899 ) ;
#37926 = ORIENTED_EDGE ( 'NONE', *, *, #99591, .T. ) ;
#37927 = VERTEX_POINT ( 'NONE', #44604 ) ;
#37928 = EDGE_CURVE ( 'NONE', #89300, #73117, #11800, .T. ) ;
#37929 = VERTEX_POINT ( 'NONE', #105462 ) ;
#37930 = CARTESIAN_POINT ( 'NONE',  ( -8.100000000000013856, 2.500000000000000000, 0.2464101615137736789 ) ) ;
#37931 = FACE_OUTER_BOUND ( 'NONE', #126179, .T. ) ;
#37932 = ADVANCED_FACE ( 'NONE', ( #34803 ), #110017, .T. ) ;
#37933 = ORIENTED_EDGE ( 'NONE', *, *, #13087, .T. ) ;
#37934 = EDGE_CURVE ( 'NONE', #83506, #105517, #76559, .T. ) ;
#37935 = CARTESIAN_POINT ( 'NONE',  ( 4.549999999999939426, 2.500000000000000000, -2.165063509461101710 ) ) ;
#37936 = LINE ( 'NONE', #46454, #54928 ) ;
#37937 = EDGE_CURVE ( 'NONE', #885, #125076, #45259, .T. ) ;
#37938 = DIRECTION ( 'NONE',  ( 0.000000000000000000, 0.000000000000000000, -1.000000000000000000 ) ) ;
#37940 = ORIENTED_EDGE ( 'NONE', *, *, #92396, .T. ) ;
#37939 = DIRECTION ( 'NONE',  ( 0.000000000000000000, 0.000000000000000000, 1.000000000000000000 ) ) ;
#37941 = CARTESIAN_POINT ( 'NONE',  ( 8.149999999999920419, 12.50000000000000000, 6.841600689897072485 ) ) ;
#37942 = ADVANCED_FACE ( 'NONE', ( #8369 ), #48308, .F. ) ;
#37943 = CARTESIAN_POINT ( 'NONE',  ( 8.949999999999921130, 2.500000000000000000, 1.818653347947321475 ) ) ;
#37944 = VERTEX_POINT ( 'NONE', #101278 ) ;
#37945 = ORIENTED_EDGE ( 'NONE', *, *, #1919, .F. ) ;
#37946 = ORIENTED_EDGE ( 'NONE', *, *, #7591, .T. ) ;
#37947 = AXIS2_PLACEMENT_3D ( 'NONE', #11076, #619, #40586 ) ;
#37948 = CARTESIAN_POINT ( 'NONE',  ( 13.09999999999990195, 2.500000000000000000, 4.576537180435972019 ) ) ;
#37949 = AXIS2_PLACEMENT_3D ( 'NONE', #31485, #103933, #71384 ) ;
#37950 = CIRCLE ( 'NONE', #111078, 0.06509327318403745899 ) ;
#37951 = CARTESIAN_POINT ( 'NONE',  ( -2.100000000000033840, 2.500000000000000000, 5.022947341949748790 ) ) ;
#37952 = CIRCLE ( 'NONE', #67166, 0.1000000000000000472 ) ;
#37954 = EDGE_LOOP ( 'NONE', ( #90743, #62058, #71111, #17246 ) ) ;
#37953 = AXIS2_PLACEMENT_3D ( 'NONE', #111452, #112765, #10658 ) ;
#37955 = CARTESIAN_POINT ( 'NONE',  ( -3.150000000000030109, 2.500000000000000000, 1.818653347947321475 ) ) ;
#37956 = DIRECTION ( 'NONE',  ( 0.000000000000000000, 1.000000000000000000, 0.000000000000000000 ) ) ;
#37957 = CARTESIAN_POINT ( 'NONE',  ( 3.349999999999945466, 2.500000000000000000, -6.495190528383302464 ) ) ;
#37958 = DIRECTION ( 'NONE',  ( 0.000000000000000000, 0.000000000000000000, -1.000000000000000000 ) ) ;
#37959 = EDGE_CURVE ( 'NONE', #90001, #128895, #79073, .T. ) ;
#37960 = ORIENTED_EDGE ( 'NONE', *, *, #97864, .F. ) ;
#37961 = DIRECTION ( 'NONE',  ( 0.000000000000000000, -0.000000000000000000, 1.000000000000000000 ) ) ;
#37962 = ORIENTED_EDGE ( 'NONE', *, *, #10352, .F. ) ;
#37963 = ORIENTED_EDGE ( 'NONE', *, *, #89935, .T. ) ;
#37964 = CARTESIAN_POINT ( 'NONE',  ( -0.6500000000000389910, 12.50000000000000000, -6.148780366869526226 ) ) ;
#37965 = PLANE ( 'NONE',  #127618 ) ;
#37966 = FACE_BOUND ( 'NONE', #76791, .T. ) ;
#37967 = CARTESIAN_POINT ( 'NONE',  ( 17.50000000000000000, 2.500000000000000444, 4.040567763474975926 ) ) ;
#37968 = CARTESIAN_POINT ( 'NONE',  ( 8.749999999999953815, 12.50000000000000000, 6.560283801567334372 ) ) ;
#37969 = FACE_OUTER_BOUND ( 'NONE', #87337, .T. ) ;
#37970 = EDGE_CURVE ( 'NONE', #85122, #83523, #116254, .T. ) ;
#37971 = ORIENTED_EDGE ( 'NONE', *, *, #52578, .T. ) ;
#37972 = FACE_OUTER_BOUND ( 'NONE', #16201, .T. ) ;
#37973 = CARTESIAN_POINT ( 'NONE',  ( -1.650000000000035660, 12.50000000000000000, 2.857883832488649301 ) ) ;
#37974 = LINE ( 'NONE', #64849, #42490 ) ;
#37975 = DIRECTION ( 'NONE',  ( 0.000000000000000000, 0.000000000000000000, -1.000000000000000000 ) ) ;
#37976 = ORIENTED_EDGE ( 'NONE', *, *, #107530, .T. ) ;
#37977 = CIRCLE ( 'NONE', #25433, 0.06509327318403745899 ) ;
#37978 = CARTESIAN_POINT ( 'NONE',  ( -6.249999999999984901, 12.50000000000000000, -2.165063509461101710 ) ) ;
#37979 = CIRCLE ( 'NONE', #58826, 0.1000000000000002554 ) ;
#37980 = CARTESIAN_POINT ( 'NONE',  ( 0.4499999999999569344, 2.500000000000000000, 2.165063509461097713 ) ) ;
#37981 = EDGE_LOOP ( 'NONE', ( #4631, #73160, #73517, #60723 ) ) ;
#37982 = EDGE_LOOP ( 'NONE', ( #85227, #51048 ) ) ;
#37983 = DIRECTION ( 'NONE',  ( -0.000000000000000000, -1.000000000000000000, -0.000000000000000000 ) ) ;
#37984 = EDGE_CURVE ( 'NONE', #25471, #41232, #13844, .T. ) ;
#37985 = DIRECTION ( 'NONE',  ( 0.000000000000000000, -0.000000000000000000, 1.000000000000000000 ) ) ;
#37986 = FACE_BOUND ( 'NONE', #52497, .T. ) ;
#37987 = AXIS2_PLACEMENT_3D ( 'NONE', #31377, #33318, #101402 ) ;
#37988 = DIRECTION ( 'NONE',  ( 0.000000000000000000, 0.000000000000000000, -1.000000000000000000 ) ) ;
#37989 = ORIENTED_EDGE ( 'NONE', *, *, #35738, .T. ) ;
#37991 = CARTESIAN_POINT ( 'NONE',  ( -12.69999999999999041, 2.500000000000000000, 3.983716857408420964 ) ) ;
#37990 = AXIS2_PLACEMENT_3D ( 'NONE', #66575, #127449, #107142 ) ;
#37992 = ORIENTED_EDGE ( 'NONE', *, *, #18333, .T. ) ;
#37993 = VERTEX_POINT ( 'NONE', #62009 ) ;
#37994 = CARTESIAN_POINT ( 'NONE',  ( -10.60000000000000142, 12.50000000000000000, 3.983716857408420964 ) ) ;
#37995 = APPLICATION_CONTEXT ( 'automotive_design' ) ;
#37996 = CARTESIAN_POINT ( 'NONE',  ( 187.0416666666666288, -4.445597072760122614, 7.699999999999998401 ) ) ;
#37997 = EDGE_LOOP ( 'NONE', ( #117013, #77267 ) ) ;
#37999 = LINE ( 'NONE', #77280, #124190 ) ;
#37998 = AXIS2_PLACEMENT_3D ( 'NONE', #61311, #103157, #41686 ) ;
#38000 = LINE ( 'NONE', #17702, #97132 ) ;
#38001 = AXIS2_PLACEMENT_3D ( 'NONE', #46413, #35963, #123671 ) ;
#38002 = CONICAL_SURFACE ( 'NONE', #92367, 0.09999999999999999167, 0.003490658503988666988 ) ;
#38003 = CIRCLE ( 'NONE', #40169, 0.06509327318403741736 ) ;
#38004 = CONICAL_SURFACE ( 'NONE', #52676, 0.09999999999999982514, 0.003490658503988666988 ) ;
#38005 = DIRECTION ( 'NONE',  ( -0.000000000000000000, -1.000000000000000000, -0.000000000000000000 ) ) ;
#38006 = CARTESIAN_POINT ( 'NONE',  ( 7.099999999999926814, 2.500000000000000000, -2.276824562219559311E-15 ) ) ;
#38007 = AXIS2_PLACEMENT_3D ( 'NONE', #69694, #109629, #8187 ) ;
#38008 = ORIENTED_EDGE ( 'NONE', *, *, #103331, .T. ) ;
#38009 = EDGE_CURVE ( 'NONE', #17110, #106540, #70302, .T. ) ;
#38010 = SURFACE_STYLE_USAGE ( .BOTH. , #28846 ) ;
#38011 = AXIS2_PLACEMENT_3D ( 'NONE', #43971, #4647, #44607 ) ;
#38012 = DIRECTION ( 'NONE',  ( 0.000000000000000000, 0.000000000000000000, 1.000000000000000000 ) ) ;
#38013 = DIRECTION ( 'NONE',  ( 0.000000000000000000, 1.000000000000000000, 0.000000000000000000 ) ) ;
#38014 = DIRECTION ( 'NONE',  ( -0.000000000000000000, 1.000000000000000000, -0.000000000000000000 ) ) ;
#38015 = ORIENTED_EDGE ( 'NONE', *, *, #1235, .T. ) ;
#38016 = DIRECTION ( 'NONE',  ( -4.274815082592931898E-19, -0.9999939076577903929, -0.003490651415223739937 ) ) ;
#38017 = VERTEX_POINT ( 'NONE', #475 ) ;
#38018 = CARTESIAN_POINT ( 'NONE',  ( 1.699999999999951994, 12.50000000000000000, -4.265033745738164406 ) ) ;
#38019 = ORIENTED_EDGE ( 'NONE', *, *, #69500, .T. ) ;
#38020 = DIRECTION ( 'NONE',  ( -0.000000000000000000, 1.000000000000000000, -0.000000000000000000 ) ) ;
#38021 = DIRECTION ( 'NONE',  ( 0.000000000000000000, 1.000000000000000000, 0.000000000000000000 ) ) ;
#38022 = DIRECTION ( 'NONE',  ( 0.000000000000000000, 0.000000000000000000, -1.000000000000000000 ) ) ;
#38023 = DIRECTION ( 'NONE',  ( 0.000000000000000000, 0.000000000000000000, 1.000000000000000000 ) ) ;
#38024 = VERTEX_POINT ( 'NONE', #10930 ) ;
#38025 = DIRECTION ( 'NONE',  ( -1.000000000000000000, -0.000000000000000000, -0.000000000000000000 ) ) ;
#38026 = DIRECTION ( 'NONE',  ( -0.000000000000000000, 1.000000000000000000, -0.000000000000000000 ) ) ;
#38027 = EDGE_CURVE ( 'NONE', #105557, #76276, #120471, .T. ) ;
#38028 = EDGE_CURVE ( 'NONE', #69282, #116043, #90810, .T. ) ;
#38029 = CARTESIAN_POINT ( 'NONE',  ( 185.7343750003414016, 8.734944146203032389, 5.348610694689227483E-16 ) ) ;
#38030 = CARTESIAN_POINT ( 'NONE',  ( 10.79999999999991012, 12.50000000000000000, -4.330127018922201643 ) ) ;
#38031 = EDGE_CURVE ( 'NONE', #84244, #74651, #18052, .T. ) ;
#38032 = EDGE_CURVE ( 'NONE', #12562, #25677, #80994, .T. ) ;
#38033 = CARTESIAN_POINT ( 'NONE',  ( 7.499999999999961808, 12.50000000000000000, -4.395220292106239768 ) ) ;
#38034 = ORIENTED_EDGE ( 'NONE', *, *, #15974, .T. ) ;
#38035 = ORIENTED_EDGE ( 'NONE', *, *, #104116, .F. ) ;
#38036 = CARTESIAN_POINT ( 'NONE',  ( -14.19999999999998685, 12.50000000000000000, 0.06509327318403732021 ) ) ;
#38038 = ORIENTED_EDGE ( 'NONE', *, *, #79452, .T. ) ;
#38037 = EDGE_CURVE ( 'NONE', #13161, #75848, #118980, .T. ) ;
#38039 = DIRECTION ( 'NONE',  ( 0.000000000000000000, 0.000000000000000000, -1.000000000000000000 ) ) ;
#38040 = VECTOR ( 'NONE', #19399, 1000.000000000000000 ) ;
#38041 = AXIS2_PLACEMENT_3D ( 'NONE', #110667, #12464, #52398 ) ;
#38043 = VERTEX_POINT ( 'NONE', #29322 ) ;
#38042 = ORIENTED_EDGE ( 'NONE', *, *, #98032, .F. ) ;
#38044 = EDGE_LOOP ( 'NONE', ( #61915, #73781 ) ) ;
#38045 = ADVANCED_FACE ( 'NONE', ( #52178 ), #91451, .T. ) ;
#38046 = DIRECTION ( 'NONE',  ( 0.000000000000000000, 1.000000000000000000, 0.000000000000000000 ) ) ;
#38047 = EDGE_CURVE ( 'NONE', #36161, #32820, #80775, .T. ) ;
#38048 = DIRECTION ( 'NONE',  ( 0.000000000000000000, -0.9999939076577903929, 0.003490651415223739937 ) ) ;
#38049 = EDGE_CURVE ( 'NONE', #79899, #63390, #124682, .T. ) ;
#38051 = CARTESIAN_POINT ( 'NONE',  ( -11.69999999999999929, 2.500000000000000000, -4.330127018922198978 ) ) ;
#38050 = CIRCLE ( 'NONE', #59285, 0.06509327318403745899 ) ;
#38052 = AXIS2_PLACEMENT_3D ( 'NONE', #118851, #79581, #119488 ) ;
#38053 = FILL_AREA_STYLE ('',( #79277 ) ) ;
#38054 = DIRECTION ( 'NONE',  ( 0.000000000000000000, 0.000000000000000000, 1.000000000000000000 ) ) ;
#38055 = DIRECTION ( 'NONE',  ( -0.000000000000000000, -1.000000000000000000, -0.000000000000000000 ) ) ;
#38056 = DIRECTION ( 'NONE',  ( 0.000000000000000000, 0.000000000000000000, 1.000000000000000000 ) ) ;
#38057 = LINE ( 'NONE', #23896, #80277 ) ;
#38058 = CIRCLE ( 'NONE', #33841, 0.06509327318403745899 ) ;
#38059 = PRODUCT_RELATED_PRODUCT_CATEGORY ( 'part', '', ( #72268 ) ) ;
#38060 = EDGE_CURVE ( 'NONE', #77627, #78283, #78816, .T. ) ;
#38061 = DIRECTION ( 'NONE',  ( 0.000000000000000000, -0.000000000000000000, 1.000000000000000000 ) ) ;
#38063 = ORIENTED_EDGE ( 'NONE', *, *, #81010, .F. ) ;
#38062 = VECTOR ( 'NONE', #68422, 1000.000000000000000 ) ;
#38064 = VERTEX_POINT ( 'NONE', #111068 ) ;
#38065 = EDGE_LOOP ( 'NONE', ( #26331, #125753, #62093, #13226 ) ) ;
#38066 = ORIENTED_EDGE ( 'NONE', *, *, #112345, .T. ) ;
#38067 = CARTESIAN_POINT ( 'NONE',  ( -14.54999999999998472, 12.50000000000000000, 2.099970236277064028 ) ) ;
#38068 = ORIENTED_EDGE ( 'NONE', *, *, #50019, .T. ) ;
#38069 = ORIENTED_EDGE ( 'NONE', *, *, #125101, .F. ) ;
#38070 = CARTESIAN_POINT ( 'NONE',  ( 0.6499999999999561684, 12.50000000000000000, 1.818653347947321475 ) ) ;
#38071 = DIRECTION ( 'NONE',  ( 0.000000000000000000, -0.9999939076577903929, 0.003490651415223739937 ) ) ;
#38072 = DIRECTION ( 'NONE',  ( -0.000000000000000000, 1.000000000000000000, -0.000000000000000000 ) ) ;
#38073 = CARTESIAN_POINT ( 'NONE',  ( 8.349999999999923261, 12.50000000000000000, -5.802370205355749988 ) ) ;
#38074 = DIRECTION ( 'NONE',  ( 0.000000000000000000, 0.000000000000000000, 1.000000000000000000 ) ) ;
#38075 = EDGE_LOOP ( 'NONE', ( #78266, #21363 ) ) ;
#38076 = FACE_OUTER_BOUND ( 'NONE', #12054, .T. ) ;
#38077 = CIRCLE ( 'NONE', #44325, 0.1000000000000002554 ) ;
#38078 = CIRCLE ( 'NONE', #111117, 0.1000000000000002554 ) ;
#38079 = ORIENTED_EDGE ( 'NONE', *, *, #115587, .F. ) ;
#38080 = LINE ( 'NONE', #8590, #113616 ) ;
#38081 = ORIENTED_EDGE ( 'NONE', *, *, #14691, .F. ) ;
#38082 = DIRECTION ( 'NONE',  ( 0.000000000000000000, -0.9999939076577903929, 0.003490651415223739937 ) ) ;
#38083 = ORIENTED_EDGE ( 'NONE', *, *, #106164, .F. ) ;
#38084 = ORIENTED_EDGE ( 'NONE', *, *, #58628, .F. ) ;
#38085 = AXIS2_PLACEMENT_3D ( 'NONE', #112510, #73226, #113140 ) ;
#38086 = DIRECTION ( 'NONE',  ( 0.000000000000000000, -0.000000000000000000, 1.000000000000000000 ) ) ;
#38087 = DIRECTION ( 'NONE',  ( 0.000000000000000000, 0.000000000000000000, 1.000000000000000000 ) ) ;
#38088 = AXIS2_PLACEMENT_3D ( 'NONE', #91337, #92629, #101166 ) ;
#38089 = EDGE_CURVE ( 'NONE', #71724, #86890, #76741, .T. ) ;
#38090 = CIRCLE ( 'NONE', #104961, 0.1000000000000002554 ) ;
#38091 = CARTESIAN_POINT ( 'NONE',  ( 115.5000000000000000, 0.000000000000000000, 0.000000000000000000 ) ) ;
#38092 = VECTOR ( 'NONE', #58555, 1000.000000000000000 ) ;
#38093 = DIRECTION ( 'NONE',  ( 0.000000000000000000, 0.000000000000000000, 1.000000000000000000 ) ) ;
#38094 = ADVANCED_FACE ( 'NONE', ( #21421 ), #59445, .T. ) ;
#38095 = DIRECTION ( 'NONE',  ( -4.274815082592931898E-19, -0.9999939076577903929, -0.003490651415223739937 ) ) ;
#38096 = EDGE_LOOP ( 'NONE', ( #116159, #101109, #60740, #122606 ) ) ;
#38097 = DIRECTION ( 'NONE',  ( 0.000000000000000000, 1.000000000000000000, 0.000000000000000000 ) ) ;
#38098 = DIRECTION ( 'NONE',  ( -0.000000000000000000, 1.000000000000000000, -0.000000000000000000 ) ) ;
#38099 = DIRECTION ( 'NONE',  ( -0.000000000000000000, 1.000000000000000000, -0.000000000000000000 ) ) ;
#38100 = DIRECTION ( 'NONE',  ( 0.000000000000000000, 1.000000000000000000, 0.000000000000000000 ) ) ;
#38101 = CONICAL_SURFACE ( 'NONE', #117476, 0.09999999999999982514, 0.003490658503988666988 ) ;
#38102 = ADVANCED_FACE ( 'NONE', ( #39799 ), #89260, .T. ) ;
#38103 = CIRCLE ( 'NONE', #90305, 0.06509327318403745899 ) ;
#38104 = FACE_OUTER_BOUND ( 'NONE', #35623, .T. ) ;
#38105 = EDGE_LOOP ( 'NONE', ( #5493, #122382 ) ) ;
#38106 = AXIS2_PLACEMENT_3D ( 'NONE', #74215, #62478, #52631 ) ;
#38107 = AXIS2_PLACEMENT_3D ( 'NONE', #74739, #114023, #76674 ) ;
#38108 = VERTEX_POINT ( 'NONE', #60082 ) ;
#38109 = DIRECTION ( 'NONE',  ( 0.000000000000000000, 0.000000000000000000, 1.000000000000000000 ) ) ;
#38110 = VECTOR ( 'NONE', #28827, 1000.000000000000000 ) ;
#38111 = VERTEX_POINT ( 'NONE', #50251 ) ;
#38112 = CARTESIAN_POINT ( 'NONE',  ( -3.350000000000032507, 2.500000000000000000, -6.595190528383302109 ) ) ;
#38113 = DIRECTION ( 'NONE',  ( 0.000000000000000000, 1.000000000000000000, 0.000000000000000000 ) ) ;
#38114 = VECTOR ( 'NONE', #21590, 1000.000000000000000 ) ;
#38115 = EDGE_LOOP ( 'NONE', ( #66383, #44480, #99478, #104848 ) ) ;
#38116 = CARTESIAN_POINT ( 'NONE',  ( 185.9166666666666856, 6.668395609140176816, 3.850000000000000977 ) ) ;
#38117 = DIRECTION ( 'NONE',  ( 0.000000000000000000, 0.000000000000000000, 1.000000000000000000 ) ) ;
#38118 = CARTESIAN_POINT ( 'NONE',  ( 1.849999999999949019, 12.50000000000000000, 6.841600689897072485 ) ) ;
#38119 = DIRECTION ( 'NONE',  ( -0.000000000000000000, 1.000000000000000000, -0.000000000000000000 ) ) ;
#38120 = ORIENTED_EDGE ( 'NONE', *, *, #102449, .T. ) ;
#38121 = CARTESIAN_POINT ( 'NONE',  ( -1.250000000000037526, 2.500000000000000000, -5.702370205355749455 ) ) ;
#38122 = DIRECTION ( 'NONE',  ( 0.000000000000000000, -0.000000000000000000, 1.000000000000000000 ) ) ;
#38123 = ORIENTED_EDGE ( 'NONE', *, *, #9953, .F. ) ;
#38124 = CARTESIAN_POINT ( 'NONE',  ( 1.649999999999951505, 12.50000000000000000, 1.472243186433545459 ) ) ;
#38125 = FACE_OUTER_BOUND ( 'NONE', #93564, .T. ) ;
#38126 = DIRECTION ( 'NONE',  ( -0.000000000000000000, -1.000000000000000000, -0.000000000000000000 ) ) ;
#38127 = ORIENTED_EDGE ( 'NONE', *, *, #123340, .T. ) ;
#38128 = CARTESIAN_POINT ( 'NONE',  ( 1.849999999999948130, 2.500000000000000000, 6.048780366869520364 ) ) ;
#38129 = CIRCLE ( 'NONE', #81933, 0.1000000000000000472 ) ;
#38130 = CIRCLE ( 'NONE', #75673, 0.06509327318403745899 ) ;
#38131 = ORIENTED_EDGE ( 'NONE', *, *, #42682, .T. ) ;
#38132 = CARTESIAN_POINT ( 'NONE',  ( -12.49999999999995914, 2.500000000000000000, -4.330127018922198978 ) ) ;
#38133 = CARTESIAN_POINT ( 'NONE',  ( -4.600000000000024514, 2.500000000000000000, 0.6928203230275494784 ) ) ;
#38134 = DIRECTION ( 'NONE',  ( 0.000000000000000000, 1.000000000000000000, 0.000000000000000000 ) ) ;
#38135 = VERTEX_POINT ( 'NONE', #55401 ) ;
#38137 = LINE ( 'NONE', #117976, #65647 ) ;
#38136 = AXIS2_PLACEMENT_3D ( 'NONE', #104077, #114522, #65428 ) ;
#38138 = AXIS2_PLACEMENT_3D ( 'NONE', #28772, #88971, #109907 ) ;
#38139 = VECTOR ( 'NONE', #23555, 1000.000000000000000 ) ;
#38140 = DIRECTION ( 'NONE',  ( 0.000000000000000000, 0.000000000000000000, 1.000000000000000000 ) ) ;
#38142 = EDGE_CURVE ( 'NONE', #42165, #32002, #113022, .T. ) ;
#38141 = AXIS2_PLACEMENT_3D ( 'NONE', #100979, #102280, #110794 ) ;
#38143 = EDGE_LOOP ( 'NONE', ( #119419, #101501 ) ) ;
#38144 = LINE ( 'NONE', #19795, #76121 ) ;
#38145 = EDGE_CURVE ( 'NONE', #48067, #13926, #41170, .T. ) ;
#38146 = VERTEX_POINT ( 'NONE', #105131 ) ;
#38147 = CONICAL_SURFACE ( 'NONE', #105032, 0.09999999999999982514, 0.003490658503988666988 ) ;
#38148 = DIRECTION ( 'NONE',  ( 0.000000000000000000, 0.000000000000000000, 1.000000000000000000 ) ) ;
#38149 = ORIENTED_EDGE ( 'NONE', *, *, #126053, .T. ) ;
#38150 = DIRECTION ( 'NONE',  ( -0.000000000000000000, -1.000000000000000000, -0.000000000000000000 ) ) ;
#38151 = CARTESIAN_POINT ( 'NONE',  ( 10.39999999999991509, 12.50000000000000000, 0.6928203230275494784 ) ) ;
#38152 = ORIENTED_EDGE ( 'NONE', *, *, #53575, .T. ) ;
#38153 = EDGE_CURVE ( 'NONE', #5078, #106111, #94031, .T. ) ;
#38154 = VERTEX_POINT ( 'NONE', #75041 ) ;
#38155 = DIRECTION ( 'NONE',  ( -0.000000000000000000, 1.000000000000000000, -0.000000000000000000 ) ) ;
#38156 = DIRECTION ( 'NONE',  ( 0.000000000000000000, 0.000000000000000000, -1.000000000000000000 ) ) ;
#38157 = ORIENTED_EDGE ( 'NONE', *, *, #76349, .F. ) ;
#38158 = VECTOR ( 'NONE', #18144, 1000.000000000000000 ) ;
#38159 = CARTESIAN_POINT ( 'NONE',  ( -4.800000000000022915, 2.500000000000000000, -0.3464101615137783474 ) ) ;
#38160 = CARTESIAN_POINT ( 'NONE',  ( 187.2343750003414016, 8.734944146203032389, 5.348610694689227483E-16 ) ) ;
#38161 = DIRECTION ( 'NONE',  ( -0.000000000000000000, 1.000000000000000000, -0.000000000000000000 ) ) ;
#38162 = CARTESIAN_POINT ( 'NONE',  ( -11.44999999999999929, 12.50000000000000000, -1.818653347947322141 ) ) ;
#38163 = DIRECTION ( 'NONE',  ( 0.000000000000000000, 0.000000000000000000, -1.000000000000000000 ) ) ;
#38164 = DIRECTION ( 'NONE',  ( -4.274815082592931898E-19, -0.9999939076577903929, -0.003490651415223739937 ) ) ;
#38165 = CONICAL_SURFACE ( 'NONE', #123831, 0.1000000000000002554, 0.003490658503988666988 ) ;
#38166 = VECTOR ( 'NONE', #102869, 1000.000000000000000 ) ;
#38167 = ORIENTED_EDGE ( 'NONE', *, *, #120409, .F. ) ;
#38169 = ORIENTED_EDGE ( 'NONE', *, *, #85786, .T. ) ;
#38168 = ADVANCED_FACE ( 'NONE', ( #54735 ), #112392, .T. ) ;
#38170 = VERTEX_POINT ( 'NONE', #4331 ) ;
#38171 = ORIENTED_EDGE ( 'NONE', *, *, #118802, .T. ) ;
#38172 = CARTESIAN_POINT ( 'NONE',  ( -10.85000000000000142, 12.50000000000000000, 2.230156782645134950 ) ) ;
#38173 = DIRECTION ( 'NONE',  ( -0.000000000000000000, -1.000000000000000000, -0.000000000000000000 ) ) ;
#38174 = CARTESIAN_POINT ( 'NONE',  ( -6.650000000000018119, 12.50000000000000000, -2.857883832488653741 ) ) ;
#38175 = ORIENTED_EDGE ( 'NONE', *, *, #117149, .F. ) ;
#38176 = FACE_BOUND ( 'NONE', #3392, .T. ) ;
#38177 = ORIENTED_EDGE ( 'NONE', *, *, #58939, .T. ) ;
#38178 = CARTESIAN_POINT ( 'NONE',  ( -13.94999999999998863, 2.500000000000000000, -1.818653347947323917 ) ) ;
#38179 = DIRECTION ( 'NONE',  ( 0.000000000000000000, 1.000000000000000000, 0.000000000000000000 ) ) ;
#38180 = CIRCLE ( 'NONE', #21446, 0.1000000000000002554 ) ;
#38183 = ADVANCED_FACE ( 'NONE', ( #122851 ), #74593, .T. ) ;
#38182 = DIRECTION ( 'NONE',  ( 0.000000000000000000, 0.000000000000000000, 1.000000000000000000 ) ) ;
#38181 = VECTOR ( 'NONE', #39502, 1000.000000000000000 ) ;
#38184 = AXIS2_PLACEMENT_3D ( 'NONE', #8779, #99766, #48736 ) ;
#38185 = CARTESIAN_POINT ( 'NONE',  ( 11.24999999999990585, 2.500000000000000000, -5.902370205355750521 ) ) ;
#38186 = DIRECTION ( 'NONE',  ( 0.000000000000000000, -0.000000000000000000, 1.000000000000000000 ) ) ;
#38187 = FACE_OUTER_BOUND ( 'NONE', #56116, .T. ) ;
#38188 = LINE ( 'NONE', #8696, #8101 ) ;
#38189 = DIRECTION ( 'NONE',  ( 0.000000000000000000, 0.000000000000000000, 1.000000000000000000 ) ) ;
#38190 = EDGE_CURVE ( 'NONE', #93275, #108043, #53476, .T. ) ;
#38191 = ADVANCED_FACE ( 'NONE', ( #3711 ), #44279, .T. ) ;
#38192 = DIRECTION ( 'NONE',  ( 0.000000000000000000, 1.000000000000000000, 0.000000000000000000 ) ) ;
#38193 = EDGE_CURVE ( 'NONE', #127376, #49108, #68324, .T. ) ;
#38194 = EDGE_CURVE ( 'NONE', #22334, #43141, #101792, .T. ) ;
#38195 = AXIS2_PLACEMENT_3D ( 'NONE', #19624, #18958, #108639 ) ;
#38196 = DIRECTION ( 'NONE',  ( 0.000000000000000000, 1.000000000000000000, 0.000000000000000000 ) ) ;
#38197 = ORIENTED_EDGE ( 'NONE', *, *, #26388, .T. ) ;
#38198 = EDGE_LOOP ( 'NONE', ( #34257, #25157, #66421, #6880 ) ) ;
#38199 = ORIENTED_EDGE ( 'NONE', *, *, #9831, .F. ) ;
#38201 = EDGE_LOOP ( 'NONE', ( #3553, #22887, #48005, #34159 ) ) ;
#38200 = VECTOR ( 'NONE', #21638, 1000.000000000000000 ) ;
#38202 = CIRCLE ( 'NONE', #33990, 0.09999999999999982514 ) ;
#38203 = AXIS2_PLACEMENT_3D ( 'NONE', #25455, #66678, #106606 ) ;
#38204 = DIRECTION ( 'NONE',  ( -0.000000000000000000, -1.000000000000000000, -0.000000000000000000 ) ) ;
#38205 = EDGE_CURVE ( 'NONE', #98683, #114600, #26568, .T. ) ;
#38206 = DIRECTION ( 'NONE',  ( -0.000000000000000000, 1.000000000000000000, -0.000000000000000000 ) ) ;
#38209 = VERTEX_POINT ( 'NONE', #12867 ) ;
#38208 = ORIENTED_EDGE ( 'NONE', *, *, #49112, .T. ) ;
#38207 = EDGE_CURVE ( 'NONE', #11460, #79421, #18143, .T. ) ;
#38210 = ORIENTED_EDGE ( 'NONE', *, *, #30810, .T. ) ;
#38211 = DIRECTION ( 'NONE',  ( 0.000000000000000000, -0.9999939076577903929, 0.003490651415223739937 ) ) ;
#38212 = EDGE_CURVE ( 'NONE', #113, #11709, #45361, .T. ) ;
#38213 = EDGE_CURVE ( 'NONE', #4130, #46755, #91317, .T. ) ;
#38214 = DIRECTION ( 'NONE',  ( 0.000000000000000000, 0.000000000000000000, 1.000000000000000000 ) ) ;
#38215 = AXIS2_PLACEMENT_3D ( 'NONE', #73264, #5792, #115762 ) ;
#38216 = DIRECTION ( 'NONE',  ( -4.274815082592931898E-19, -0.9999939076577903929, -0.003490651415223739937 ) ) ;
#38217 = DIRECTION ( 'NONE',  ( 0.000000000000000000, 1.000000000000000000, 0.000000000000000000 ) ) ;
#38218 = LINE ( 'NONE', #78142, #72252 ) ;
#38219 = DIRECTION ( 'NONE',  ( 0.000000000000000000, 0.000000000000000000, -1.000000000000000000 ) ) ;
#38220 = DIRECTION ( 'NONE',  ( -0.000000000000000000, 1.000000000000000000, -0.000000000000000000 ) ) ;
#38221 = VERTEX_POINT ( 'NONE', #54108 ) ;
#38222 = EDGE_CURVE ( 'NONE', #95448, #117445, #124786, .T. ) ;
#38223 = DIRECTION ( 'NONE',  ( 0.000000000000000000, 1.000000000000000000, 0.000000000000000000 ) ) ;
#38224 = ORIENTED_EDGE ( 'NONE', *, *, #14902, .T. ) ;
#38225 = ORIENTED_EDGE ( 'NONE', *, *, #102731, .F. ) ;
#38226 = EDGE_LOOP ( 'NONE', ( #111946, #31572 ) ) ;
#38227 = DIRECTION ( 'NONE',  ( 0.000000000000000000, 1.000000000000000000, 0.000000000000000000 ) ) ;
#38228 = CIRCLE ( 'NONE', #25687, 0.06509327318403743123 ) ;
#38229 = CIRCLE ( 'NONE', #109311, 0.1000000000000002554 ) ;
#38230 = ORIENTED_EDGE ( 'NONE', *, *, #84002, .F. ) ;
#38231 = ORIENTED_EDGE ( 'NONE', *, *, #100743, .T. ) ;
#38232 = DIRECTION ( 'NONE',  ( -0.000000000000000000, 1.000000000000000000, -0.000000000000000000 ) ) ;
#38233 = DIRECTION ( 'NONE',  ( 0.000000000000000000, 0.000000000000000000, 1.000000000000000000 ) ) ;
#38234 = DIRECTION ( 'NONE',  ( 0.000000000000000000, 1.000000000000000000, 0.000000000000000000 ) ) ;
#38236 = FACE_OUTER_BOUND ( 'NONE', #2243, .T. ) ;
#38235 = CIRCLE ( 'NONE', #6791, 2.000000000000000000 ) ;
#38237 = AXIS2_PLACEMENT_3D ( 'NONE', #126907, #17575, #26768 ) ;
#38238 = AXIS2_PLACEMENT_3D ( 'NONE', #105367, #55620, #54332 ) ;
#38239 = LINE ( 'NONE', #7461, #97809 ) ;
#38240 = EDGE_LOOP ( 'NONE', ( #116775, #1517, #15400, #83695 ) ) ;
#38241 = CARTESIAN_POINT ( 'NONE',  ( 1.849999999999950573, 2.500000000000000000, 2.511473670974873507 ) ) ;
#38242 = CIRCLE ( 'NONE', #25703, 0.1000000000000002554 ) ;
#38244 = ORIENTED_EDGE ( 'NONE', *, *, #57985, .F. ) ;
#38243 = AXIS2_PLACEMENT_3D ( 'NONE', #49548, #78364, #88808 ) ;
#38245 = DIRECTION ( 'NONE',  ( 0.000000000000000000, 1.000000000000000000, 0.000000000000000000 ) ) ;
#38246 = VECTOR ( 'NONE', #50650, 1000.000000000000000 ) ;
#38247 = VERTEX_POINT ( 'NONE', #14163 ) ;
#38248 = CARTESIAN_POINT ( 'NONE',  ( 12.04999999999990834, 12.50000000000000000, 6.560283801567334372 ) ) ;
#38249 = DIRECTION ( 'NONE',  ( -0.000000000000000000, 1.000000000000000000, -0.000000000000000000 ) ) ;
#38250 = ORIENTED_EDGE ( 'NONE', *, *, #84587, .F. ) ;
#38251 = DIRECTION ( 'NONE',  ( 0.000000000000000000, 0.000000000000000000, 1.000000000000000000 ) ) ;
#38252 = DIRECTION ( 'NONE',  ( 0.000000000000000000, 1.000000000000000000, 0.000000000000000000 ) ) ;
#38253 = VERTEX_POINT ( 'NONE', #114945 ) ;
#38254 = AXIS2_PLACEMENT_3D ( 'NONE', #73021, #110363, #112947 ) ;
#38255 = EDGE_CURVE ( 'NONE', #1392, #33034, #24653, .T. ) ;
#38256 = DIRECTION ( 'NONE',  ( -0.000000000000000000, 1.000000000000000000, -0.000000000000000000 ) ) ;
#38257 = EDGE_CURVE ( 'NONE', #15629, #92907, #36946, .T. ) ;
#38258 = ORIENTED_EDGE ( 'NONE', *, *, #6392, .T. ) ;
#38259 = ORIENTED_EDGE ( 'NONE', *, *, #96363, .F. ) ;
#38260 = DIRECTION ( 'NONE',  ( 0.000000000000000000, 1.000000000000000000, 0.000000000000000000 ) ) ;
#38261 = FACE_OUTER_BOUND ( 'NONE', #73697, .T. ) ;
#38262 = CARTESIAN_POINT ( 'NONE',  ( 184.0677083336747160, -4.367472073101514418, -7.564683531250002702 ) ) ;
#38263 = DIRECTION ( 'NONE',  ( 0.000000000000000000, 1.000000000000000000, 0.000000000000000000 ) ) ;
#38264 = VECTOR ( 'NONE', #100429, 1000.000000000000000 ) ;
#38265 = FACE_OUTER_BOUND ( 'NONE', #63479, .T. ) ;
#38266 = CARTESIAN_POINT ( 'NONE',  ( -3.100000000000028511, 2.500000000000000000, -4.776537180435977525 ) ) ;
#38267 = ORIENTED_EDGE ( 'NONE', *, *, #112503, .F. ) ;
#38268 = AXIS2_PLACEMENT_3D ( 'NONE', #31097, #100457, #71005 ) ;
#38269 = CARTESIAN_POINT ( 'NONE',  ( 87.50000000000001421, 3.975344334345554120, -6.360552532166837914 ) ) ;
#38270 = DIRECTION ( 'NONE',  ( 0.000000000000000000, -0.000000000000000000, 1.000000000000000000 ) ) ;
#38271 = AXIS2_PLACEMENT_3D ( 'NONE', #24330, #34816, #105468 ) ;
#38272 = ORIENTED_EDGE ( 'NONE', *, *, #83556, .F. ) ;
#38273 = DIRECTION ( 'NONE',  ( 0.000000000000000000, -0.000000000000000000, 1.000000000000000000 ) ) ;
#38274 = DIRECTION ( 'NONE',  ( 0.000000000000000000, -0.000000000000000000, 1.000000000000000000 ) ) ;
#38275 = DIRECTION ( 'NONE',  ( 0.000000000000000000, 0.000000000000000000, -1.000000000000000000 ) ) ;
#38276 = CARTESIAN_POINT ( 'NONE',  ( -0.2000000000000399791, 12.50000000000000000, -4.676537180435977881 ) ) ;
#38277 = AXIS2_PLACEMENT_3D ( 'NONE', #68075, #8498, #58912 ) ;
#38279 = AXIS2_PLACEMENT_3D ( 'NONE', #105523, #23745, #14540 ) ;
#38278 = CARTESIAN_POINT ( 'NONE',  ( 186.7500000000000000, 9.429780353434619030E-16, -7.700000000000000178 ) ) ;
#38280 = ORIENTED_EDGE ( 'NONE', *, *, #110617, .F. ) ;
#38281 = CIRCLE ( 'NONE', #21546, 0.06509327318403745899 ) ;
#38282 = AXIS2_PLACEMENT_3D ( 'NONE', #64971, #126493, #104895 ) ;
#38283 = DIRECTION ( 'NONE',  ( 0.000000000000000000, -0.9999939076577903929, 0.003490651415223739937 ) ) ;
#38284 = FACE_OUTER_BOUND ( 'NONE', #124356, .T. ) ;
#38285 = AXIS2_PLACEMENT_3D ( 'NONE', #69195, #88176, #98654 ) ;
#38286 = ORIENTED_EDGE ( 'NONE', *, *, #11586, .T. ) ;
#38287 = DIRECTION ( 'NONE',  ( 0.000000000000000000, 0.000000000000000000, -1.000000000000000000 ) ) ;
#38288 = EDGE_CURVE ( 'NONE', #34969, #2954, #51619, .T. ) ;
#38289 = EDGE_LOOP ( 'NONE', ( #105775, #44267 ) ) ;
#38290 = AXIS2_PLACEMENT_3D ( 'NONE', #9503, #89353, #129301 ) ;
#38292 = ORIENTED_EDGE ( 'NONE', *, *, #29884, .T. ) ;
#38291 = VECTOR ( 'NONE', #52718, 1000.000000000000000 ) ;
#38293 = AXIS2_PLACEMENT_3D ( 'NONE', #9049, #49649, #88235 ) ;
#38294 = CARTESIAN_POINT ( 'NONE',  ( 2.949999999999943334, 12.50000000000000000, 6.495190528383297135 ) ) ;
#38295 = EDGE_LOOP ( 'NONE', ( #10656, #28480, #80614, #77569 ) ) ;
#38296 = CARTESIAN_POINT ( 'NONE',  ( -7.300000000000018474, 12.50000000000000000, -3.983716857408426293 ) ) ;
#38297 = DIRECTION ( 'NONE',  ( 0.000000000000000000, 0.000000000000000000, -1.000000000000000000 ) ) ;
#38298 = DIRECTION ( 'NONE',  ( 0.000000000000000000, 1.000000000000000000, 0.000000000000000000 ) ) ;
#38299 = EDGE_LOOP ( 'NONE', ( #54906, #57785, #54470, #56318 ) ) ;
#38300 = LINE ( 'NONE', #48767, #128276 ) ;
#38301 = AXIS2_PLACEMENT_3D ( 'NONE', #74404, #94679, #97261 ) ;
#38303 = ORIENTED_EDGE ( 'NONE', *, *, #86182, .T. ) ;
#38302 = CARTESIAN_POINT ( 'NONE',  ( 4.999999999999935163, 12.50000000000000000, 0.6928203230275494784 ) ) ;
#38304 = EDGE_CURVE ( 'NONE', #39786, #25992, #25945, .T. ) ;
#38305 = DIRECTION ( 'NONE',  ( 0.000000000000000000, 0.000000000000000000, -1.000000000000000000 ) ) ;
#38306 = DIRECTION ( 'NONE',  ( 0.000000000000000000, -0.9999939076577903929, 0.003490651415223739937 ) ) ;
#38307 = EDGE_CURVE ( 'NONE', #54643, #46118, #118491, .T. ) ;
#38308 = ORIENTED_EDGE ( 'NONE', *, *, #64542, .T. ) ;
#38309 = ORIENTED_EDGE ( 'NONE', *, *, #93523, .T. ) ;
#38310 = EDGE_LOOP ( 'NONE', ( #111007, #40384 ) ) ;
#38311 = DIRECTION ( 'NONE',  ( 0.000000000000000000, -0.000000000000000000, 1.000000000000000000 ) ) ;
#38312 = FACE_OUTER_BOUND ( 'NONE', #117493, .T. ) ;
#38314 = DIRECTION ( 'NONE',  ( 0.000000000000000000, 1.000000000000000000, 0.000000000000000000 ) ) ;
#38313 = AXIS2_PLACEMENT_3D ( 'NONE', #7131, #87630, #56870 ) ;
#38315 = AXIS2_PLACEMENT_3D ( 'NONE', #56681, #96608, #46896 ) ;
#38316 = EDGE_CURVE ( 'NONE', #32403, #80982, #95963, .T. ) ;
#38317 = FACE_BOUND ( 'NONE', #107564, .T. ) ;
#38318 = ORIENTED_EDGE ( 'NONE', *, *, #43732, .T. ) ;
#38319 = FACE_OUTER_BOUND ( 'NONE', #118677, .T. ) ;
#38320 = CARTESIAN_POINT ( 'NONE',  ( 1.449999999999952216, 2.500000000000000000, -2.411473670974877859 ) ) ;
#38321 = EDGE_LOOP ( 'NONE', ( #25648, #13398 ) ) ;
#38322 = CARTESIAN_POINT ( 'NONE',  ( 184.5000000000000000, 0.000000000000000000, 0.000000000000000000 ) ) ;
#38324 = CARTESIAN_POINT ( 'NONE',  ( 6.449999999999931788, 12.50000000000000000, -6.148780366869526226 ) ) ;
#38323 = AXIS2_PLACEMENT_3D ( 'NONE', #38294, #117446, #78221 ) ;
#38325 = AXIS2_PLACEMENT_3D ( 'NONE', #48462, #59604, #28184 ) ;
#38326 = AXIS2_PLACEMENT_3D ( 'NONE', #7108, #16274, #94862 ) ;
#38328 = CIRCLE ( 'NONE', #55032, 0.09999999999999982514 ) ;
#38327 = DIRECTION ( 'NONE',  ( 0.000000000000000000, 1.000000000000000000, 0.000000000000000000 ) ) ;
#38329 = DIRECTION ( 'NONE',  ( 0.000000000000000000, -0.000000000000000000, 1.000000000000000000 ) ) ;
#38330 = CARTESIAN_POINT ( 'NONE',  ( 5.449999999999936229, 12.50000000000000000, -2.099970236277064473 ) ) ;
#38331 = DIRECTION ( 'NONE',  ( 0.000000000000000000, 0.000000000000000000, -1.000000000000000000 ) ) ;
#38332 = CARTESIAN_POINT ( 'NONE',  ( -5.800000000000018474, 12.50000000000000000, 4.395220292106234439 ) ) ;
#38333 = AXIS2_PLACEMENT_3D ( 'NONE', #31505, #51799, #71408 ) ;
#38334 = AXIS2_PLACEMENT_3D ( 'NONE', #61940, #101856, #12165 ) ;
#38335 = AXIS2_PLACEMENT_3D ( 'NONE', #21187, #61113, #101042 ) ;
#38336 = ORIENTED_EDGE ( 'NONE', *, *, #77191, .F. ) ;
#38337 = VERTEX_POINT ( 'NONE', #125428 ) ;
#38338 = VERTEX_POINT ( 'NONE', #7569 ) ;
#38339 = ORIENTED_EDGE ( 'NONE', *, *, #21012, .F. ) ;
#38341 = ORIENTED_EDGE ( 'NONE', *, *, #22400, .F. ) ;
#38340 = CIRCLE ( 'NONE', #55047, 0.1000000000000002554 ) ;
#38342 = DIRECTION ( 'NONE',  ( 0.000000000000000000, 0.000000000000000000, 1.000000000000000000 ) ) ;
#38343 = PLANE ( 'NONE',  #15370 ) ;
#38344 = ORIENTED_EDGE ( 'NONE', *, *, #48389, .F. ) ;
#38345 = FACE_BOUND ( 'NONE', #4748, .T. ) ;
#38346 = CARTESIAN_POINT ( 'NONE',  ( -13.74999999999998934, 2.500000000000000000, -1.572243186433547990 ) ) ;
#38347 = ADVANCED_FACE ( 'NONE', ( #108358 ), #87097, .T. ) ;
#38348 = DIRECTION ( 'NONE',  ( -0.000000000000000000, -1.000000000000000000, -0.000000000000000000 ) ) ;
#38349 = CARTESIAN_POINT ( 'NONE',  ( -2.900000000000029221, 12.50000000000000000, -5.022947341949754119 ) ) ;
#38350 =( BOUNDED_CURVE ( )  B_SPLINE_CURVE ( 2, ( #16925, #76539, #26786, #77805, #66700, #96801, #126931 ),
 .UNSPECIFIED., .F., .F. ) 
 B_SPLINE_CURVE_WITH_KNOTS ( ( 3, 2, 2, 3 ),
 ( 0.07142857142857149400, 0.09523809523809532995, 0.1190476190476191520, 0.1428571428571429880 ),
 .UNSPECIFIED. ) 
 CURVE ( )  GEOMETRIC_REPRESENTATION_ITEM ( )  RATIONAL_B_SPLINE_CURVE ( ( 0.9999999999999996669, 0.8660254037844390407, 1.000000000000000000, 0.8660254037844387076, 1.000000000000000000, 0.8660254037844379305, 1.000000000000000666 ) ) 
 REPRESENTATION_ITEM ( '' )  );
#38351 = LINE ( 'NONE', #59290, #101419 ) ;
#38352 = EDGE_CURVE ( 'NONE', #34182, #52632, #35760, .T. ) ;
#38353 = CARTESIAN_POINT ( 'NONE',  ( -13.34999999999999076, 12.50000000000000000, 1.472243186433549456 ) ) ;
#38354 = VERTEX_POINT ( 'NONE', #6272 ) ;
#38355 = LINE ( 'NONE', #40785, #72384 ) ;
#38356 = ADVANCED_FACE ( 'NONE', ( #116240 ), #95527, .T. ) ;
#38357 = VECTOR ( 'NONE', #112185, 1000.000000000000000 ) ;
#38358 = ORIENTED_EDGE ( 'NONE', *, *, #66721, .T. ) ;
#38359 = ORIENTED_EDGE ( 'NONE', *, *, #46976, .T. ) ;
#38360 = ORIENTED_EDGE ( 'NONE', *, *, #85868, .F. ) ;
#38361 = EDGE_CURVE ( 'NONE', #99244, #68489, #112255, .T. ) ;
#38362 = CARTESIAN_POINT ( 'NONE',  ( 12.94999999999990337, 12.50000000000000000, 2.165063509461097713 ) ) ;
#38364 = ADVANCED_FACE ( 'NONE', ( #46217 ), #6909, .T. ) ;
#38363 = DIRECTION ( 'NONE',  ( 0.000000000000000000, 1.000000000000000000, 0.000000000000000000 ) ) ;
#38365 = DIRECTION ( 'NONE',  ( 0.000000000000000000, 0.000000000000000000, -1.000000000000000000 ) ) ;
#38367 = ORIENTED_EDGE ( 'NONE', *, *, #2523, .T. ) ;
#38366 = EDGE_CURVE ( 'NONE', #22212, #101321, #55810, .T. ) ;
#38368 = DIRECTION ( 'NONE',  ( 0.000000000000000000, -0.9999939076577903929, 0.003490651415223739937 ) ) ;
#38369 = EDGE_CURVE ( 'NONE', #51769, #57444, #3581, .T. ) ;
#38370 = CIRCLE ( 'NONE', #69647, 0.06509327318403745899 ) ;
#38371 = VECTOR ( 'NONE', #47993, 1000.000000000000000 ) ;
#38373 = DIRECTION ( 'NONE',  ( 0.000000000000000000, 0.000000000000000000, 1.000000000000000000 ) ) ;
#38372 = VECTOR ( 'NONE', #82252, 1000.000000000000000 ) ;
#38375 = ADVANCED_FACE ( 'NONE', ( #116874 ), #5635, .T. ) ;
#38374 = DIRECTION ( 'NONE',  ( 0.000000000000000000, 1.000000000000000000, 0.000000000000000000 ) ) ;
#38376 = CARTESIAN_POINT ( 'NONE',  ( 185.1093750003413732, 9.264065473108010111E-16, -7.564683531250000925 ) ) ;
#38377 = CARTESIAN_POINT ( 'NONE',  ( 12.69999999999989804, 2.500000000000000000, 0.2464101615137735679 ) ) ;
#38378 = CARTESIAN_POINT ( 'NONE',  ( 0.000000000000000000, 2.500000000000000000, 0.000000000000000000 ) ) ;
#38379 = PLANE ( 'NONE',  #85083 ) ;
#38380 = CIRCLE ( 'NONE', #88517, 0.06509327318403745899 ) ;
#38381 = ORIENTED_EDGE ( 'NONE', *, *, #42794, .T. ) ;
#38382 = CARTESIAN_POINT ( 'NONE',  ( -9.550000000000007816, 12.50000000000000000, -6.430097255199259010 ) ) ;
#38383 = CIRCLE ( 'NONE', #63405, 0.06509327318403745899 ) ;
#38384 = ADVANCED_FACE ( 'NONE', ( #86118 ), #116436, .T. ) ;
#38385 = CIRCLE ( 'NONE', #82287, 0.1000000000000002554 ) ;
#38386 = VERTEX_POINT ( 'NONE', #118182 ) ;
#38387 = CIRCLE ( 'NONE', #53042, 0.06509327318403745899 ) ;
#38388 = ORIENTED_EDGE ( 'NONE', *, *, #41476, .T. ) ;
#38389 = CARTESIAN_POINT ( 'NONE',  ( 4.149999999999938183, 2.500000000000000000, 5.902370205355745192 ) ) ;
#38390 = CARTESIAN_POINT ( 'NONE',  ( 8.349999999999919709, 12.50000000000000000, 5.737276932171707422 ) ) ;
#38391 = DIRECTION ( 'NONE',  ( -0.000000000000000000, 1.000000000000000000, -0.000000000000000000 ) ) ;
#38392 = AXIS2_PLACEMENT_3D ( 'NONE', #43044, #39958, #13540 ) ;
#38393 = ORIENTED_EDGE ( 'NONE', *, *, #54408, .F. ) ;
#38394 = ORIENTED_EDGE ( 'NONE', *, *, #127581, .F. ) ;
#38395 = DIRECTION ( 'NONE',  ( -0.000000000000000000, 1.000000000000000000, -0.000000000000000000 ) ) ;
#38397 = VECTOR ( 'NONE', #109619, 1000.000000000000000 ) ;
#38396 = DIRECTION ( 'NONE',  ( 0.000000000000000000, 0.000000000000000000, -1.000000000000000000 ) ) ;
#38398 = CONICAL_SURFACE ( 'NONE', #111531, 0.09999999999999982514, 0.003490658503988666988 ) ;
#38399 = AXIS2_PLACEMENT_3D ( 'NONE', #74433, #35791, #3746 ) ;
#38400 = CARTESIAN_POINT ( 'NONE',  ( -7.300000000000013145, 2.500000000000000000, 3.983716857408420076 ) ) ;
#38401 = ORIENTED_EDGE ( 'NONE', *, *, #104007, .T. ) ;
#38402 = ORIENTED_EDGE ( 'NONE', *, *, #99348, .F. ) ;
#38403 = CARTESIAN_POINT ( 'NONE',  ( 1.849999999999949685, 12.50000000000000000, -2.576566944158915184 ) ) ;
#38404 = CIRCLE ( 'NONE', #34193, 0.06509327318403745899 ) ;
#38405 = ORIENTED_EDGE ( 'NONE', *, *, #45021, .F. ) ;
#38406 = AXIS2_PLACEMENT_3D ( 'NONE', #112077, #61033, #111407 ) ;
#38407 = CARTESIAN_POINT ( 'NONE',  ( 6.649999999999928413, 2.500000000000000000, 2.957883832488649389 ) ) ;
#38408 = DIRECTION ( 'NONE',  ( 0.000000000000000000, -0.000000000000000000, 1.000000000000000000 ) ) ;
#38409 = VERTEX_POINT ( 'NONE', #45588 ) ;
#38410 = DIRECTION ( 'NONE',  ( 0.000000000000000000, 0.000000000000000000, 1.000000000000000000 ) ) ;
#38411 = CARTESIAN_POINT ( 'NONE',  ( -11.89999999999999680, 2.500000000000000000, -0.3464101615137741841 ) ) ;
#38412 = PLANE ( 'NONE',  #7174 ) ;
#38413 = CARTESIAN_POINT ( 'NONE',  ( -1.650000000000034772, 2.500000000000000000, 6.495190528383297135 ) ) ;
#38414 = ORIENTED_EDGE ( 'NONE', *, *, #50966, .T. ) ;
#38415 = CARTESIAN_POINT ( 'NONE',  ( -7.500000000000016875, 2.500000000000000000, 0.6928203230275494784 ) ) ;
#38416 = ADVANCED_FACE ( 'NONE', ( #126058 ), #67111, .T. ) ;
#38417 = ORIENTED_EDGE ( 'NONE', *, *, #71786, .T. ) ;
#38418 = ORIENTED_EDGE ( 'NONE', *, *, #69846, .F. ) ;
#38419 = CIRCLE ( 'NONE', #11294, 0.06509327318403745899 ) ;
#38420 = CIRCLE ( 'NONE', #59351, 0.1000000000000002554 ) ;
#38421 = DIRECTION ( 'NONE',  ( 0.000000000000000000, 1.000000000000000000, 0.000000000000000000 ) ) ;
#38422 = DIRECTION ( 'NONE',  ( -0.000000000000000000, 1.000000000000000000, -0.000000000000000000 ) ) ;
#38423 = FACE_OUTER_BOUND ( 'NONE', #97391, .T. ) ;
#38424 = DIRECTION ( 'NONE',  ( 0.000000000000000000, -0.9999939076577903929, 0.003490651415223739937 ) ) ;
#38425 = CARTESIAN_POINT ( 'NONE',  ( -14.79999999999998295, 12.50000000000000000, -0.3464101615137760715 ) ) ;
#38426 = DIRECTION ( 'NONE',  ( 0.000000000000000000, 0.000000000000000000, 1.000000000000000000 ) ) ;
#38427 = EDGE_CURVE ( 'NONE', #49328, #21207, #7670, .T. ) ;
#38428 = AXIS2_PLACEMENT_3D ( 'NONE', #69672, #109611, #10114 ) ;
#38429 = CARTESIAN_POINT ( 'NONE',  ( -0.6500000000000403233, 2.500000000000000000, 1.918653347947321564 ) ) ;
#38430 = CONICAL_SURFACE ( 'NONE', #88577, 0.1000000000000002554, 0.003490658503988666988 ) ;
#38431 = DIRECTION ( 'NONE',  ( 0.000000000000000000, -0.9999939076577903929, 0.003490651415223739937 ) ) ;
#38432 = DIRECTION ( 'NONE',  ( 0.000000000000000000, -0.9999939076577903929, 0.003490651415223739937 ) ) ;
#38433 = VECTOR ( 'NONE', #53868, 1000.000000000000000 ) ;
#38434 = DIRECTION ( 'NONE',  ( 0.000000000000000000, 0.000000000000000000, 1.000000000000000000 ) ) ;
#38435 = CIRCLE ( 'NONE', #113731, 0.06509327318403745899 ) ;
#38436 = CIRCLE ( 'NONE', #94845, 0.09999999999999999167 ) ;
#38437 = AXIS2_PLACEMENT_3D ( 'NONE', #67599, #8038, #107543 ) ;
#38438 = VERTEX_POINT ( 'NONE', #97251 ) ;
#38439 = PLANE ( 'NONE',  #84236 ) ;
#38440 = DIRECTION ( 'NONE',  ( -0.000000000000000000, -1.000000000000000000, -0.000000000000000000 ) ) ;
#38441 = FACE_OUTER_BOUND ( 'NONE', #64951, .T. ) ;
#38442 = LINE ( 'NONE', #108438, #10757 ) ;
#38443 = FACE_OUTER_BOUND ( 'NONE', #104548, .T. ) ;
#38444 = ORIENTED_EDGE ( 'NONE', *, *, #83133, .T. ) ;
#38445 = DIRECTION ( 'NONE',  ( 0.000000000000000000, 0.000000000000000000, -1.000000000000000000 ) ) ;
#38446 = CARTESIAN_POINT ( 'NONE',  ( 185.2500000000000000, 9.429780353434619030E-16, -7.700000000000000178 ) ) ;
#38448 = ORIENTED_EDGE ( 'NONE', *, *, #20447, .T. ) ;
#38447 = LINE ( 'NONE', #128769, #73502 ) ;
#38449 = AXIS2_PLACEMENT_3D ( 'NONE', #23008, #62296, #102215 ) ;
#38450 = ORIENTED_EDGE ( 'NONE', *, *, #90511, .F. ) ;
#38451 = CARTESIAN_POINT ( 'NONE',  ( -6.900000000000019007, 12.50000000000000000, -3.983716857408426293 ) ) ;
#38452 = EDGE_CURVE ( 'NONE', #55284, #70524, #44080, .T. ) ;
#38453 = ORIENTED_EDGE ( 'NONE', *, *, #41465, .F. ) ;
#38454 = ORIENTED_EDGE ( 'NONE', *, *, #114417, .T. ) ;
#38455 = EDGE_LOOP ( 'NONE', ( #108958, #128699 ) ) ;
#38456 = CARTESIAN_POINT ( 'NONE',  ( 4.149999999999938183, 2.500000000000000000, 2.065063509461097624 ) ) ;
#38457 = CARTESIAN_POINT ( 'NONE',  ( 0.6499999999999561684, 12.50000000000000000, -1.753560074763288457 ) ) ;
#38458 = DIRECTION ( 'NONE',  ( 0.000000000000000000, 1.000000000000000000, 0.000000000000000000 ) ) ;
#38459 = AXIS2_PLACEMENT_3D ( 'NONE', #39479, #119289, #117323 ) ;
#38460 = DIRECTION ( 'NONE',  ( -0.000000000000000000, 1.000000000000000000, -0.000000000000000000 ) ) ;
#38461 = ADVANCED_FACE ( 'NONE', ( #71661 ), #80949, .T. ) ;
#38462 = AXIS2_PLACEMENT_3D ( 'NONE', #125070, #76619, #85777 ) ;
#38463 = ORIENTED_EDGE ( 'NONE', *, *, #112053, .T. ) ;
#38464 = CARTESIAN_POINT ( 'NONE',  ( 9.599999999999914380, 2.500000000000000000, 4.330127018922196314 ) ) ;
#38465 = ORIENTED_EDGE ( 'NONE', *, *, #93932, .F. ) ;
#38466 = PLANE ( 'NONE',  #62231 ) ;
#38467 = CARTESIAN_POINT ( 'NONE',  ( 6.449999999999931788, 2.500000000000000000, -6.148780366869526226 ) ) ;
#38468 = EDGE_CURVE ( 'NONE', #20444, #13136, #62177, .T. ) ;
#38469 = CARTESIAN_POINT ( 'NONE',  ( 18.37149739119579905, 2.540880845002019495, 2.596776292459959112 ) ) ;
#38470 = PLANE ( 'NONE',  #75622 ) ;
#38471 = DIRECTION ( 'NONE',  ( -4.274815082592931898E-19, -0.9999939076577903929, -0.003490651415223739937 ) ) ;
#38472 = CONICAL_SURFACE ( 'NONE', #111610, 0.1000000000000000472, 0.003490658503988666988 ) ;
#38473 = EDGE_CURVE ( 'NONE', #79548, #87068, #111587, .T. ) ;
#38474 = CONICAL_SURFACE ( 'NONE', #126187, 0.1000000000000000472, 0.003490658503988666988 ) ;
#38475 = CONICAL_SURFACE ( 'NONE', #111614, 0.09999999999999999167, 0.003490658503988666988 ) ;
#38476 = ORIENTED_EDGE ( 'NONE', *, *, #126956, .F. ) ;
#38477 = VECTOR ( 'NONE', #120856, 1000.000000000000000 ) ;
#38478 = ORIENTED_EDGE ( 'NONE', *, *, #60804, .F. ) ;
#38480 = EDGE_LOOP ( 'NONE', ( #40107, #42324, #73795, #96454 ) ) ;
#38479 = EDGE_CURVE ( 'NONE', #16041, #128284, #89356, .T. ) ;
#38481 = ORIENTED_EDGE ( 'NONE', *, *, #43334, .F. ) ;
#38482 = EDGE_LOOP ( 'NONE', ( #122900, #29515 ) ) ;
#38483 = FACE_OUTER_BOUND ( 'NONE', #41780, .T. ) ;
#38484 = DIRECTION ( 'NONE',  ( -0.000000000000000000, -1.000000000000000000, -0.000000000000000000 ) ) ;
#38485 = DIRECTION ( 'NONE',  ( -0.000000000000000000, -1.000000000000000000, -0.000000000000000000 ) ) ;
#38486 = ADVANCED_FACE ( 'NONE', ( #99848 ), #106075, .T. ) ;
#38487 = FACE_BOUND ( 'NONE', #39878, .T. ) ;
#38488 = DIRECTION ( 'NONE',  ( 0.000000000000000000, -0.000000000000000000, 1.000000000000000000 ) ) ;
#38489 = DIRECTION ( 'NONE',  ( -0.000000000000000000, 1.000000000000000000, -0.000000000000000000 ) ) ;
#38490 = PLANE ( 'NONE',  #69872 ) ;
#38491 = PLANE ( 'NONE',  #87654 ) ;
#38492 = AXIS2_PLACEMENT_3D ( 'NONE', #114751, #75473, #66930 ) ;
#38493 = CONICAL_SURFACE ( 'NONE', #53054, 0.09999999999999982514, 0.003490658503988666988 ) ;
#38494 = AXIS2_PLACEMENT_3D ( 'NONE', #19119, #40081, #78063 ) ;
#38495 = CARTESIAN_POINT ( 'NONE',  ( 184.1302083336747160, -4.367472073101514418, -7.564683531250002702 ) ) ;
#38496 = CARTESIAN_POINT ( 'NONE',  ( -9.150000000000009237, 12.50000000000000000, 2.857883832488649301 ) ) ;
#38497 = AXIS2_PLACEMENT_3D ( 'NONE', #29641, #40112, #57163 ) ;
#38498 = DIRECTION ( 'NONE',  ( 0.000000000000000000, 1.000000000000000000, 0.000000000000000000 ) ) ;
#38499 = AXIS2_PLACEMENT_3D ( 'NONE', #1747, #82265, #2376 ) ;
#38500 = CARTESIAN_POINT ( 'NONE',  ( -12.89999999999999147, 12.50000000000000000, -0.06509327318403558549 ) ) ;
#38501 = ORIENTED_EDGE ( 'NONE', *, *, #20882, .T. ) ;
#38502 = EDGE_LOOP ( 'NONE', ( #103723, #1242 ) ) ;
#38503 = VERTEX_POINT ( 'NONE', #120125 ) ;
#38504 = ORIENTED_EDGE ( 'NONE', *, *, #100524, .T. ) ;
#38505 = DIRECTION ( 'NONE',  ( -0.000000000000000000, -1.000000000000000000, -0.000000000000000000 ) ) ;
#38506 = FACE_BOUND ( 'NONE', #53234, .T. ) ;
#38507 = CARTESIAN_POINT ( 'NONE',  ( 5.649999999999934630, 2.500000000000000000, -2.511473670974877948 ) ) ;
#38508 = VECTOR ( 'NONE', #110518, 1000.000000000000000 ) ;
#38510 = VERTEX_POINT ( 'NONE', #108989 ) ;
#38509 = AXIS2_PLACEMENT_3D ( 'NONE', #39712, #99258, #48872 ) ;
#38512 = AXIS2_PLACEMENT_3D ( 'NONE', #109825, #20155, #82310 ) ;
#38511 = CARTESIAN_POINT ( 'NONE',  ( 5.849999999999932143, 2.500000000000000000, 1.472243186433545459 ) ) ;
#38513 = DIRECTION ( 'NONE',  ( 0.000000000000000000, -0.9999939076577903929, 0.003490651415223739937 ) ) ;
#38514 = CARTESIAN_POINT ( 'NONE',  ( 10.84999999999990905, 2.500000000000000000, -5.802370205355749988 ) ) ;
#38515 = DIRECTION ( 'NONE',  ( 0.000000000000000000, 0.000000000000000000, 1.000000000000000000 ) ) ;
#38516 = EDGE_LOOP ( 'NONE', ( #84195, #122682 ) ) ;
#38517 = CARTESIAN_POINT ( 'NONE',  ( 18.09027855933890550, 2.526462839860865284, -2.685672775344708718 ) ) ;
#38518 = EDGE_CURVE ( 'NONE', #14289, #39788, #20305, .T. ) ;
#38519 = AXIS2_PLACEMENT_3D ( 'NONE', #35055, #62575, #74959 ) ;
#38520 = VECTOR ( 'NONE', #38944, 1000.000000000000000 ) ;
#38521 = ORIENTED_EDGE ( 'NONE', *, *, #63037, .F. ) ;
#38522 = EDGE_CURVE ( 'NONE', #52139, #34976, #24515, .T. ) ;
#38523 = EDGE_LOOP ( 'NONE', ( #30061, #12707 ) ) ;
#38524 = EDGE_CURVE ( 'NONE', #62921, #86305, #29809, .T. ) ;
#38525 = CARTESIAN_POINT ( 'NONE',  ( 5.649999999999932854, 2.500000000000000000, 2.511473670974873507 ) ) ;
#38526 = PLANE ( 'NONE',  #102006 ) ;
#38528 = EDGE_LOOP ( 'NONE', ( #97212, #18867 ) ) ;
#38527 = ADVANCED_FACE ( 'NONE', ( #19322 ), #69730, .T. ) ;
#38529 = ADVANCED_FACE ( 'NONE', ( #319 ), #129323, .T. ) ;
#38530 = AXIS2_PLACEMENT_3D ( 'NONE', #121019, #90916, #41197 ) ;
#38531 = CIRCLE ( 'NONE', #105408, 0.06509327318403745899 ) ;
#38532 = CARTESIAN_POINT ( 'NONE',  ( -14.59999999999998366, 2.500000000000000000, -0.5928203230275519431 ) ) ;
#38533 = DIRECTION ( 'NONE',  ( 0.000000000000000000, -0.9999939076577903929, 0.003490651415223739937 ) ) ;
#38534 = ORIENTED_EDGE ( 'NONE', *, *, #16877, .T. ) ;
#38536 = EDGE_CURVE ( 'NONE', #53623, #72821, #70374, .T. ) ;
#38535 = CARTESIAN_POINT ( 'NONE',  ( -5.850000000000018296, 2.500000000000000000, 1.472243186433545459 ) ) ;
#38538 = ORIENTED_EDGE ( 'NONE', *, *, #82559, .T. ) ;
#38537 = AXIS2_PLACEMENT_3D ( 'NONE', #98116, #106652, #115829 ) ;
#38539 = FACE_OUTER_BOUND ( 'NONE', #41035, .T. ) ;
#38540 = ORIENTED_EDGE ( 'NONE', *, *, #80290, .F. ) ;
#38541 = DIRECTION ( 'NONE',  ( -0.000000000000000000, -1.000000000000000000, -0.000000000000000000 ) ) ;
#38542 = FACE_BOUND ( 'NONE', #70103, .T. ) ;
#38543 = EDGE_CURVE ( 'NONE', #18013, #32951, #85134, .T. ) ;
#38544 = ADVANCED_FACE ( 'NONE', ( #49468 ), #91399, .T. ) ;
#38545 = EDGE_LOOP ( 'NONE', ( #3228, #95436, #104975, #25242 ) ) ;
#38546 = CARTESIAN_POINT ( 'NONE',  ( 5.849999999999934808, 12.50000000000000000, -5.737276932171712751 ) ) ;
#38547 = EDGE_LOOP ( 'NONE', ( #59247, #399, #113525, #20976 ) ) ;
#38548 = DIRECTION ( 'NONE',  ( 0.000000000000000000, 0.000000000000000000, 1.000000000000000000 ) ) ;
#38549 = LINE ( 'NONE', #28060, #123986 ) ;
#38550 = FACE_OUTER_BOUND ( 'NONE', #125917, .T. ) ;
#38551 = CARTESIAN_POINT ( 'NONE',  ( -10.20000000000000639, 2.500000000000000000, -3.983716857408421852 ) ) ;
#38552 = CARTESIAN_POINT ( 'NONE',  ( 17.50000000000000355, 2.413248583741727682, -3.595440551767597359 ) ) ;
#38553 = EDGE_LOOP ( 'NONE', ( #1896, #79302 ) ) ;
#38554 = ORIENTED_EDGE ( 'NONE', *, *, #74097, .F. ) ;
#38555 = ORIENTED_EDGE ( 'NONE', *, *, #60912, .F. ) ;
#38556 = FACE_OUTER_BOUND ( 'NONE', #111898, .T. ) ;
#38557 = CARTESIAN_POINT ( 'NONE',  ( 11.64999999999990621, 2.500000000000000000, 6.595190528383296780 ) ) ;
#38558 = CARTESIAN_POINT ( 'NONE',  ( 3.099999999999945022, 2.500000000000000000, -0.4464101615137783252 ) ) ;
#38560 = ORIENTED_EDGE ( 'NONE', *, *, #118102, .T. ) ;
#38559 = ORIENTED_EDGE ( 'NONE', *, *, #71565, .T. ) ;
#38561 = EDGE_LOOP ( 'NONE', ( #88918, #5885 ) ) ;
#38562 = LINE ( 'NONE', #60132, #35212 ) ;
#38563 = CIRCLE ( 'NONE', #65623, 0.06509327318403741736 ) ;
#38564 = PLANE ( 'NONE',  #115483 ) ;
#38565 = VECTOR ( 'NONE', #40590, 1000.000000000000000 ) ;
#38566 = ITEM_DEFINED_TRANSFORMATION ( 'NONE', 'NONE', #58845,  #108296 ) ;
#38567 = FACE_OUTER_BOUND ( 'NONE', #68785, .T. ) ;
#38568 = FACE_OUTER_BOUND ( 'NONE', #12672, .T. ) ;
#38569 = CARTESIAN_POINT ( 'NONE',  ( 7.949999999999925571, 2.500000000000000000, -6.595190528383302109 ) ) ;
#38570 = CARTESIAN_POINT ( 'NONE',  ( -12.49999999999999467, 12.50000000000000000, -3.702399969078684627 ) ) ;
#38571 = DIRECTION ( 'NONE',  ( -1.000000000000000000, 0.000000000000000000, 1.084202172485504434E-16 ) ) ;
#38572 = DIRECTION ( 'NONE',  ( 0.000000000000000000, 0.000000000000000000, -1.000000000000000000 ) ) ;
#38573 = EDGE_LOOP ( 'NONE', ( #95881, #80814 ) ) ;
#38574 = ORIENTED_EDGE ( 'NONE', *, *, #1295, .T. ) ;
#38575 = AXIS2_PLACEMENT_3D ( 'NONE', #8799, #76272, #116824 ) ;
#38576 = DIRECTION ( 'NONE',  ( 0.000000000000000000, 0.000000000000000000, -1.000000000000000000 ) ) ;
#38577 = LINE ( 'NONE', #28743, #57051 ) ;
#38578 = VERTEX_POINT ( 'NONE', #41585 ) ;
#38579 = EDGE_LOOP ( 'NONE', ( #127153, #92468, #27256, #23442 ) ) ;
#38580 = CARTESIAN_POINT ( 'NONE',  ( 187.2343750003414016, 8.734944146203032389, 5.348610694689227483E-16 ) ) ;
#38581 = CARTESIAN_POINT ( 'NONE',  ( -4.800000000000022915, 12.50000000000000000, 3.983716857408420076 ) ) ;
#38582 = DIRECTION ( 'NONE',  ( 0.000000000000000000, 1.000000000000000000, 0.000000000000000000 ) ) ;
#38583 = DIRECTION ( 'NONE',  ( 0.000000000000000000, 0.000000000000000000, 1.000000000000000000 ) ) ;
#38584 = EDGE_CURVE ( 'NONE', #82532, #51256, #47501, .T. ) ;
#38585 = AXIS2_PLACEMENT_3D ( 'NONE', #56319, #26236, #5915 ) ;
#38586 = DIRECTION ( 'NONE',  ( 0.000000000000000000, 0.000000000000000000, -1.000000000000000000 ) ) ;
#38587 = VECTOR ( 'NONE', #67110, 1000.000000000000000 ) ;
#38588 = CARTESIAN_POINT ( 'NONE',  ( 14.34999999999989662, 12.50000000000000000, 1.753560074763284016 ) ) ;
#38589 = DIRECTION ( 'NONE',  ( 0.000000000000000000, 0.000000000000000000, -1.000000000000000000 ) ) ;
#38590 = CIRCLE ( 'NONE', #122196, 0.06509327318403745899 ) ;
#38591 = AXIS2_PLACEMENT_3D ( 'NONE', #106398, #73706, #55375 ) ;
#38592 = FACE_OUTER_BOUND ( 'NONE', #29511, .T. ) ;
#38593 = VERTEX_POINT ( 'NONE', #59289 ) ;
#38594 = ORIENTED_EDGE ( 'NONE', *, *, #113141, .F. ) ;
#38595 = ORIENTED_EDGE ( 'NONE', *, *, #123882, .F. ) ;
#38596 = VERTEX_POINT ( 'NONE', #40943 ) ;
#38597 = CARTESIAN_POINT ( 'NONE',  ( 13.74999999999989875, 12.50000000000000000, 1.472243186433545459 ) ) ;
#38598 = CARTESIAN_POINT ( 'NONE',  ( 1.249999999999950262, 12.50000000000000000, 7.122917578226811486 ) ) ;
#38599 = EDGE_LOOP ( 'NONE', ( #89384, #97238, #11562, #1021 ) ) ;
#38600 = LINE ( 'NONE', #70615, #36080 ) ;
#38601 = DIRECTION ( 'NONE',  ( -0.000000000000000000, -1.000000000000000000, -0.000000000000000000 ) ) ;
#38602 = VECTOR ( 'NONE', #50459, 1000.000000000000000 ) ;
#38603 = AXIS2_PLACEMENT_3D ( 'NONE', #118249, #79616, #69138 ) ;
#38604 = DIRECTION ( 'NONE',  ( -0.000000000000000000, 1.000000000000000000, -0.000000000000000000 ) ) ;
#38606 = EDGE_LOOP ( 'NONE', ( #34021, #106470, #46297, #97542 ) ) ;
#38605 = DIRECTION ( 'NONE',  ( 0.000000000000000000, 0.000000000000000000, 1.000000000000000000 ) ) ;
#38607 = AXIS2_PLACEMENT_3D ( 'NONE', #44845, #104399, #54637 ) ;
#38608 = CIRCLE ( 'NONE', #128485, 0.06509327318403745899 ) ;
#38609 = CARTESIAN_POINT ( 'NONE',  ( -7.050000000000013145, 12.50000000000000000, 6.560283801567334372 ) ) ;
#38610 = DIRECTION ( 'NONE',  ( 0.000000000000000000, 0.000000000000000000, 1.000000000000000000 ) ) ;
#38611 = ORIENTED_EDGE ( 'NONE', *, *, #4144, .F. ) ;
#38612 = CONICAL_SURFACE ( 'NONE', #69894, 0.1000000000000000472, 0.003490658503988666988 ) ;
#38613 = AXIS2_PLACEMENT_3D ( 'NONE', #64892, #104808, #124477 ) ;
#38614 = CIRCLE ( 'NONE', #78414, 0.06509327318403745899 ) ;
#38615 = ORIENTED_EDGE ( 'NONE', *, *, #21917, .F. ) ;
#38616 = ORIENTED_EDGE ( 'NONE', *, *, #38207, .F. ) ;
#38617 = CARTESIAN_POINT ( 'NONE',  ( -11.24999999999999822, 12.50000000000000000, 1.472243186433545459 ) ) ;
#38618 = AXIS2_PLACEMENT_3D ( 'NONE', #87031, #67359, #126967 ) ;
#38619 = LINE ( 'NONE', #117773, #35765 ) ;
#38620 = AXIS2_PLACEMENT_3D ( 'NONE', #57559, #7797, #97473 ) ;
#38622 = ADVANCED_FACE ( 'NONE', ( #99201 ), #49665, .T. ) ;
#38621 = AXIS2_PLACEMENT_3D ( 'NONE', #63446, #103372, #70685 ) ;
#38623 = CIRCLE ( 'NONE', #36568, 0.1000000000000002554 ) ;
#38624 = VERTEX_POINT ( 'NONE', #89378 ) ;
#38625 = CARTESIAN_POINT ( 'NONE',  ( 108.0000000000000142, 9.000000000000001776, -2.749999999999997335 ) ) ;
#38626 = DIRECTION ( 'NONE',  ( -0.000000000000000000, -1.000000000000000000, -0.000000000000000000 ) ) ;
#38627 = EDGE_CURVE ( 'NONE', #122449, #46062, #39210, .T. ) ;
#38628 = DIRECTION ( 'NONE',  ( -4.274815082592931898E-19, -0.9999939076577903929, -0.003490651415223739937 ) ) ;
#38629 = DIRECTION ( 'NONE',  ( -0.000000000000000000, -1.000000000000000000, -0.000000000000000000 ) ) ;
#38630 = EDGE_CURVE ( 'NONE', #66522, #53654, #108126, .T. ) ;
#38631 = EDGE_LOOP ( 'NONE', ( #66924, #7163 ) ) ;
#38632 = DIRECTION ( 'NONE',  ( 0.000000000000000000, 0.000000000000000000, 1.000000000000000000 ) ) ;
#38633 = ORIENTED_EDGE ( 'NONE', *, *, #83144, .F. ) ;
#38634 = ADVANCED_FACE ( 'NONE', ( #54580 ), #94515, .T. ) ;
#38636 = ORIENTED_EDGE ( 'NONE', *, *, #32181, .F. ) ;
#38635 = EDGE_CURVE ( 'NONE', #36662, #53828, #82700, .T. ) ;
#38637 = PLANE ( 'NONE',  #72973 ) ;
#38638 = EDGE_CURVE ( 'NONE', #75229, #85897, #124862, .T. ) ;
#38639 = DIRECTION ( 'NONE',  ( 0.000000000000000000, -0.000000000000000000, 1.000000000000000000 ) ) ;
#38640 = EDGE_CURVE ( 'NONE', #16894, #76479, #60133, .T. ) ;
#38641 = FACE_BOUND ( 'NONE', #124560, .T. ) ;
#38642 = CARTESIAN_POINT ( 'NONE',  ( -3.150000000000030109, 2.500000000000000000, 1.718653347947321386 ) ) ;
#38643 = CIRCLE ( 'NONE', #69921, 0.1000000000000000056 ) ;
#38644 = DIRECTION ( 'NONE',  ( 0.000000000000000000, 0.000000000000000000, 1.000000000000000000 ) ) ;
#38645 = FACE_OUTER_BOUND ( 'NONE', #31608, .T. ) ;
#38646 = VERTEX_POINT ( 'NONE', #52035 ) ;
#38647 = FACE_OUTER_BOUND ( 'NONE', #107100, .T. ) ;
#38648 = DIRECTION ( 'NONE',  ( 0.000000000000000000, -0.9999939076577903929, 0.003490651415223739937 ) ) ;
#38649 = ADVANCED_FACE ( 'NONE', ( #123343 ), #112337, .T. ) ;
#38650 = CARTESIAN_POINT ( 'NONE',  ( 12.49999999999990408, 12.50000000000000000, 5.022947341949748790 ) ) ;
#38651 = CARTESIAN_POINT ( 'NONE',  ( -0.6500000000000403233, 12.50000000000000000, 1.818653347947321475 ) ) ;
#38652 = VERTEX_POINT ( 'NONE', #82128 ) ;
#38653 = CONICAL_SURFACE ( 'NONE', #44896, 0.1000000000000002554, 0.003490658503988666988 ) ;
#38654 = AXIS2_PLACEMENT_3D ( 'NONE', #29948, #58760, #88860 ) ;
#38655 = CARTESIAN_POINT ( 'NONE',  ( 187.5000000000000000, 1.500000000000000000, 6.000000000000000000 ) ) ;
#38656 = DIRECTION ( 'NONE',  ( -0.000000000000000000, -1.000000000000000000, -0.000000000000000000 ) ) ;
#38657 = EDGE_LOOP ( 'NONE', ( #40508, #34558, #98773, #89133 ) ) ;
#38658 = ORIENTED_EDGE ( 'NONE', *, *, #75847, .T. ) ;
#38659 = LINE ( 'NONE', #58920, #83634 ) ;
#38660 = CARTESIAN_POINT ( 'NONE',  ( 3.149999999999946176, 2.500000000000000000, -6.048780366869526581 ) ) ;
#38661 = FACE_BOUND ( 'NONE', #106981, .T. ) ;
#38662 = CARTESIAN_POINT ( 'NONE',  ( 13.39473262249371999, -2.500000000000000000, -7.044698190877974220 ) ) ;
#38663 = ORIENTED_EDGE ( 'NONE', *, *, #103174, .F. ) ;
#38664 = DIRECTION ( 'NONE',  ( -0.000000000000000000, -1.000000000000000000, -0.000000000000000000 ) ) ;
#38665 = CONICAL_SURFACE ( 'NONE', #26035, 0.1000000000000002554, 0.003490658503988666988 ) ;
#38666 = ORIENTED_EDGE ( 'NONE', *, *, #60516, .T. ) ;
#38667 = VERTEX_POINT ( 'NONE', #113514 ) ;
#38669 = ADVANCED_FACE ( 'NONE', ( #53328 ), #76841, .T. ) ;
#38668 = DIRECTION ( 'NONE',  ( 0.000000000000000000, 1.000000000000000000, 0.000000000000000000 ) ) ;
#38670 = CARTESIAN_POINT ( 'NONE',  ( 185.7083333333333428, -4.445597072760115509, -7.700000000000001954 ) ) ;
#38671 = ORIENTED_EDGE ( 'NONE', *, *, #4630, .F. ) ;
#38672 = CARTESIAN_POINT ( 'NONE',  ( -6.650000000000018119, 12.50000000000000000, -2.099970236277064473 ) ) ;
#38673 = CARTESIAN_POINT ( 'NONE',  ( -1.850000000000033396, 2.500000000000000000, -6.248780366869526759 ) ) ;
#38674 = VECTOR ( 'NONE', #81141, 1000.000000000000000 ) ;
#38675 = AXIS2_PLACEMENT_3D ( 'NONE', #117500, #108987, #118178 ) ;
#38676 = EDGE_CURVE ( 'NONE', #97603, #96273, #32417, .T. ) ;
#38677 = DIRECTION ( 'NONE',  ( 0.000000000000000000, -0.000000000000000000, 1.000000000000000000 ) ) ;
#38678 = DIRECTION ( 'NONE',  ( -0.000000000000000000, -1.000000000000000000, -0.000000000000000000 ) ) ;
#38679 = EDGE_CURVE ( 'NONE', #122539, #58927, #22480, .T. ) ;
#38680 = AXIS2_PLACEMENT_3D ( 'NONE', #63097, #20608, #100448 ) ;
#38681 = ORIENTED_EDGE ( 'NONE', *, *, #46154, .T. ) ;
#38682 = EDGE_CURVE ( 'NONE', #63649, #125318, #52662, .T. ) ;
#38683 = FACE_OUTER_BOUND ( 'NONE', #104219, .T. ) ;
#38684 = LINE ( 'NONE', #57661, #68567 ) ;
#38685 = LINE ( 'NONE', #11114, #34621 ) ;
#38686 = DIRECTION ( 'NONE',  ( 0.000000000000000000, 0.000000000000000000, -1.000000000000000000 ) ) ;
#38687 = ORIENTED_EDGE ( 'NONE', *, *, #71579, .F. ) ;
#38688 = CARTESIAN_POINT ( 'NONE',  ( -7.100000000000017408, 12.50000000000000000, -0.7579135962115917113 ) ) ;
#38689 = ORIENTED_EDGE ( 'NONE', *, *, #34196, .T. ) ;
#38690 = EDGE_CURVE ( 'NONE', #129208, #98964, #126924, .T. ) ;
#38691 = DIRECTION ( 'NONE',  ( 0.000000000000000000, 0.000000000000000000, 1.000000000000000000 ) ) ;
#38693 = VERTEX_POINT ( 'NONE', #103712 ) ;
#38692 = ADVANCED_FACE ( 'NONE', ( #22591 ), #14029, .T. ) ;
#38694 = PLANE ( 'NONE',  #128783 ) ;
#38695 = CARTESIAN_POINT ( 'NONE',  ( 87.50000000000002842, -7.499999999999997335, 0.6928095518838454092 ) ) ;
#38696 = EDGE_CURVE ( 'NONE', #11963, #9662, #87188, .T. ) ;
#38697 = CARTESIAN_POINT ( 'NONE',  ( 7.899999999999923084, 2.500000000000000000, -0.6928203230275542523 ) ) ;
#38698 = ADVANCED_FACE ( 'NONE', ( #4188 ), #64208, .T. ) ;
#38700 = CARTESIAN_POINT ( 'NONE',  ( -7.300000000000018474, 2.500000000000000000, 0.2464101615137735679 ) ) ;
#38699 = AXIS2_PLACEMENT_3D ( 'NONE', #69962, #70601, #50316 ) ;
#38701 = ORIENTED_EDGE ( 'NONE', *, *, #8043, .T. ) ;
#38702 = AXIS2_PLACEMENT_3D ( 'NONE', #118739, #9440, #70296 ) ;
#38703 = DIRECTION ( 'NONE',  ( -0.000000000000000000, -1.000000000000000000, -0.000000000000000000 ) ) ;
#38704 = DIRECTION ( 'NONE',  ( -0.000000000000000000, -1.000000000000000000, -0.000000000000000000 ) ) ;
#38705 = CARTESIAN_POINT ( 'NONE',  ( 9.999999999999948486, 2.500000000000000000, -4.230127018922201998 ) ) ;
#38706 = CIRCLE ( 'NONE', #53353, 0.06509327318403745899 ) ;
#38707 = CARTESIAN_POINT ( 'NONE',  ( -6.850000000000017408, 2.500000000000000000, -1.818653347947325916 ) ) ;
#38708 = CARTESIAN_POINT ( 'NONE',  ( -2.499999999999996447, 12.50000000000000000, 4.330127018922196314 ) ) ;
#38710 = EDGE_CURVE ( 'NONE', #120555, #21815, #24498, .T. ) ;
#38709 = DIRECTION ( 'NONE',  ( 0.000000000000000000, 1.000000000000000000, 0.000000000000000000 ) ) ;
#38711 = AXIS2_PLACEMENT_3D ( 'NONE', #40830, #8267, #11980 ) ;
#38712 = ORIENTED_EDGE ( 'NONE', *, *, #38627, .F. ) ;
#38713 = EDGE_LOOP ( 'NONE', ( #21252, #63195, #84803, #106965 ) ) ;
#38715 = DIRECTION ( 'NONE',  ( -0.000000000000000000, -1.000000000000000000, -0.000000000000000000 ) ) ;
#38714 = AXIS2_PLACEMENT_3D ( 'NONE', #78818, #19213, #59172 ) ;
#38716 = EDGE_LOOP ( 'NONE', ( #113800, #48859, #14993, #44222 ) ) ;
#38717 = DIRECTION ( 'NONE',  ( 0.000000000000000000, -0.000000000000000000, 1.000000000000000000 ) ) ;
#38720 = VERTEX_POINT ( 'NONE', #34985 ) ;
#38719 = ORIENTED_EDGE ( 'NONE', *, *, #20049, .T. ) ;
#38718 = CONICAL_SURFACE ( 'NONE', #51222, 0.09999999999999982514, 0.003490658503988666988 ) ;
#38721 = ORIENTED_EDGE ( 'NONE', *, *, #18086, .F. ) ;
#38722 = CARTESIAN_POINT ( 'NONE',  ( -3.350000000000028955, 2.500000000000000000, -2.265063509461101798 ) ) ;
#38723 = AXIS2_PLACEMENT_3D ( 'NONE', #113088, #84270, #85562 ) ;
#38725 = CONICAL_SURFACE ( 'NONE', #78424, 0.1000000000000002554, 0.003490658503988666988 ) ;
#38724 = CARTESIAN_POINT ( 'NONE',  ( 7.699999999999923794, 2.500000000000000000, -3.983716857408426293 ) ) ;
#38726 = DIRECTION ( 'NONE',  ( 0.000000000000000000, 0.000000000000000000, 1.000000000000000000 ) ) ;
#38727 = SHAPE_REPRESENTATION_RELATIONSHIP ( 'NONE' , 'NONE' ,  #18450, #25840 ) ;
#38728 = FACE_OUTER_BOUND ( 'NONE', #66481, .T. ) ;
#38729 = CARTESIAN_POINT ( 'NONE',  ( 14.54999999999989591, 12.50000000000000000, 2.099970236277060032 ) ) ;
#38730 = CIRCLE ( 'NONE', #9453, 0.09999999999999982514 ) ;
#38731 = DIRECTION ( 'NONE',  ( 0.000000000000000000, -0.000000000000000000, 1.000000000000000000 ) ) ;
#38732 = CARTESIAN_POINT ( 'NONE',  ( 6.899999999999926636, 2.500000000000000000, 0.4464101615137736623 ) ) ;
#38733 = DIRECTION ( 'NONE',  ( -4.274815082592931898E-19, -0.9999939076577903929, -0.003490651415223739937 ) ) ;
#38734 = ORIENTED_EDGE ( 'NONE', *, *, #14093, .F. ) ;
#38735 = ORIENTED_EDGE ( 'NONE', *, *, #44980, .F. ) ;
#38736 = ORIENTED_EDGE ( 'NONE', *, *, #116818, .F. ) ;
#38737 = DIRECTION ( 'NONE',  ( 0.000000000000000000, 0.000000000000000000, 1.000000000000000000 ) ) ;
#38738 = ORIENTED_EDGE ( 'NONE', *, *, #5469, .F. ) ;
#38739 = EDGE_LOOP ( 'NONE', ( #79061, #101615, #12936, #43714 ) ) ;
#38740 = LINE ( 'NONE', #100211, #44105 ) ;
#38741 = VECTOR ( 'NONE', #40775, 1000.000000000000000 ) ;
#38742 = CARTESIAN_POINT ( 'NONE',  ( -5.450000000000019718, 2.500000000000000000, 6.495190528383297135 ) ) ;
#38743 = EDGE_CURVE ( 'NONE', #23431, #30816, #48017, .T. ) ;
#38745 = DIRECTION ( 'NONE',  ( 0.000000000000000000, 1.000000000000000000, 0.000000000000000000 ) ) ;
#38744 = PRODUCT ( 'BR-831', 'BR-831', '', ( #68636 ) ) ;
#38746 = DIRECTION ( 'NONE',  ( 0.000000000000000000, 0.000000000000000000, 1.000000000000000000 ) ) ;
#38747 = CARTESIAN_POINT ( 'NONE',  ( -6.900000000000019007, 2.500000000000000000, 0.3464101615137735735 ) ) ;
#38748 = ORIENTED_EDGE ( 'NONE', *, *, #127322, .F. ) ;
#38749 = AXIS2_PLACEMENT_3D ( 'NONE', #42051, #81959, #101618 ) ;
#38750 = CARTESIAN_POINT ( 'NONE',  ( 8.549999999999924327, 12.50000000000000000, -6.841600689897077814 ) ) ;
#38751 = AXIS2_PLACEMENT_3D ( 'NONE', #99202, #49469, #89379 ) ;
#38752 = AXIS2_PLACEMENT_3D ( 'NONE', #28011, #69203, #109121 ) ;
#38753 = ORIENTED_EDGE ( 'NONE', *, *, #38194, .T. ) ;
#38754 = CARTESIAN_POINT ( 'NONE',  ( -13.54999999999999005, 2.500000000000000000, -1.918653347947324006 ) ) ;
#38755 = ORIENTED_EDGE ( 'NONE', *, *, #77643, .F. ) ;
#38756 = LINE ( 'NONE', #37450, #33742 ) ;
#38757 = ORIENTED_EDGE ( 'NONE', *, *, #48232, .T. ) ;
#38758 = EDGE_CURVE ( 'NONE', #107667, #37222, #1514, .T. ) ;
#38759 = ORIENTED_EDGE ( 'NONE', *, *, #16646, .F. ) ;
#38760 = DIRECTION ( 'NONE',  ( 0.000000000000000000, 0.000000000000000000, 1.000000000000000000 ) ) ;
#38761 = CARTESIAN_POINT ( 'NONE',  ( 76.44220535186029508, -3.905138931494386956, -5.869652189505990769 ) ) ;
#38762 = AXIS2_PLACEMENT_3D ( 'NONE', #26862, #77879, #46488 ) ;
#38763 = LINE ( 'NONE', #78673, #109335 ) ;
#38764 = CARTESIAN_POINT ( 'NONE',  ( -12.69999999999999218, 12.50000000000000000, 4.676537180435972552 ) ) ;
#38765 = VECTOR ( 'NONE', #94188, 1000.000000000000000 ) ;
#38766 = DIRECTION ( 'NONE',  ( -0.000000000000000000, -1.000000000000000000, -0.000000000000000000 ) ) ;
#38767 = EDGE_LOOP ( 'NONE', ( #7276, #15895 ) ) ;
#38768 = CARTESIAN_POINT ( 'NONE',  ( 6.849999999999930367, 12.50000000000000000, -6.148780366869526226 ) ) ;
#38769 = CARTESIAN_POINT ( 'NONE',  ( -9.150000000000009237, 2.500000000000000000, 2.857883832488649301 ) ) ;
#38770 = CARTESIAN_POINT ( 'NONE',  ( 11.04999999999991189, 2.500000000000000000, 6.048780366869521252 ) ) ;
#38771 = CARTESIAN_POINT ( 'NONE',  ( -0.4000000000000401013, 2.500000000000000000, -3.637306695894650055 ) ) ;
#38772 = DIRECTION ( 'NONE',  ( 0.000000000000000000, 0.000000000000000000, 1.000000000000000000 ) ) ;
#38773 = ORIENTED_EDGE ( 'NONE', *, *, #90994, .F. ) ;
#38774 = CIRCLE ( 'NONE', #7335, 0.06509327318403745899 ) ;
#38775 = AXIS2_PLACEMENT_3D ( 'NONE', #49316, #59782, #19159 ) ;
#38776 = ORIENTED_EDGE ( 'NONE', *, *, #36886, .F. ) ;
#38777 = CARTESIAN_POINT ( 'NONE',  ( -6.850000000000017408, 2.500000000000000000, -6.248780366869526759 ) ) ;
#38778 = EDGE_LOOP ( 'NONE', ( #80295, #122562, #66744, #47976 ) ) ;
#38779 = LINE ( 'NONE', #98958, #128162 ) ;
#38780 = CARTESIAN_POINT ( 'NONE',  ( -9.800000000000007816, 2.500000000000000000, -3.983716857408421852 ) ) ;
#38781 = EDGE_CURVE ( 'NONE', #75194, #75250, #11982, .T. ) ;
#38782 = AXIS2_PLACEMENT_3D ( 'NONE', #82963, #34520, #74431 ) ;
#38783 = VERTEX_POINT ( 'NONE', #45435 ) ;
#38784 = CARTESIAN_POINT ( 'NONE',  ( 184.8750000000000000, 8.891194145520236347, 5.444286225454521982E-16 ) ) ;
#38785 = DIRECTION ( 'NONE',  ( -4.274815082592931898E-19, -0.9999939076577903929, -0.003490651415223739937 ) ) ;
#38786 = CARTESIAN_POINT ( 'NONE',  ( -2.300000000000033573, 12.50000000000000000, -3.983716857408426293 ) ) ;
#38787 = CIRCLE ( 'NONE', #78492, 0.06509327318403741736 ) ;
#38788 = DIRECTION ( 'NONE',  ( -0.000000000000000000, -1.000000000000000000, -0.000000000000000000 ) ) ;
#38789 = ORIENTED_EDGE ( 'NONE', *, *, #101453, .F. ) ;
#38790 = EDGE_CURVE ( 'NONE', #70542, #116584, #74681, .T. ) ;
#38791 = CIRCLE ( 'NONE', #90989, 0.06509327318403745899 ) ;
#38792 = FACE_OUTER_BOUND ( 'NONE', #75030, .T. ) ;
#38793 = CIRCLE ( 'NONE', #38702, 0.06509327318403745899 ) ;
#38794 = EDGE_LOOP ( 'NONE', ( #59155, #9323 ) ) ;
#38795 = ADVANCED_FACE ( 'NONE', ( #38187 ), #125901, .T. ) ;
#38796 = EDGE_CURVE ( 'NONE', #74258, #40987, #67626, .T. ) ;
#38797 = EDGE_CURVE ( 'NONE', #68062, #64597, #24598, .T. ) ;
#38799 = EDGE_CURVE ( 'NONE', #74146, #79205, #127222, .T. ) ;
#38798 = CARTESIAN_POINT ( 'NONE',  ( 35.04033562331356677, 1.562405403454929065, -4.793261083390611077 ) ) ;
#38800 = FACE_OUTER_BOUND ( 'NONE', #49086, .T. ) ;
#38801 = DIRECTION ( 'NONE',  ( 0.000000000000000000, 0.000000000000000000, -1.000000000000000000 ) ) ;
#38802 = VECTOR ( 'NONE', #3457, 1000.000000000000000 ) ;
#38803 = CONICAL_SURFACE ( 'NONE', #7361, 0.1000000000000002554, 0.003490658503988666988 ) ;
#38804 = EDGE_LOOP ( 'NONE', ( #87377, #84539, #1014, #124118 ) ) ;
#38805 = VECTOR ( 'NONE', #93778, 1000.000000000000000 ) ;
#38806 = CARTESIAN_POINT ( 'NONE',  ( -6.450000000000019718, 12.50000000000000000, -6.148780366869526226 ) ) ;
#38807 = CIRCLE ( 'NONE', #76433, 0.1000000000000000472 ) ;
#38808 = VERTEX_POINT ( 'NONE', #76825 ) ;
#38809 = DIRECTION ( 'NONE',  ( 0.000000000000000000, 0.000000000000000000, 1.000000000000000000 ) ) ;
#38810 = DIRECTION ( 'NONE',  ( 0.000000000000000000, 0.000000000000000000, 1.000000000000000000 ) ) ;
#38811 = EDGE_CURVE ( 'NONE', #21177, #112816, #39304, .T. ) ;
#38812 = CARTESIAN_POINT ( 'NONE',  ( 0.5999999999999621192, 12.50000000000000000, 0.2813168883297384459 ) ) ;
#38813 = ORIENTED_EDGE ( 'NONE', *, *, #111519, .F. ) ;
#38814 = EDGE_CURVE ( 'NONE', #119487, #74873, #51801, .T. ) ;
#38815 = CIRCLE ( 'NONE', #107736, 0.09999999999999982514 ) ;
#38816 = AXIS2_PLACEMENT_3D ( 'NONE', #93093, #63627, #51875 ) ;
#38818 = EDGE_CURVE ( 'NONE', #83051, #83715, #77459, .T. ) ;
#38817 = CARTESIAN_POINT ( 'NONE',  ( -5.650000000000019895, 12.50000000000000000, 6.083687093685482772 ) ) ;
#38819 = AXIS2_PLACEMENT_3D ( 'NONE', #93752, #23078, #5356 ) ;
#38820 = DIRECTION ( 'NONE',  ( 0.000000000000000000, 0.000000000000000000, -1.000000000000000000 ) ) ;
#38821 = ORIENTED_EDGE ( 'NONE', *, *, #124057, .T. ) ;
#38822 = CARTESIAN_POINT ( 'NONE',  ( 9.149999999999916866, 2.500000000000000000, -2.857883832488653741 ) ) ;
#38823 = VERTEX_POINT ( 'NONE', #7417 ) ;
#38824 = CARTESIAN_POINT ( 'NONE',  ( 8.099999999999923261, 12.50000000000000000, 3.983716857408420076 ) ) ;
#38825 = EDGE_LOOP ( 'NONE', ( #74035, #115540, #92055, #14706 ) ) ;
#38826 = DIRECTION ( 'NONE',  ( -0.000000000000000000, -1.000000000000000000, -0.000000000000000000 ) ) ;
#38827 = DIRECTION ( 'NONE',  ( 0.000000000000000000, 1.000000000000000000, 0.000000000000000000 ) ) ;
#38828 = ORIENTED_EDGE ( 'NONE', *, *, #4158, .T. ) ;
#38829 = VERTEX_POINT ( 'NONE', #117347 ) ;
#38830 = DIRECTION ( 'NONE',  ( 0.000000000000000000, 0.000000000000000000, -1.000000000000000000 ) ) ;
#38831 = CARTESIAN_POINT ( 'NONE',  ( 0.6499999999999543920, 12.50000000000000000, 6.776507416713035248 ) ) ;
#38832 = CONICAL_SURFACE ( 'NONE', #57594, 0.09999999999999982514, 0.003490658503988666988 ) ;
#38833 = EDGE_LOOP ( 'NONE', ( #46889, #63289 ) ) ;
#38834 = DIRECTION ( 'NONE',  ( 0.000000000000000000, 0.000000000000000000, -1.000000000000000000 ) ) ;
#38835 = PLANE ( 'NONE',  #118251 ) ;
#38836 = CARTESIAN_POINT ( 'NONE',  ( 10.84999999999990905, 2.500000000000000000, 2.165063509461097713 ) ) ;
#38837 = CARTESIAN_POINT ( 'NONE',  ( 104.6953598897069497, 7.846636665918518716, -3.765776865403877682 ) ) ;
#38838 = CARTESIAN_POINT ( 'NONE',  ( -2.700000000000029932, 12.50000000000000000, -0.3464101615137782364 ) ) ;
#38839 = CYLINDRICAL_SURFACE ( 'NONE', #5531, 2.000000000000000000 ) ;
#38840 = AXIS2_PLACEMENT_3D ( 'NONE', #20317, #49792, #60263 ) ;
#38841 = FACE_OUTER_BOUND ( 'NONE', #89490, .T. ) ;
#38842 = AXIS2_PLACEMENT_3D ( 'NONE', #116731, #44796, #14655 ) ;
#38843 = AXIS2_PLACEMENT_3D ( 'NONE', #31878, #113006, #23325 ) ;
#38844 = ORIENTED_EDGE ( 'NONE', *, *, #32499, .T. ) ;
#38845 = ORIENTED_EDGE ( 'NONE', *, *, #69788, .F. ) ;
#38846 = ORIENTED_EDGE ( 'NONE', *, *, #3910, .F. ) ;
#38847 = ORIENTED_EDGE ( 'NONE', *, *, #74665, .T. ) ;
#38848 = CARTESIAN_POINT ( 'NONE',  ( -2.900000000000030109, 2.500000000000000000, 0.6928203230275494784 ) ) ;
#38849 = CARTESIAN_POINT ( 'NONE',  ( -10.60000000000000142, 12.50000000000000000, 3.983716857408420964 ) ) ;
#38850 = DIRECTION ( 'NONE',  ( 0.000000000000000000, 0.000000000000000000, -1.000000000000000000 ) ) ;
#38851 = EDGE_LOOP ( 'NONE', ( #74664, #27304 ) ) ;
#38852 = FACE_BOUND ( 'NONE', #126150, .T. ) ;
#38853 = ORIENTED_EDGE ( 'NONE', *, *, #59792, .F. ) ;
#38854 = EDGE_CURVE ( 'NONE', #75500, #86861, #85348, .T. ) ;
#38855 = CARTESIAN_POINT ( 'NONE',  ( -5.650000000000019895, 12.50000000000000000, 6.841600689897072485 ) ) ;
#38856 = DIRECTION ( 'NONE',  ( -1.000000000000000000, -0.000000000000000000, -0.000000000000000000 ) ) ;
#38857 = AXIS2_PLACEMENT_3D ( 'NONE', #62781, #103349, #51674 ) ;
#38858 = ADVANCED_FACE ( 'NONE', ( #57172 ), #5795, .T. ) ;
#38859 = DIRECTION ( 'NONE',  ( 0.000000000000000000, 0.000000000000000000, 1.000000000000000000 ) ) ;
#38860 = DIRECTION ( 'NONE',  ( 0.000000000000000000, -0.9999939076577903929, 0.003490651415223739937 ) ) ;
#38862 = EDGE_CURVE ( 'NONE', #28471, #86078, #26747, .T. ) ;
#38861 = AXIS2_PLACEMENT_3D ( 'NONE', #52182, #92759, #69892 ) ;
#38863 = CARTESIAN_POINT ( 'NONE',  ( 2.299999999999948752, 12.50000000000000000, 0.3464101615137735735 ) ) ;
#38864 = DIRECTION ( 'NONE',  ( 0.000000000000000000, 0.000000000000000000, 1.000000000000000000 ) ) ;
#38865 = CARTESIAN_POINT ( 'NONE',  ( -8.749999999999975131, 2.500000000000000000, -2.265063509461101798 ) ) ;
#38866 = CARTESIAN_POINT ( 'NONE',  ( -9.600000000000006750, 12.50000000000000000, 5.022947341949748790 ) ) ;
#38867 = FACE_OUTER_BOUND ( 'NONE', #23849, .T. ) ;
#38869 = EDGE_CURVE ( 'NONE', #63695, #98092, #64306, .T. ) ;
#38868 = CARTESIAN_POINT ( 'NONE',  ( -10.40000000000000213, 2.500000000000000000, -2.276824562219559311E-15 ) ) ;
#38870 = AXIS2_PLACEMENT_3D ( 'NONE', #23171, #12066, #12694 ) ;
#38871 = ORIENTED_EDGE ( 'NONE', *, *, #108437, .T. ) ;
#38872 = VERTEX_POINT ( 'NONE', #105642 ) ;
#38873 = VECTOR ( 'NONE', #63629, 1000.000000000000000 ) ;
#38874 = ORIENTED_EDGE ( 'NONE', *, *, #77695, .T. ) ;
#38875 = ORIENTED_EDGE ( 'NONE', *, *, #1946, .T. ) ;
#38876 = FACE_OUTER_BOUND ( 'NONE', #126713, .T. ) ;
#38877 = CARTESIAN_POINT ( 'NONE',  ( -16.50000000000000000, 1.500000000000000000, 1.734723475976807094E-15 ) ) ;
#38879 = ORIENTED_EDGE ( 'NONE', *, *, #52274, .F. ) ;
#38878 = ORIENTED_EDGE ( 'NONE', *, *, #128717, .T. ) ;
#38880 = EDGE_LOOP ( 'NONE', ( #52776, #21406 ) ) ;
#38881 = ADVANCED_FACE ( 'NONE', ( #17889 ), #6752, .T. ) ;
#38882 = DIRECTION ( 'NONE',  ( -0.000000000000000000, 1.000000000000000000, -0.000000000000000000 ) ) ;
#38883 = DIRECTION ( 'NONE',  ( 0.000000000000000000, 1.000000000000000000, 0.000000000000000000 ) ) ;
#38884 = DIRECTION ( 'NONE',  ( 0.000000000000000000, 0.000000000000000000, -1.000000000000000000 ) ) ;
#38885 = LINE ( 'NONE', #127242, #31242 ) ;
#38886 = CARTESIAN_POINT ( 'NONE',  ( 3.549999999999941203, 2.500000000000000000, 6.148780366869520897 ) ) ;
#38887 = DIRECTION ( 'NONE',  ( -0.000000000000000000, 1.000000000000000000, -0.000000000000000000 ) ) ;
#38888 = DIRECTION ( 'NONE',  ( -0.000000000000000000, -1.000000000000000000, -0.000000000000000000 ) ) ;
#38889 = ADVANCED_FACE ( 'NONE', ( #65040 ), #53852, .T. ) ;
#38890 = ORIENTED_EDGE ( 'NONE', *, *, #86315, .T. ) ;
#38891 = FACE_OUTER_BOUND ( 'NONE', #11544, .T. ) ;
#38892 = VERTEX_POINT ( 'NONE', #25778 ) ;
#38894 = ORIENTED_EDGE ( 'NONE', *, *, #1629, .F. ) ;
#38893 = AXIS2_PLACEMENT_3D ( 'NONE', #126569, #118024, #36905 ) ;
#38895 = ORIENTED_EDGE ( 'NONE', *, *, #44711, .T. ) ;
#38896 = CONICAL_SURFACE ( 'NONE', #7451, 0.1000000000000002554, 0.003490658503988666988 ) ;
#38897 = DIRECTION ( 'NONE',  ( -0.000000000000000000, 1.000000000000000000, -0.000000000000000000 ) ) ;
#38898 = ORIENTED_EDGE ( 'NONE', *, *, #117678, .F. ) ;
#38899 = EDGE_LOOP ( 'NONE', ( #100620, #2973 ) ) ;
#38900 = DIRECTION ( 'NONE',  ( -0.000000000000000000, -1.000000000000000000, -0.000000000000000000 ) ) ;
#38901 = DIRECTION ( 'NONE',  ( 0.000000000000000000, 1.000000000000000000, 0.000000000000000000 ) ) ;
#38902 = DIRECTION ( 'NONE',  ( 0.000000000000000000, 1.000000000000000000, 0.000000000000000000 ) ) ;
#38903 = EDGE_CURVE ( 'NONE', #102323, #33917, #15942, .T. ) ;
#38904 = CARTESIAN_POINT ( 'NONE',  ( 11.64999999999990798, 2.500000000000000000, 7.188010851410848723 ) ) ;
#38905 = LINE ( 'NONE', #61591, #108278 ) ;
#38906 = ORIENTED_EDGE ( 'NONE', *, *, #98847, .T. ) ;
#38907 = DIRECTION ( 'NONE',  ( 0.000000000000000000, 0.000000000000000000, 1.000000000000000000 ) ) ;
#38908 = CIRCLE ( 'NONE', #118284, 0.1000000000000002554 ) ;
#38909 = AXIS2_PLACEMENT_3D ( 'NONE', #84546, #75358, #95655 ) ;
#38910 = EDGE_LOOP ( 'NONE', ( #73720, #58796, #122240, #123581 ) ) ;
#38911 = CARTESIAN_POINT ( 'NONE',  ( -3.550000000000027356, 12.50000000000000000, 1.883746621131358934 ) ) ;
#38912 = CIRCLE ( 'NONE', #57761, 0.1000000000000000472 ) ;
#38913 = EDGE_LOOP ( 'NONE', ( #80861, #60261, #59649, #5505 ) ) ;
#38914 = CARTESIAN_POINT ( 'NONE',  ( 112.8328331032861485, 8.604841203010149542, -1.324313734004374910 ) ) ;
#38915 = DIRECTION ( 'NONE',  ( 0.000000000000000000, 0.000000000000000000, 1.000000000000000000 ) ) ;
#38916 = AXIS2_PLACEMENT_3D ( 'NONE', #115036, #95417, #84942 ) ;
#38917 = ORIENTED_EDGE ( 'NONE', *, *, #126681, .F. ) ;
#38918 = DIRECTION ( 'NONE',  ( 0.000000000000000000, 1.000000000000000000, 0.000000000000000000 ) ) ;
#38919 = EDGE_CURVE ( 'NONE', #54886, #54702, #89444, .T. ) ;
#38920 = DIRECTION ( 'NONE',  ( 1.000000000000000000, -0.000000000000000000, 1.224646799147353207E-16 ) ) ;
#38921 = VERTEX_POINT ( 'NONE', #120612 ) ;
#38922 = CARTESIAN_POINT ( 'NONE',  ( 5.649999999999934630, 12.50000000000000000, 6.148780366869520897 ) ) ;
#38923 = ORIENTED_EDGE ( 'NONE', *, *, #46268, .F. ) ;
#38925 = ORIENTED_EDGE ( 'NONE', *, *, #61544, .T. ) ;
#38924 = ADVANCED_FACE ( 'NONE', ( #11292 ), #124948, .T. ) ;
#38926 = DIRECTION ( 'NONE',  ( 1.000000000000000000, 0.000000000000000000, 0.000000000000000000 ) ) ;
#38927 = DIRECTION ( 'NONE',  ( -0.000000000000000000, -1.000000000000000000, -0.000000000000000000 ) ) ;
#38928 = CARTESIAN_POINT ( 'NONE',  ( 5.399999999999934630, 2.500000000000000000, 0.5928203230275495006 ) ) ;
#38929 = AXIS2_PLACEMENT_3D ( 'NONE', #42549, #111914, #92257 ) ;
#38930 = CARTESIAN_POINT ( 'NONE',  ( 1.849999999999949019, 2.500000000000000000, 6.841600689897072485 ) ) ;
#38931 = DIRECTION ( 'NONE',  ( 0.000000000000000000, 0.000000000000000000, 1.000000000000000000 ) ) ;
#38932 = VERTEX_POINT ( 'NONE', #58490 ) ;
#38933 = CARTESIAN_POINT ( 'NONE',  ( 184.2395833340161460, 4.445597072760201662, 7.699999999999855405 ) ) ;
#38934 = AXIS2_PLACEMENT_3D ( 'NONE', #64741, #123032, #104655 ) ;
#38935 = AXIS2_PLACEMENT_3D ( 'NONE', #42700, #93073, #123785 ) ;
#38936 = ORIENTED_EDGE ( 'NONE', *, *, #7723, .F. ) ;
#38937 = CONICAL_SURFACE ( 'NONE', #3391, 0.1000000000000000472, 0.003490658503988666988 ) ;
#38938 = DIRECTION ( 'NONE',  ( -0.000000000000000000, -1.000000000000000000, -0.000000000000000000 ) ) ;
#38939 = DIRECTION ( 'NONE',  ( -0.000000000000000000, -1.000000000000000000, -0.000000000000000000 ) ) ;
#38940 = VECTOR ( 'NONE', #72616, 1000.000000000000000 ) ;
#38941 = EDGE_CURVE ( 'NONE', #25583, #118034, #110147, .T. ) ;
#38942 = ORIENTED_EDGE ( 'NONE', *, *, #73817, .T. ) ;
#38943 = DIRECTION ( 'NONE',  ( -0.000000000000000000, 1.000000000000000000, -0.000000000000000000 ) ) ;
#38944 = DIRECTION ( 'NONE',  ( -4.274815082592931898E-19, -0.9999939076577903929, -0.003490651415223739937 ) ) ;
#38945 = CARTESIAN_POINT ( 'NONE',  ( 3.749999999999940492, 2.500000000000000000, 5.902370205355745192 ) ) ;
#38946 = DIRECTION ( 'NONE',  ( 0.000000000000000000, 1.000000000000000000, 0.000000000000000000 ) ) ;
#38947 = DIRECTION ( 'NONE',  ( 0.000000000000000000, 0.000000000000000000, 1.000000000000000000 ) ) ;
#38948 = VERTEX_POINT ( 'NONE', #100333 ) ;
#38949 = AXIS2_PLACEMENT_3D ( 'NONE', #52305, #2538, #111203 ) ;
#38950 = EDGE_CURVE ( 'NONE', #11046, #102186, #47597, .T. ) ;
#38951 = LINE ( 'NONE', #78862, #2004 ) ;
#38952 = CIRCLE ( 'NONE', #70226, 0.1000000000000000472 ) ;
#38953 = DIRECTION ( 'NONE',  ( 0.000000000000000000, 0.000000000000000000, 1.000000000000000000 ) ) ;
#38954 = DIRECTION ( 'NONE',  ( 0.000000000000000000, 1.000000000000000000, 0.000000000000000000 ) ) ;
#38955 = EDGE_CURVE ( 'NONE', #128693, #66202, #68506, .T. ) ;
#38956 = ADVANCED_FACE ( 'NONE', ( #79410 ), #30961, .T. ) ;
#38957 = EDGE_CURVE ( 'NONE', #82926, #3365, #28815, .T. ) ;
#38958 = EDGE_CURVE ( 'NONE', #87862, #83631, #60222, .T. ) ;
#38959 = ORIENTED_EDGE ( 'NONE', *, *, #7139, .F. ) ;
#38960 = PLANE ( 'NONE',  #17606 ) ;
#38961 = VERTEX_POINT ( 'NONE', #69568 ) ;
#38962 = VERTEX_POINT ( 'NONE', #18538 ) ;
#38963 = DIRECTION ( 'NONE',  ( -0.000000000000000000, -1.000000000000000000, -0.000000000000000000 ) ) ;
#38964 = EDGE_CURVE ( 'NONE', #101462, #35406, #89852, .T. ) ;
#38965 = ADVANCED_FACE ( 'NONE', ( #59122 ), #91499, .T. ) ;
#38966 = ORIENTED_EDGE ( 'NONE', *, *, #39800, .F. ) ;
#38967 = DIRECTION ( 'NONE',  ( 0.000000000000000000, 1.000000000000000000, 0.000000000000000000 ) ) ;
#38968 = FACE_OUTER_BOUND ( 'NONE', #11138, .T. ) ;
#38969 = EDGE_CURVE ( 'NONE', #102800, #17230, #78114, .T. ) ;
#38970 = VERTEX_POINT ( 'NONE', #59786 ) ;
#38971 = ADVANCED_FACE ( 'NONE', ( #833 ), #80700, .T. ) ;
#38973 = ADVANCED_FACE ( 'NONE', ( #49319 ), #55976, .T. ) ;
#38972 = DIRECTION ( 'NONE',  ( 0.000000000000000000, 0.000000000000000000, 1.000000000000000000 ) ) ;
#38975 = ORIENTED_EDGE ( 'NONE', *, *, #49029, .F. ) ;
#38974 = DIRECTION ( 'NONE',  ( 0.000000000000000000, 0.000000000000000000, 1.000000000000000000 ) ) ;
#38976 = DIRECTION ( 'NONE',  ( 0.000000000000000000, 0.000000000000000000, -1.000000000000000000 ) ) ;
#38977 = DIRECTION ( 'NONE',  ( 0.000000000000000000, 0.000000000000000000, 1.000000000000000000 ) ) ;
#38978 = ADVANCED_FACE ( 'NONE', ( #28373 ), #129190, .T. ) ;
#38979 = VERTEX_POINT ( 'NONE', #78773 ) ;
#38980 = VECTOR ( 'NONE', #112090, 1000.000000000000000 ) ;
#38981 = ORIENTED_EDGE ( 'NONE', *, *, #10316, .F. ) ;
#38982 = CIRCLE ( 'NONE', #120427, 0.06509327318403745899 ) ;
#38983 = ORIENTED_EDGE ( 'NONE', *, *, #59551, .T. ) ;
#38984 = LINE ( 'NONE', #69038, #33707 ) ;
#38985 = DIRECTION ( 'NONE',  ( 0.000000000000000000, 0.000000000000000000, 1.000000000000000000 ) ) ;
#38986 = CARTESIAN_POINT ( 'NONE',  ( 0.1999999999999571565, 12.50000000000000000, 3.983716857408420076 ) ) ;
#38987 = FACE_BOUND ( 'NONE', #29458, .T. ) ;
#38988 = ORIENTED_EDGE ( 'NONE', *, *, #10516, .T. ) ;
#38989 = FACE_OUTER_BOUND ( 'NONE', #24062, .T. ) ;
#38990 = DIRECTION ( 'NONE',  ( -0.000000000000000000, 1.000000000000000000, -0.000000000000000000 ) ) ;
#38991 = ORIENTED_EDGE ( 'NONE', *, *, #122452, .T. ) ;
#38992 = CIRCLE ( 'NONE', #47285, 0.09999999999999982514 ) ;
#38993 = CARTESIAN_POINT ( 'NONE',  ( -11.64999999999999858, 2.500000000000000000, -1.572243186433546214 ) ) ;
#38994 = CARTESIAN_POINT ( 'NONE',  ( 129.5000000000000000, -0.6250000000000028866, -7.634788798650553154 ) ) ;
#38995 = DIRECTION ( 'NONE',  ( 0.000000000000000000, 0.000000000000000000, 1.000000000000000000 ) ) ;
#38996 = CARTESIAN_POINT ( 'NONE',  ( -10.65000000000000213, 12.50000000000000000, 1.753560074763284016 ) ) ;
#38997 = DIRECTION ( 'NONE',  ( 0.000000000000000000, 0.000000000000000000, 1.000000000000000000 ) ) ;
#38998 = PLANE ( 'NONE',  #116076 ) ;
#38999 = DIRECTION ( 'NONE',  ( 0.000000000000000000, 0.000000000000000000, -1.000000000000000000 ) ) ;
#39000 = AXIS2_PLACEMENT_3D ( 'NONE', #23774, #63698, #34250 ) ;
#39001 = VECTOR ( 'NONE', #64768, 1000.000000000000000 ) ;
#39002 = EDGE_LOOP ( 'NONE', ( #75294, #30840 ) ) ;
#39003 = ORIENTED_EDGE ( 'NONE', *, *, #45302, .F. ) ;
#39004 = VERTEX_POINT ( 'NONE', #118667 ) ;
#39005 = EDGE_LOOP ( 'NONE', ( #75942, #35704, #129331, #10435 ) ) ;
#39006 = EDGE_LOOP ( 'NONE', ( #69383, #98482, #121285, #77705 ) ) ;
#39007 = DIRECTION ( 'NONE',  ( 0.000000000000000000, 0.000000000000000000, -1.000000000000000000 ) ) ;
#39008 = FACE_OUTER_BOUND ( 'NONE', #33451, .T. ) ;
#39009 = EDGE_LOOP ( 'NONE', ( #93156, #127207, #121217, #88054 ) ) ;
#39010 = FACE_BOUND ( 'NONE', #27301, .T. ) ;
#39011 = DIRECTION ( 'NONE',  ( 0.000000000000000000, 1.000000000000000000, 0.000000000000000000 ) ) ;
#39012 = ADVANCED_FACE ( 'NONE', ( #30319 ), #29023, .T. ) ;
#39013 = CARTESIAN_POINT ( 'NONE',  ( -4.550000000000022915, 2.500000000000000000, 2.065063509461097624 ) ) ;
#39014 = EDGE_CURVE ( 'NONE', #71566, #108669, #58064, .T. ) ;
#39015 = DIRECTION ( 'NONE',  ( 0.000000000000000000, 0.000000000000000000, 1.000000000000000000 ) ) ;
#39016 = CARTESIAN_POINT ( 'NONE',  ( -15.59999999999998010, 2.500000000000000000, 0.2464101615137759549 ) ) ;
#39017 = DIRECTION ( 'NONE',  ( 0.000000000000000000, 1.000000000000000000, 0.000000000000000000 ) ) ;
#39019 = ORIENTED_EDGE ( 'NONE', *, *, #108512, .F. ) ;
#39018 = AXIS2_PLACEMENT_3D ( 'NONE', #120296, #98695, #30637 ) ;
#39020 = EDGE_CURVE ( 'NONE', #94819, #69257, #114475, .T. ) ;
#39021 = VERTEX_POINT ( 'NONE', #102888 ) ;
#39022 = VECTOR ( 'NONE', #48769, 1000.000000000000000 ) ;
#39023 = ORIENTED_EDGE ( 'NONE', *, *, #114548, .T. ) ;
#39024 = ORIENTED_EDGE ( 'NONE', *, *, #129566, .T. ) ;
#39025 = CARTESIAN_POINT ( 'NONE',  ( 8.549999999999918998, 2.500000000000000000, -1.918653347947326004 ) ) ;
#39026 = CARTESIAN_POINT ( 'NONE',  ( -5.650000000000023448, 12.50000000000000000, -6.083687093685488989 ) ) ;
#39027 = CARTESIAN_POINT ( 'NONE',  ( 10.84999999999991260, 2.500000000000000000, 7.188010851410848723 ) ) ;
#39028 = ORIENTED_EDGE ( 'NONE', *, *, #123164, .F. ) ;
#39029 = CARTESIAN_POINT ( 'NONE',  ( 4.149999999999939959, 12.50000000000000000, 1.407149913249508000 ) ) ;
#39030 = CONICAL_SURFACE ( 'NONE', #61989, 0.09999999999999982514, 0.003490658503988666988 ) ;
#39031 = VECTOR ( 'NONE', #32233, 1000.000000000000000 ) ;
#39032 = CARTESIAN_POINT ( 'NONE',  ( -7.300000000000016698, 2.500000000000000000, -4.576537180435978236 ) ) ;
#39033 = AXIS2_PLACEMENT_3D ( 'NONE', #3863, #83087, #94177 ) ;
#39034 = DIRECTION ( 'NONE',  ( 0.000000000000000000, 0.000000000000000000, 1.000000000000000000 ) ) ;
#39035 = CARTESIAN_POINT ( 'NONE',  ( 184.6927083336747160, 6.551208109652275624, -3.782341765624998686 ) ) ;
#39036 = LINE ( 'NONE', #38377, #4838 ) ;
#39037 = CARTESIAN_POINT ( 'NONE',  ( 1.249999999999988454, 2.500000000000000000, -2.265063509461101798 ) ) ;
#39038 = CARTESIAN_POINT ( 'NONE',  ( 9.349999999999919709, 12.50000000000000000, -6.841600689897078702 ) ) ;
#39039 = VERTEX_POINT ( 'NONE', #102267 ) ;
#39040 = DIRECTION ( 'NONE',  ( 0.000000000000000000, 0.000000000000000000, 1.000000000000000000 ) ) ;
#39041 = AXIS2_PLACEMENT_3D ( 'NONE', #68884, #106241, #16546 ) ;
#39042 = ORIENTED_EDGE ( 'NONE', *, *, #123411, .T. ) ;
#39043 = AXIS2_PLACEMENT_3D ( 'NONE', #15794, #55091, #55728 ) ;
#39044 = ORIENTED_EDGE ( 'NONE', *, *, #127638, .F. ) ;
#39045 = DIRECTION ( 'NONE',  ( 0.000000000000000000, 1.000000000000000000, 0.000000000000000000 ) ) ;
#39046 = DIRECTION ( 'NONE',  ( 0.000000000000000000, 0.000000000000000000, 1.000000000000000000 ) ) ;
#39047 = DIRECTION ( 'NONE',  ( -4.274815082592931898E-19, -0.9999939076577903929, -0.003490651415223739937 ) ) ;
#39048 = ORIENTED_EDGE ( 'NONE', *, *, #107208, .T. ) ;
#39049 = ORIENTED_EDGE ( 'NONE', *, *, #5381, .F. ) ;
#39050 = EDGE_CURVE ( 'NONE', #46879, #109098, #37225, .T. ) ;
#39051 = FACE_OUTER_BOUND ( 'NONE', #86164, .T. ) ;
#39052 = DIRECTION ( 'NONE',  ( 0.000000000000000000, 0.000000000000000000, -1.000000000000000000 ) ) ;
#39053 = DIRECTION ( 'NONE',  ( 0.000000000000000000, 0.000000000000000000, -1.000000000000000000 ) ) ;
#39054 = ORIENTED_EDGE ( 'NONE', *, *, #35571, .F. ) ;
#39055 = DIRECTION ( 'NONE',  ( 0.000000000000000000, 1.000000000000000000, 0.000000000000000000 ) ) ;
#39056 = ORIENTED_EDGE ( 'NONE', *, *, #77146, .F. ) ;
#39057 = DIRECTION ( 'NONE',  ( 0.000000000000000000, 0.000000000000000000, -1.000000000000000000 ) ) ;
#39058 = ORIENTED_EDGE ( 'NONE', *, *, #11476, .T. ) ;
#39059 = DIRECTION ( 'NONE',  ( 0.000000000000000000, 0.000000000000000000, -1.000000000000000000 ) ) ;
#39060 = FACE_OUTER_BOUND ( 'NONE', #71018, .T. ) ;
#39061 = DIRECTION ( 'NONE',  ( 0.000000000000000000, 0.000000000000000000, 1.000000000000000000 ) ) ;
#39062 = ADVANCED_FACE ( 'NONE', ( #31592 ), #70569, .T. ) ;
#39063 = EDGE_CURVE ( 'NONE', #37898, #86156, #30882, .T. ) ;
#39064 = FACE_OUTER_BOUND ( 'NONE', #33690, .T. ) ;
#39065 = ORIENTED_EDGE ( 'NONE', *, *, #70663, .T. ) ;
#39066 = CARTESIAN_POINT ( 'NONE',  ( -9.150000000000005684, 12.50000000000000000, 6.495190528383297135 ) ) ;
#39067 = AXIS2_PLACEMENT_3D ( 'NONE', #51730, #81187, #35 ) ;
#39068 = AXIS2_PLACEMENT_3D ( 'NONE', #37310, #126970, #27453 ) ;
#39069 = ORIENTED_EDGE ( 'NONE', *, *, #26593, .F. ) ;
#39070 = ORIENTED_EDGE ( 'NONE', *, *, #113997, .F. ) ;
#39071 = ADVANCED_FACE ( 'NONE', ( #51881 ), #45354, .T. ) ;
#39072 = FACE_OUTER_BOUND ( 'NONE', #76505, .T. ) ;
#39073 = CARTESIAN_POINT ( 'NONE',  ( 3.749999999999942268, 2.500000000000000000, -1.472243186433550122 ) ) ;
#39074 = CARTESIAN_POINT ( 'NONE',  ( -6.900000000000019007, 2.500000000000000000, -4.576537180435978236 ) ) ;
#39075 = DIRECTION ( 'NONE',  ( 0.000000000000000000, 0.000000000000000000, -1.000000000000000000 ) ) ;
#39076 = CARTESIAN_POINT ( 'NONE',  ( 3.349999999999943689, 12.50000000000000000, 2.165063509461097713 ) ) ;
#39078 = CONICAL_SURFACE ( 'NONE', #51581, 0.1000000000000002554, 0.003490658503988666988 ) ;
#39077 = FACE_OUTER_BOUND ( 'NONE', #13167, .T. ) ;
#39079 = DIRECTION ( 'NONE',  ( 0.000000000000000000, 0.000000000000000000, 1.000000000000000000 ) ) ;
#39080 = FACE_OUTER_BOUND ( 'NONE', #51825, .T. ) ;
#39081 = PLANE ( 'NONE',  #46343 ) ;
#39082 = AXIS2_PLACEMENT_3D ( 'NONE', #19015, #28866, #86477 ) ;
#39083 = CONICAL_SURFACE ( 'NONE', #112222, 0.1000000000000002554, 0.003490658503988666988 ) ;
#39084 = AXIS2_PLACEMENT_3D ( 'NONE', #126558, #27689, #77447 ) ;
#39085 = ORIENTED_EDGE ( 'NONE', *, *, #83136, .F. ) ;
#39086 = CARTESIAN_POINT ( 'NONE',  ( -2.900000000000030109, 12.50000000000000000, 0.6928203230275494784 ) ) ;
#39087 = CARTESIAN_POINT ( 'NONE',  ( 8.749999999999957367, 12.50000000000000000, -6.430097255199264339 ) ) ;
#39088 = CARTESIAN_POINT ( 'NONE',  ( 11.44999999999990692, 2.500000000000000000, -6.741600689897078169 ) ) ;
#39089 = FACE_OUTER_BOUND ( 'NONE', #107756, .T. ) ;
#39090 = DIRECTION ( 'NONE',  ( -0.000000000000000000, -1.000000000000000000, -0.000000000000000000 ) ) ;
#39091 = VERTEX_POINT ( 'NONE', #81340 ) ;
#39092 = CARTESIAN_POINT ( 'NONE',  ( -3.950000000000024603, 12.50000000000000000, -2.511473670974877948 ) ) ;
#39093 = EDGE_CURVE ( 'NONE', #120916, #95574, #11871, .T. ) ;
#39094 = DIRECTION ( 'NONE',  ( 0.000000000000000000, 0.000000000000000000, 1.000000000000000000 ) ) ;
#39096 = EDGE_LOOP ( 'NONE', ( #47477, #96853 ) ) ;
#39095 = DIRECTION ( 'NONE',  ( 0.000000000000000000, 0.000000000000000000, -1.000000000000000000 ) ) ;
#39097 = EDGE_CURVE ( 'NONE', #82797, #54150, #93097, .T. ) ;
#39098 = AXIS2_PLACEMENT_3D ( 'NONE', #40300, #67134, #39034 ) ;
#39099 = AXIS2_PLACEMENT_3D ( 'NONE', #19681, #79883, #129018 ) ;
#39100 = ADVANCED_FACE ( 'NONE', ( #11937 ), #118482, .T. ) ;
#39101 = EDGE_LOOP ( 'NONE', ( #86976, #106788, #94077, #96714 ) ) ;
#39102 = VECTOR ( 'NONE', #57009, 1000.000000000000000 ) ;
#39103 = DIRECTION ( 'NONE',  ( 0.000000000000000000, -0.000000000000000000, 1.000000000000000000 ) ) ;
#39104 = AXIS2_PLACEMENT_3D ( 'NONE', #16540, #46040, #74201 ) ;
#39105 = ORIENTED_EDGE ( 'NONE', *, *, #58717, .F. ) ;
#39106 = ORIENTED_EDGE ( 'NONE', *, *, #5483, .T. ) ;
#39107 = VERTEX_POINT ( 'NONE', #14502 ) ;
#39108 = DIRECTION ( 'NONE',  ( 0.000000000000000000, 0.000000000000000000, 1.000000000000000000 ) ) ;
#39109 = EDGE_CURVE ( 'NONE', #114232, #33730, #125034, .T. ) ;
#39110 = ADVANCED_FACE ( 'NONE', ( #91796 ), #2109, .T. ) ;
#39111 = EDGE_CURVE ( 'NONE', #120522, #54801, #56073, .T. ) ;
#39112 = AXIS2_PLACEMENT_3D ( 'NONE', #57986, #26587, #65854 ) ;
#39113 = CARTESIAN_POINT ( 'NONE',  ( -4.200000000000025935, 2.500000000000000000, -0.1000000000000023925 ) ) ;
#39114 = PLANE ( 'NONE',  #117290 ) ;
#39115 = AXIS2_PLACEMENT_3D ( 'NONE', #27360, #57492, #74064 ) ;
#39116 = DIRECTION ( 'NONE',  ( 0.000000000000000000, 0.000000000000000000, 1.000000000000000000 ) ) ;
#39117 = ORIENTED_EDGE ( 'NONE', *, *, #73935, .T. ) ;
#39118 = CIRCLE ( 'NONE', #5615, 0.06509327318403745899 ) ;
#39119 = ADVANCED_FACE ( 'NONE', ( #121256 ), #71503, .T. ) ;
#39120 = DIRECTION ( 'NONE',  ( 0.000000000000000000, 0.000000000000000000, 1.000000000000000000 ) ) ;
#39121 = EDGE_LOOP ( 'NONE', ( #7748, #110547 ) ) ;
#39122 = CARTESIAN_POINT ( 'NONE',  ( -6.450000000000014388, 12.50000000000000000, 6.148780366869520897 ) ) ;
#39123 = CARTESIAN_POINT ( 'NONE',  ( 18.87984495337378732, -0.5408627091910553908, -4.542689527610523470 ) ) ;
#39124 = CARTESIAN_POINT ( 'NONE',  ( -1.650000000000034772, 2.500000000000000000, 2.265063509461097357 ) ) ;
#39125 = FACE_OUTER_BOUND ( 'NONE', #1083, .T. ) ;
#39126 = AXIS2_PLACEMENT_3D ( 'NONE', #96150, #26774, #66046 ) ;
#39127 = CARTESIAN_POINT ( 'NONE',  ( 5.399999999999934630, 12.50000000000000000, 0.6277270498435120194 ) ) ;
#39128 = EDGE_CURVE ( 'NONE', #114933, #98804, #87368, .T. ) ;
#39129 = AXIS2_PLACEMENT_3D ( 'NONE', #119929, #79369, #29607 ) ;
#39130 = ORIENTED_EDGE ( 'NONE', *, *, #127740, .F. ) ;
#39132 = CIRCLE ( 'NONE', #20234, 0.06509327318403745899 ) ;
#39131 = CIRCLE ( 'NONE', #18159, 0.1000000000000000472 ) ;
#39133 = EDGE_LOOP ( 'NONE', ( #22837, #71185, #109986, #8557 ) ) ;
#39134 = ORIENTED_EDGE ( 'NONE', *, *, #47537, .F. ) ;
#39135 = VERTEX_POINT ( 'NONE', #103560 ) ;
#39136 = ORIENTED_EDGE ( 'NONE', *, *, #108084, .F. ) ;
#39137 = DIRECTION ( 'NONE',  ( 0.000000000000000000, -0.9999939076577903929, 0.003490651415223739937 ) ) ;
#39138 = DIRECTION ( 'NONE',  ( -4.274815082592931898E-19, -0.9999939076577903929, -0.003490651415223739937 ) ) ;
#39139 = FACE_OUTER_BOUND ( 'NONE', #15164, .T. ) ;
#39140 = FACE_BOUND ( 'NONE', #110795, .T. ) ;
#39141 = CARTESIAN_POINT ( 'NONE',  ( 8.949999999999921130, 2.500000000000000000, -6.941600689897078347 ) ) ;
#39142 = CARTESIAN_POINT ( 'NONE',  ( 186.2395833340161460, 4.445597072760117285, 7.699999999999999289 ) ) ;
#39143 = FACE_OUTER_BOUND ( 'NONE', #45136, .T. ) ;
#39144 = DIRECTION ( 'NONE',  ( 0.000000000000000000, 1.000000000000000000, 0.000000000000000000 ) ) ;
#39145 = DIRECTION ( 'NONE',  ( -0.000000000000000000, 1.000000000000000000, -0.000000000000000000 ) ) ;
#39146 = CARTESIAN_POINT ( 'NONE',  ( 6.249999999999967137, 12.50000000000000000, 6.495190528383297135 ) ) ;
#39147 = VECTOR ( 'NONE', #126747, 1000.000000000000000 ) ;
#39148 = CARTESIAN_POINT ( 'NONE',  ( 11.24999999999994493, 2.500000000000000000, 6.495190528383297135 ) ) ;
#39149 = CARTESIAN_POINT ( 'NONE',  ( 9.399999999999918643, 12.50000000000000000, -0.2813168883297408329 ) ) ;
#39150 = ORIENTED_EDGE ( 'NONE', *, *, #79699, .T. ) ;
#39151 = ORIENTED_EDGE ( 'NONE', *, *, #12716, .F. ) ;
#39152 = ORIENTED_EDGE ( 'NONE', *, *, #62035, .T. ) ;
#39153 = ORIENTED_EDGE ( 'NONE', *, *, #98910, .T. ) ;
#39154 = DIRECTION ( 'NONE',  ( 0.000000000000000000, 1.000000000000000000, 0.000000000000000000 ) ) ;
#39155 = DIRECTION ( 'NONE',  ( -4.274815082592931898E-19, -0.9999939076577903929, -0.003490651415223739937 ) ) ;
#39156 = FACE_BOUND ( 'NONE', #65462, .T. ) ;
#39157 = DIRECTION ( 'NONE',  ( 0.000000000000000000, 0.000000000000000000, 1.000000000000000000 ) ) ;
#39158 = ADVANCED_FACE ( 'NONE', ( #81967 ), #91591, .T. ) ;
#39159 = CIRCLE ( 'NONE', #41211, 0.06509327318403745899 ) ;
#39160 = EDGE_LOOP ( 'NONE', ( #109608, #125160 ) ) ;
#39161 = CARTESIAN_POINT ( 'NONE',  ( -6.050000000000022027, 12.50000000000000000, -6.083687093685488989 ) ) ;
#39162 = DIRECTION ( 'NONE',  ( -0.000000000000000000, 1.000000000000000000, -0.000000000000000000 ) ) ;
#39163 = DIRECTION ( 'NONE',  ( 0.000000000000000000, 1.000000000000000000, 0.000000000000000000 ) ) ;
#39164 = DIRECTION ( 'NONE',  ( -0.000000000000000000, 1.000000000000000000, -0.000000000000000000 ) ) ;
#39165 = DIRECTION ( 'NONE',  ( 0.000000000000000000, 0.000000000000000000, 1.000000000000000000 ) ) ;
#39166 = EDGE_LOOP ( 'NONE', ( #15779, #1858, #109249, #70119 ) ) ;
#39167 = CARTESIAN_POINT ( 'NONE',  ( 6.649999999999931966, 12.50000000000000000, -7.253104124594891289 ) ) ;
#39168 = AXIS2_PLACEMENT_3D ( 'NONE', #119710, #90239, #37939 ) ;
#39169 = EDGE_CURVE ( 'NONE', #77956, #33245, #112086, .T. ) ;
#39170 = VERTEX_POINT ( 'NONE', #123815 ) ;
#39171 = ORIENTED_EDGE ( 'NONE', *, *, #9630, .T. ) ;
#39172 = DIRECTION ( 'NONE',  ( 0.000000000000000000, -0.000000000000000000, 1.000000000000000000 ) ) ;
#39173 = CARTESIAN_POINT ( 'NONE',  ( -3.750000000000025757, 2.500000000000000000, -2.757883832488654097 ) ) ;
#39174 = ORIENTED_EDGE ( 'NONE', *, *, #40725, .F. ) ;
#39176 = VECTOR ( 'NONE', #73887, 1000.000000000000000 ) ;
#39175 = CONICAL_SURFACE ( 'NONE', #58033, 0.1000000000000002554, 0.003490658503988666988 ) ;
#39177 = VECTOR ( 'NONE', #59107, 1000.000000000000000 ) ;
#39178 = CARTESIAN_POINT ( 'NONE',  ( -10.60000000000000320, 2.500000000000000000, -4.776537180435973085 ) ) ;
#39179 = FACE_OUTER_BOUND ( 'NONE', #33780, .T. ) ;
#39180 = VERTEX_POINT ( 'NONE', #34175 ) ;
#39181 = DIRECTION ( 'NONE',  ( 0.000000000000000000, 1.000000000000000000, 0.000000000000000000 ) ) ;
#39182 = EDGE_LOOP ( 'NONE', ( #69972, #58147 ) ) ;
#39183 = DIRECTION ( 'NONE',  ( -4.274815082592931898E-19, -0.9999939076577903929, -0.003490651415223739937 ) ) ;
#39184 = ORIENTED_EDGE ( 'NONE', *, *, #123105, .F. ) ;
#39185 = CARTESIAN_POINT ( 'NONE',  ( -14.14999999999998614, 2.500000000000000000, -2.165063509461099489 ) ) ;
#39186 = FACE_BOUND ( 'NONE', #107876, .T. ) ;
#39187 = VECTOR ( 'NONE', #31117, 1000.000000000000000 ) ;
#39188 = ORIENTED_EDGE ( 'NONE', *, *, #49773, .F. ) ;
#39189 = DIRECTION ( 'NONE',  ( 0.000000000000000000, 0.000000000000000000, -1.000000000000000000 ) ) ;
#39190 = EDGE_LOOP ( 'NONE', ( #10229, #102180 ) ) ;
#39191 = CARTESIAN_POINT ( 'NONE',  ( 0.7999999999999612976, 2.500000000000000000, -0.1000000000000001166 ) ) ;
#39192 = LINE ( 'NONE', #37869, #80087 ) ;
#39193 = CARTESIAN_POINT ( 'NONE',  ( 9.149999999999920419, 2.500000000000000000, 2.857883832488649301 ) ) ;
#39194 = PLANE ( 'NONE',  #13166 ) ;
#39196 = AXIS2_PLACEMENT_3D ( 'NONE', #12420, #51088, #41908 ) ;
#39195 = CARTESIAN_POINT ( 'NONE',  ( -4.250072516143177381E-14, 2.500000000000000000, -3.537306695894649966 ) ) ;
#39197 = ORIENTED_EDGE ( 'NONE', *, *, #54307, .F. ) ;
#39198 = CONICAL_SURFACE ( 'NONE', #5705, 0.09999999999999982514, 0.003490658503988666988 ) ;
#39199 = ORIENTED_EDGE ( 'NONE', *, *, #58006, .T. ) ;
#39201 = VERTEX_POINT ( 'NONE', #5335 ) ;
#39200 = EDGE_CURVE ( 'NONE', #103444, #96136, #44630, .T. ) ;
#39202 = DIRECTION ( 'NONE',  ( -0.000000000000000000, -1.000000000000000000, -0.000000000000000000 ) ) ;
#39203 = CIRCLE ( 'NONE', #37130, 0.06509327318403745899 ) ;
#39204 = CARTESIAN_POINT ( 'NONE',  ( -1.650000000000034772, 2.500000000000000000, 6.495190528383297135 ) ) ;
#39205 = CARTESIAN_POINT ( 'NONE',  ( 129.5000000000000000, -1.375000000000000000, 7.576237522675751457 ) ) ;
#39207 = ORIENTED_EDGE ( 'NONE', *, *, #118387, .F. ) ;
#39206 = VERTEX_POINT ( 'NONE', #55732 ) ;
#39208 = ORIENTED_EDGE ( 'NONE', *, *, #74520, .T. ) ;
#39209 = DIRECTION ( 'NONE',  ( 0.000000000000000000, 0.000000000000000000, 1.000000000000000000 ) ) ;
#39210 = CIRCLE ( 'NONE', #43404, 0.06509327318403745899 ) ;
#39211 = AXIS2_PLACEMENT_3D ( 'NONE', #43033, #72473, #63935 ) ;
#39213 = EDGE_CURVE ( 'NONE', #16894, #102223, #46546, .T. ) ;
#39212 = CARTESIAN_POINT ( 'NONE',  ( 195.0000000000000000, 0.000000000000000000, 0.000000000000000000 ) ) ;
#39214 = AXIS2_PLACEMENT_3D ( 'NONE', #83823, #75296, #22992 ) ;
#39215 = APPLICATION_PROTOCOL_DEFINITION ( 'draft international standard', 'automotive_design', 1998, #114080 ) ;
#39216 = LINE ( 'NONE', #79751, #63640 ) ;
#39217 = LINE ( 'NONE', #120328, #4316 ) ;
#39218 = CARTESIAN_POINT ( 'NONE',  ( -5.800000000000018474, 12.50000000000000000, 4.330127018922196314 ) ) ;
#39219 = DIRECTION ( 'NONE',  ( -0.000000000000000000, 1.000000000000000000, -0.000000000000000000 ) ) ;
#39220 = CARTESIAN_POINT ( 'NONE',  ( -10.65000000000000213, 2.500000000000000000, 2.511473670974873507 ) ) ;
#39221 = ADVANCED_FACE ( 'NONE', ( #17058 ), #85325, .T. ) ;
#39222 = AXIS2_PLACEMENT_3D ( 'NONE', #81667, #32606, #22775 ) ;
#39223 = EDGE_CURVE ( 'NONE', #4340, #48111, #102061, .T. ) ;
#39224 = DIRECTION ( 'NONE',  ( -4.274815082592931898E-19, -0.9999939076577903929, -0.003490651415223739937 ) ) ;
#39225 = VERTEX_POINT ( 'NONE', #76018 ) ;
#39226 = ORIENTED_EDGE ( 'NONE', *, *, #98224, .T. ) ;
#39227 = DIRECTION ( 'NONE',  ( -0.000000000000000000, -1.000000000000000000, -0.000000000000000000 ) ) ;
#39229 = CIRCLE ( 'NONE', #112353, 0.1000000000000000472 ) ;
#39228 = AXIS2_PLACEMENT_3D ( 'NONE', #99084, #38901, #38233 ) ;
#39230 = EDGE_CURVE ( 'NONE', #114770, #128977, #64396, .T. ) ;
#39231 = CARTESIAN_POINT ( 'NONE',  ( 165.4999999999999716, 0.000000000000000000, -2.000000000000000000 ) ) ;
#39232 = ORIENTED_EDGE ( 'NONE', *, *, #24573, .T. ) ;
#39233 = VERTEX_POINT ( 'NONE', #115265 ) ;
#39234 = ADVANCED_FACE ( 'NONE', ( #106125 ), #22653, .T. ) ;
#39235 = CARTESIAN_POINT ( 'NONE',  ( 186.6093750003414016, 9.264065473108010111E-16, -7.564683531250000925 ) ) ;
#39236 = CARTESIAN_POINT ( 'NONE',  ( -1.850000000000033396, 12.50000000000000000, -6.213873640053564351 ) ) ;
#39237 = CARTESIAN_POINT ( 'NONE',  ( 12.89999999999990266, 2.500000000000000000, -4.922947341949753586 ) ) ;
#39238 = CARTESIAN_POINT ( 'NONE',  ( 13.09999999999990195, 12.50000000000000000, 4.611443907251934426 ) ) ;
#39239 = DIRECTION ( 'NONE',  ( -0.000000000000000000, 1.000000000000000000, -0.000000000000000000 ) ) ;
#39240 = DIRECTION ( 'NONE',  ( 0.000000000000000000, -0.9999939076577903929, 0.003490651415223739937 ) ) ;
#39241 = DIRECTION ( 'NONE',  ( -0.000000000000000000, 1.000000000000000000, -0.000000000000000000 ) ) ;
#39242 = CONICAL_SURFACE ( 'NONE', #103964, 0.1000000000000002554, 0.003490658503988666988 ) ;
#39243 = CARTESIAN_POINT ( 'NONE',  ( 7.049999999999928768, 12.50000000000000000, -2.230156782645139391 ) ) ;
#39244 = ORIENTED_EDGE ( 'NONE', *, *, #7266, .F. ) ;
#39245 = EDGE_CURVE ( 'NONE', #83964, #118566, #81137, .T. ) ;
#39246 = VERTEX_POINT ( 'NONE', #57007 ) ;
#39247 = ORIENTED_EDGE ( 'NONE', *, *, #69082, .F. ) ;
#39248 = ORIENTED_EDGE ( 'NONE', *, *, #108929, .T. ) ;
#39249 = DIRECTION ( 'NONE',  ( 0.000000000000000000, 0.000000000000000000, 1.000000000000000000 ) ) ;
#39250 = DIRECTION ( 'NONE',  ( 0.000000000000000000, 1.000000000000000000, 0.000000000000000000 ) ) ;
#39251 = VERTEX_POINT ( 'NONE', #85825 ) ;
#39252 = VECTOR ( 'NONE', #200, 1000.000000000000000 ) ;
#39253 = DIRECTION ( 'NONE',  ( 0.000000000000000000, 1.000000000000000000, 0.000000000000000000 ) ) ;
#39254 = EDGE_CURVE ( 'NONE', #40453, #21310, #78809, .T. ) ;
#39256 = CARTESIAN_POINT ( 'NONE',  ( 8.949999999999919353, 12.50000000000000000, -6.148780366869526226 ) ) ;
#39255 = AXIS2_PLACEMENT_3D ( 'NONE', #84638, #55820, #124571 ) ;
#39257 = CARTESIAN_POINT ( 'NONE',  ( 8.749999999999953815, 2.500000000000000000, -2.065063509461102065 ) ) ;
#39259 = EDGE_LOOP ( 'NONE', ( #66108, #82113 ) ) ;
#39258 = LINE ( 'NONE', #78532, #53804 ) ;
#39260 = CARTESIAN_POINT ( 'NONE',  ( 11.24999999999990941, 12.50000000000000000, 7.122917578226811486 ) ) ;
#39262 = EDGE_CURVE ( 'NONE', #104716, #71809, #112243, .T. ) ;
#39261 = CIRCLE ( 'NONE', #37190, 0.1000000000000002554 ) ;
#39263 = DIRECTION ( 'NONE',  ( 0.000000000000000000, -0.000000000000000000, 1.000000000000000000 ) ) ;
#39264 = EDGE_LOOP ( 'NONE', ( #71280, #43727 ) ) ;
#39265 = AXIS2_PLACEMENT_3D ( 'NONE', #103583, #96312, #85213 ) ;
#39266 = AXIS2_PLACEMENT_3D ( 'NONE', #78557, #89007, #18950 ) ;
#39267 = ORIENTED_EDGE ( 'NONE', *, *, #87473, .T. ) ;
#39268 = ORIENTED_EDGE ( 'NONE', *, *, #30790, .T. ) ;
#39269 = ORIENTED_EDGE ( 'NONE', *, *, #63436, .T. ) ;
#39270 = CARTESIAN_POINT ( 'NONE',  ( 9.599999999999914380, 2.500000000000000000, -3.737306695894649700 ) ) ;
#39271 = ADVANCED_FACE ( 'NONE', ( #55095 ), #108305, .T. ) ;
#39272 = EDGE_CURVE ( 'NONE', #83854, #63832, #14211, .T. ) ;
#39273 = EDGE_CURVE ( 'NONE', #2826, #55428, #39394, .T. ) ;
#39274 = CARTESIAN_POINT ( 'NONE',  ( -8.350000000000013856, 12.50000000000000000, -5.867463478539781896 ) ) ;
#39275 = FACE_OUTER_BOUND ( 'NONE', #38767, .T. ) ;
#39276 = VECTOR ( 'NONE', #66174, 1000.000000000000000 ) ;
#39277 = EDGE_CURVE ( 'NONE', #65565, #74025, #74736, .T. ) ;
#39278 = VERTEX_POINT ( 'NONE', #116577 ) ;
#39279 = CONICAL_SURFACE ( 'NONE', #74941, 0.1000000000000002554, 0.003490658503988666988 ) ;
#39280 = DIRECTION ( 'NONE',  ( 0.000000000000000000, 0.000000000000000000, 1.000000000000000000 ) ) ;
#39281 = DIRECTION ( 'NONE',  ( 0.000000000000000000, 1.000000000000000000, 0.000000000000000000 ) ) ;
#39282 = CARTESIAN_POINT ( 'NONE',  ( 3.749999999999942268, 12.50000000000000000, 1.472243186433545459 ) ) ;
#39283 = DIRECTION ( 'NONE',  ( 0.000000000000000000, -0.9999939076577903929, 0.003490651415223739937 ) ) ;
#39284 = EDGE_CURVE ( 'NONE', #5464, #93629, #95514, .T. ) ;
#39285 = EDGE_CURVE ( 'NONE', #37787, #112012, #91306, .T. ) ;
#39286 = ORIENTED_EDGE ( 'NONE', *, *, #113132, .F. ) ;
#39287 = AXIS2_PLACEMENT_3D ( 'NONE', #125546, #16852, #56157 ) ;
#39288 = ADVANCED_FACE ( 'NONE', ( #117197 ), #124756, .T. ) ;
#39289 = CARTESIAN_POINT ( 'NONE',  ( 1.649999999999951505, 2.500000000000000000, -2.957883832488653830 ) ) ;
#39290 = CONICAL_SURFACE ( 'NONE', #26644, 0.1000000000000000472, 0.003490658503988666988 ) ;
#39291 = ORIENTED_EDGE ( 'NONE', *, *, #5681, .F. ) ;
#39292 = VERTEX_POINT ( 'NONE', #85193 ) ;
#39293 = CARTESIAN_POINT ( 'NONE',  ( 8.749999999999953815, 2.500000000000000000, 6.495190528383297135 ) ) ;
#39294 = CARTESIAN_POINT ( 'NONE',  ( 8.099999999999921485, 2.500000000000000000, 0.3464101615137735735 ) ) ;
#39295 = FACE_BOUND ( 'NONE', #11858, .T. ) ;
#39296 = VECTOR ( 'NONE', #61387, 1000.000000000000000 ) ;
#39297 = CARTESIAN_POINT ( 'NONE',  ( -5.850000000000022737, 12.50000000000000000, -2.165063509461101710 ) ) ;
#39298 = DIRECTION ( 'NONE',  ( 0.000000000000000000, 0.000000000000000000, 1.000000000000000000 ) ) ;
#39299 = AXIS2_PLACEMENT_3D ( 'NONE', #91018, #41287, #94230 ) ;
#39300 = CARTESIAN_POINT ( 'NONE',  ( 13.94999999999989448, 12.50000000000000000, -2.511473670974877948 ) ) ;
#39301 = ORIENTED_EDGE ( 'NONE', *, *, #36899, .F. ) ;
#39302 = CARTESIAN_POINT ( 'NONE',  ( -6.450000000000014388, 2.500000000000000000, 1.918653347947321564 ) ) ;
#39303 = DIRECTION ( 'NONE',  ( 0.000000000000000000, 0.000000000000000000, -1.000000000000000000 ) ) ;
#39305 = CARTESIAN_POINT ( 'NONE',  ( 0.7999999999999553024, 12.50000000000000000, -4.395220292106239768 ) ) ;
#39304 = CIRCLE ( 'NONE', #66445, 0.09999999999999982514 ) ;
#39306 = DIRECTION ( 'NONE',  ( -0.000000000000000000, 1.000000000000000000, -0.000000000000000000 ) ) ;
#39307 = ORIENTED_EDGE ( 'NONE', *, *, #108221, .F. ) ;
#39308 = LINE ( 'NONE', #118467, #78374 ) ;
#39309 = AXIS2_PLACEMENT_3D ( 'NONE', #122647, #32995, #23810 ) ;
#39310 = FACE_OUTER_BOUND ( 'NONE', #36586, .T. ) ;
#39311 = ORIENTED_EDGE ( 'NONE', *, *, #5565, .F. ) ;
#39312 = VERTEX_POINT ( 'NONE', #35464 ) ;
#39313 = CARTESIAN_POINT ( 'NONE',  ( -5.850000000000021849, 2.500000000000000000, -1.572243186433550211 ) ) ;
#39314 = CONICAL_SURFACE ( 'NONE', #101983, 0.1000000000000002554, 0.003490658503988666988 ) ;
#39315 = DIRECTION ( 'NONE',  ( 0.000000000000000000, 0.000000000000000000, 1.000000000000000000 ) ) ;
#39316 = FACE_BOUND ( 'NONE', #69853, .T. ) ;
#39317 = DIRECTION ( 'NONE',  ( 0.000000000000000000, 0.000000000000000000, 1.000000000000000000 ) ) ;
#39319 = AXIS2_PLACEMENT_3D ( 'NONE', #116036, #86568, #47953 ) ;
#39318 = AXIS2_PLACEMENT_3D ( 'NONE', #85858, #84593, #96323 ) ;
#39320 = CARTESIAN_POINT ( 'NONE',  ( 12.89999999999990088, 2.500000000000000000, 4.330127018922196314 ) ) ;
#39321 = ORIENTED_EDGE ( 'NONE', *, *, #129357, .T. ) ;
#39322 = DIRECTION ( 'NONE',  ( -4.274815082592931898E-19, -0.9999939076577903929, -0.003490651415223739937 ) ) ;
#39323 = CARTESIAN_POINT ( 'NONE',  ( 184.5833333333333144, -6.668395609140180369, 3.849999999999994760 ) ) ;
#39324 = EDGE_LOOP ( 'NONE', ( #12637, #68582, #70641, #117750 ) ) ;
#39325 = CARTESIAN_POINT ( 'NONE',  ( -0.6000000000000323963, 2.500000000000000000, 0.3464101615137759604 ) ) ;
#39326 = DIRECTION ( 'NONE',  ( -0.000000000000000000, -1.000000000000000000, -0.000000000000000000 ) ) ;
#39327 = ADVANCED_FACE ( 'NONE', ( #75362 ), #25615, .F. ) ;
#39328 = DIRECTION ( 'NONE',  ( 0.000000000000000000, 0.000000000000000000, 1.000000000000000000 ) ) ;
#39329 = CARTESIAN_POINT ( 'NONE',  ( -6.450000000000017941, 2.500000000000000000, -2.411473670974877859 ) ) ;
#39330 = ORIENTED_EDGE ( 'NONE', *, *, #86694, .F. ) ;
#39331 = DIRECTION ( 'NONE',  ( -0.000000000000000000, 1.000000000000000000, -0.000000000000000000 ) ) ;
#39332 = CARTESIAN_POINT ( 'NONE',  ( 184.6979166673494603, 6.668395609140176816, 3.850000000000000977 ) ) ;
#39333 = CARTESIAN_POINT ( 'NONE',  ( 3.299999999999944755, 2.500000000000000000, -4.230127018922201998 ) ) ;
#39334 = ORIENTED_EDGE ( 'NONE', *, *, #71830, .T. ) ;
#39335 = VECTOR ( 'NONE', #10329, 1000.000000000000000 ) ;
#39336 = EDGE_LOOP ( 'NONE', ( #69360, #127861 ) ) ;
#39337 = CARTESIAN_POINT ( 'NONE',  ( 17.99892160975036859, 2.500000000000000444, 4.934975027008750459 ) ) ;
#39338 = ORIENTED_EDGE ( 'NONE', *, *, #63545, .F. ) ;
#39339 = CARTESIAN_POINT ( 'NONE',  ( 10.79999999999991367, 2.500000000000000000, -2.385244779468109755E-15 ) ) ;
#39340 = CARTESIAN_POINT ( 'NONE',  ( 2.899999999999944844, 12.50000000000000000, 5.022947341949748790 ) ) ;
#39341 = AXIS2_PLACEMENT_3D ( 'NONE', #28891, #17758, #57706 ) ;
#39342 = LINE ( 'NONE', #31284, #43072 ) ;
#39343 = CIRCLE ( 'NONE', #91548, 0.06509327318403745899 ) ;
#39344 = CARTESIAN_POINT ( 'NONE',  ( 9.999999999999911182, 2.500000000000000000, 4.922947341949748257 ) ) ;
#39345 = ORIENTED_EDGE ( 'NONE', *, *, #58572, .T. ) ;
#39346 = DIRECTION ( 'NONE',  ( -0.000000000000000000, 1.000000000000000000, -0.000000000000000000 ) ) ;
#39347 = DIRECTION ( 'NONE',  ( 0.000000000000000000, 0.000000000000000000, 1.000000000000000000 ) ) ;
#39348 = LINE ( 'NONE', #8545, #77832 ) ;
#39349 = CARTESIAN_POINT ( 'NONE',  ( 185.4843750003414016, -8.734944146203032389, -1.604583208406767949E-15 ) ) ;
#39350 = DIRECTION ( 'NONE',  ( -1.000000000000000000, -0.000000000000000000, -0.000000000000000000 ) ) ;
#39351 = LINE ( 'NONE', #56375, #70255 ) ;
#39352 = AXIS2_PLACEMENT_3D ( 'NONE', #75559, #97789, #67017 ) ;
#39353 = ORIENTED_EDGE ( 'NONE', *, *, #1700, .T. ) ;
#39355 = ORIENTED_EDGE ( 'NONE', *, *, #98930, .F. ) ;
#39354 = AXIS2_PLACEMENT_3D ( 'NONE', #11724, #52302, #11065 ) ;
#39356 = DIRECTION ( 'NONE',  ( -0.000000000000000000, 1.000000000000000000, -0.000000000000000000 ) ) ;
#39357 = VERTEX_POINT ( 'NONE', #119163 ) ;
#39358 = CARTESIAN_POINT ( 'NONE',  ( 7.299999999999926104, 2.500000000000000000, 4.576537180435972019 ) ) ;
#39360 = VERTEX_POINT ( 'NONE', #77947 ) ;
#39359 = ORIENTED_EDGE ( 'NONE', *, *, #125053, .T. ) ;
#39361 = ORIENTED_EDGE ( 'NONE', *, *, #7266, .T. ) ;
#39362 = CARTESIAN_POINT ( 'NONE',  ( -12.04999999999999716, 12.50000000000000000, -6.495190528383298911 ) ) ;
#39365 = EDGE_CURVE ( 'NONE', #74009, #50259, #22369, .T. ) ;
#39364 = FACE_OUTER_BOUND ( 'NONE', #112594, .T. ) ;
#39363 = CIRCLE ( 'NONE', #10090, 0.1000000000000002554 ) ;
#39366 = CARTESIAN_POINT ( 'NONE',  ( -3.150000000000033218, 12.50000000000000000, -6.906693963081115939 ) ) ;
#39367 = PLANE ( 'NONE',  #82807 ) ;
#39368 = FACE_OUTER_BOUND ( 'NONE', #99552, .T. ) ;
#39369 = CARTESIAN_POINT ( 'NONE',  ( 2.949999999999946887, 2.500000000000000000, -2.265063509461101798 ) ) ;
#39370 = CONICAL_SURFACE ( 'NONE', #20562, 0.1000000000000002554, 0.003490658503988666988 ) ;
#39371 = FACE_OUTER_BOUND ( 'NONE', #92871, .T. ) ;
#39372 = EDGE_CURVE ( 'NONE', #77356, #20308, #20326, .T. ) ;
#39373 = EDGE_CURVE ( 'NONE', #8757, #50689, #97837, .T. ) ;
#39374 = DIRECTION ( 'NONE',  ( -0.000000000000000000, 1.000000000000000000, -0.000000000000000000 ) ) ;
#39375 = ORIENTED_EDGE ( 'NONE', *, *, #99731, .F. ) ;
#39376 = CIRCLE ( 'NONE', #12233, 0.06509327318403745899 ) ;
#39377 = ORIENTED_EDGE ( 'NONE', *, *, #7076, .T. ) ;
#39378 = PRESENTATION_LAYER_ASSIGNMENT (  '', '', ( #33110 ) ) ;
#39379 = EDGE_CURVE ( 'NONE', #60176, #31905, #41445, .T. ) ;
#39381 = EDGE_CURVE ( 'NONE', #109510, #44029, #58157, .T. ) ;
#39380 = CARTESIAN_POINT ( 'NONE',  ( 6.849999999999929479, 2.500000000000000000, 6.048780366869520364 ) ) ;
#39382 = ORIENTED_EDGE ( 'NONE', *, *, #70730, .F. ) ;
#39383 = ORIENTED_EDGE ( 'NONE', *, *, #60253, .T. ) ;
#39384 = EDGE_CURVE ( 'NONE', #90957, #24019, #49554, .T. ) ;
#39385 = DIRECTION ( 'NONE',  ( 0.000000000000000000, 0.000000000000000000, 1.000000000000000000 ) ) ;
#39386 = AXIS2_PLACEMENT_3D ( 'NONE', #36929, #67654, #96461 ) ;
#39387 = AXIS2_PLACEMENT_3D ( 'NONE', #37262, #71061, #1661 ) ;
#39389 = CONICAL_SURFACE ( 'NONE', #95789, 0.1000000000000002554, 0.003490658503988666988 ) ;
#39388 = CARTESIAN_POINT ( 'NONE',  ( 11.84999999999990372, 12.50000000000000000, -6.841600689897078702 ) ) ;
#39390 = DIRECTION ( 'NONE',  ( 0.000000000000000000, 1.000000000000000000, 0.000000000000000000 ) ) ;
#39391 = LINE ( 'NONE', #30205, #117983 ) ;
#39392 = FACE_OUTER_BOUND ( 'NONE', #9639, .T. ) ;
#39393 = VERTEX_POINT ( 'NONE', #120454 ) ;
#39394 = CIRCLE ( 'NONE', #112533, 0.1000000000000002554 ) ;
#39395 = ORIENTED_EDGE ( 'NONE', *, *, #34481, .F. ) ;
#39396 = CARTESIAN_POINT ( 'NONE',  ( 7.299999999999926104, 2.500000000000000000, -3.983716857408426293 ) ) ;
#39397 = ORIENTED_EDGE ( 'NONE', *, *, #39097, .T. ) ;
#39398 = DIRECTION ( 'NONE',  ( 0.000000000000000000, 0.000000000000000000, 1.000000000000000000 ) ) ;
#39399 = ORIENTED_EDGE ( 'NONE', *, *, #59804, .T. ) ;
#39400 = AXIS2_PLACEMENT_3D ( 'NONE', #48963, #108505, #76486 ) ;
#39401 = ORIENTED_EDGE ( 'NONE', *, *, #64829, .F. ) ;
#39402 = FACE_OUTER_BOUND ( 'NONE', #46947, .T. ) ;
#39403 = DIRECTION ( 'NONE',  ( 0.000000000000000000, 1.000000000000000000, 0.000000000000000000 ) ) ;
#39405 = AXIS2_PLACEMENT_3D ( 'NONE', #98315, #9304, #29587 ) ;
#39404 = AXIS2_PLACEMENT_3D ( 'NONE', #77989, #77348, #111133 ) ;
#39406 = CARTESIAN_POINT ( 'NONE',  ( 8.099999999999921485, 2.500000000000000000, -0.3464101615137783474 ) ) ;
#39407 = FACE_OUTER_BOUND ( 'NONE', #43856, .T. ) ;
#39408 = DIRECTION ( 'NONE',  ( -0.000000000000000000, -1.000000000000000000, -0.000000000000000000 ) ) ;
#39409 = VERTEX_POINT ( 'NONE', #59629 ) ;
#39410 = DIRECTION ( 'NONE',  ( 0.000000000000000000, -0.000000000000000000, 1.000000000000000000 ) ) ;
#39411 = LINE ( 'NONE', #79327, #103809 ) ;
#39412 = DIRECTION ( 'NONE',  ( -0.000000000000000000, -1.000000000000000000, -0.000000000000000000 ) ) ;
#39413 = DIRECTION ( 'NONE',  ( 0.000000000000000000, 0.000000000000000000, -1.000000000000000000 ) ) ;
#39414 = DIRECTION ( 'NONE',  ( -0.000000000000000000, -1.000000000000000000, -0.000000000000000000 ) ) ;
#39415 = VERTEX_POINT ( 'NONE', #60274 ) ;
#39416 = ORIENTED_EDGE ( 'NONE', *, *, #13023, .T. ) ;
#39417 = ADVANCED_FACE ( 'NONE', ( #69407 ), #11972, .T. ) ;
#39418 = AXIS2_PLACEMENT_3D ( 'NONE', #41392, #50535, #19807 ) ;
#39419 = CARTESIAN_POINT ( 'NONE',  ( -10.00000000000000711, 2.500000000000000000, -3.637306695894645614 ) ) ;
#39420 = EDGE_CURVE ( 'NONE', #80133, #104306, #50420, .T. ) ;
#39421 = EDGE_CURVE ( 'NONE', #76087, #126646, #99539, .T. ) ;
#39422 = ORIENTED_EDGE ( 'NONE', *, *, #85776, .T. ) ;
#39423 = FACE_OUTER_BOUND ( 'NONE', #122819, .T. ) ;
#39424 = CARTESIAN_POINT ( 'NONE',  ( 4.199999999999941558, 12.50000000000000000, -4.330127018922201643 ) ) ;
#39425 = AXIS2_PLACEMENT_3D ( 'NONE', #60950, #10549, #50490 ) ;
#39426 = CIRCLE ( 'NONE', #62398, 0.1000000000000002554 ) ;
#39427 = CIRCLE ( 'NONE', #56109, 0.06509327318403745899 ) ;
#39428 = EDGE_CURVE ( 'NONE', #98725, #63253, #89703, .T. ) ;
#39429 = EDGE_LOOP ( 'NONE', ( #44876, #78237 ) ) ;
#39430 = CARTESIAN_POINT ( 'NONE',  ( -8.150000000000012790, 2.500000000000000000, 1.718653347947321386 ) ) ;
#39431 = LINE ( 'NONE', #32185, #118494 ) ;
#39432 = EDGE_CURVE ( 'NONE', #32314, #40954, #28714, .T. ) ;
#39433 = DIRECTION ( 'NONE',  ( 0.000000000000000000, 1.000000000000000000, 0.000000000000000000 ) ) ;
#39434 = DIRECTION ( 'NONE',  ( 0.000000000000000000, 1.000000000000000000, 0.000000000000000000 ) ) ;
#39435 = EDGE_LOOP ( 'NONE', ( #73611, #83852, #113308, #19327 ) ) ;
#39436 = EDGE_CURVE ( 'NONE', #60183, #122361, #30779, .T. ) ;
#39437 = EDGE_CURVE ( 'NONE', #79801, #105776, #87757, .T. ) ;
#39438 = AXIS2_PLACEMENT_3D ( 'NONE', #3132, #82345, #102602 ) ;
#39439 = EDGE_CURVE ( 'NONE', #60348, #4520, #118513, .T. ) ;
#39440 = CARTESIAN_POINT ( 'NONE',  ( 3.099999999999945022, 2.500000000000000000, -0.2464101615137783419 ) ) ;
#39441 = ORIENTED_EDGE ( 'NONE', *, *, #126703, .T. ) ;
#39442 = CARTESIAN_POINT ( 'NONE',  ( 48.84099803997424516, 2.320797884491624163, -5.300800515398695012 ) ) ;
#39443 = DIRECTION ( 'NONE',  ( 0.000000000000000000, 1.000000000000000000, 0.000000000000000000 ) ) ;
#39444 = ADVANCED_FACE ( 'NONE', ( #20963 ), #129085, .T. ) ;
#39445 = AXIS2_PLACEMENT_3D ( 'NONE', #105262, #15579, #125541 ) ;
#39446 = DIRECTION ( 'NONE',  ( 0.000000000000000000, -0.9999939076577903929, 0.003490651415223739937 ) ) ;
#39447 = AXIS2_PLACEMENT_3D ( 'NONE', #84457, #34735, #66092 ) ;
#39448 = ORIENTED_EDGE ( 'NONE', *, *, #11430, .F. ) ;
#39449 = LINE ( 'NONE', #113147, #99141 ) ;
#39450 = ORIENTED_EDGE ( 'NONE', *, *, #115091, .F. ) ;
#39451 = DIRECTION ( 'NONE',  ( -0.000000000000000000, -1.000000000000000000, -0.000000000000000000 ) ) ;
#39452 = DIRECTION ( 'NONE',  ( -0.000000000000000000, 1.000000000000000000, -0.000000000000000000 ) ) ;
#39453 = PLANE ( 'NONE',  #102045 ) ;
#39454 = ORIENTED_EDGE ( 'NONE', *, *, #53008, .T. ) ;
#39455 = AXIS2_PLACEMENT_3D ( 'NONE', #32581, #106288, #16602 ) ;
#39456 = DIRECTION ( 'NONE',  ( 0.000000000000000000, -0.000000000000000000, 1.000000000000000000 ) ) ;
#39457 = DIRECTION ( 'NONE',  ( -0.000000000000000000, 1.000000000000000000, -0.000000000000000000 ) ) ;
#39458 = AXIS2_PLACEMENT_3D ( 'NONE', #98375, #128530, #59787 ) ;
#39459 = VECTOR ( 'NONE', #116317, 1000.000000000000000 ) ;
#39460 = ORIENTED_EDGE ( 'NONE', *, *, #74509, .F. ) ;
#39461 = DIRECTION ( 'NONE',  ( 0.000000000000000000, 1.000000000000000000, 0.000000000000000000 ) ) ;
#39462 = ORIENTED_EDGE ( 'NONE', *, *, #82965, .T. ) ;
#39463 = DIRECTION ( 'NONE',  ( -0.000000000000000000, -1.000000000000000000, -0.000000000000000000 ) ) ;
#39464 = CIRCLE ( 'NONE', #56146, 0.06509327318403743123 ) ;
#39465 = ORIENTED_EDGE ( 'NONE', *, *, #19389, .F. ) ;
#39466 = DIRECTION ( 'NONE',  ( 0.000000000000000000, 0.000000000000000000, 1.000000000000000000 ) ) ;
#39467 = CARTESIAN_POINT ( 'NONE',  ( 13.39473262249372176, 2.500000000000001332, -7.044698190877980437 ) ) ;
#39468 = ORIENTED_EDGE ( 'NONE', *, *, #35024, .T. ) ;
#39469 = EDGE_LOOP ( 'NONE', ( #60884, #6818, #107456, #112254 ) ) ;
#39470 = FACE_OUTER_BOUND ( 'NONE', #48032, .T. ) ;
#39471 = DIRECTION ( 'NONE',  ( 0.000000000000000000, 0.000000000000000000, 1.000000000000000000 ) ) ;
#39472 = ORIENTED_EDGE ( 'NONE', *, *, #2360, .T. ) ;
#39473 = CARTESIAN_POINT ( 'NONE',  ( 185.6666666666666856, -6.668395609140176816, -3.850000000000003642 ) ) ;
#39474 = CARTESIAN_POINT ( 'NONE',  ( 186.6093750003414016, 9.264065473108010111E-16, -7.564683531250000925 ) ) ;
#39475 = CIRCLE ( 'NONE', #79177, 0.06509327318403745899 ) ;
#39476 = EDGE_CURVE ( 'NONE', #106311, #25426, #74670, .T. ) ;
#39477 = DIRECTION ( 'NONE',  ( 0.000000000000000000, 0.000000000000000000, -1.000000000000000000 ) ) ;
#39478 = DIRECTION ( 'NONE',  ( 0.000000000000000000, 0.000000000000000000, 1.000000000000000000 ) ) ;
#39479 = CARTESIAN_POINT ( 'NONE',  ( 108.0000000000000142, 8.700999999999998735, 0.000000000000000000 ) ) ;
#39480 = DIRECTION ( 'NONE',  ( 0.000000000000000000, 0.000000000000000000, -1.000000000000000000 ) ) ;
#39481 = DIRECTION ( 'NONE',  ( -0.000000000000000000, 1.000000000000000000, -0.000000000000000000 ) ) ;
#39482 = AXIS2_PLACEMENT_3D ( 'NONE', #51874, #53162, #84544 ) ;
#39483 = VERTEX_POINT ( 'NONE', #58331 ) ;
#39484 = ORIENTED_EDGE ( 'NONE', *, *, #40082, .T. ) ;
#39486 = ORIENTED_EDGE ( 'NONE', *, *, #18579, .F. ) ;
#39485 = AXIS2_PLACEMENT_3D ( 'NONE', #74674, #3986, #104137 ) ;
#39487 = EDGE_LOOP ( 'NONE', ( #119936, #27384 ) ) ;
#39488 = DIRECTION ( 'NONE',  ( -0.000000000000000000, -1.000000000000000000, -0.000000000000000000 ) ) ;
#39489 = CARTESIAN_POINT ( 'NONE',  ( -5.600000000000020073, 2.500000000000000000, 0.4464101615137736623 ) ) ;
#39490 = DIRECTION ( 'NONE',  ( -0.000000000000000000, -1.000000000000000000, -0.000000000000000000 ) ) ;
#39491 = AXIS2_PLACEMENT_3D ( 'NONE', #107717, #75661, #107056 ) ;
#39492 = ORIENTED_EDGE ( 'NONE', *, *, #20354, .F. ) ;
#39493 = ADVANCED_FACE ( 'NONE', ( #58962 ), #16155, .T. ) ;
#39494 = FACE_BOUND ( 'NONE', #14072, .T. ) ;
#39495 = ORIENTED_EDGE ( 'NONE', *, *, #102895, .F. ) ;
#39496 = DIRECTION ( 'NONE',  ( 0.000000000000000000, 0.000000000000000000, 1.000000000000000000 ) ) ;
#39497 = DIRECTION ( 'NONE',  ( 0.000000000000000000, 1.000000000000000000, 0.000000000000000000 ) ) ;
#39498 = DIRECTION ( 'NONE',  ( 0.000000000000000000, 0.000000000000000000, 1.000000000000000000 ) ) ;
#39500 = AXIS2_PLACEMENT_3D ( 'NONE', #5736, #18147, #97358 ) ;
#39499 = VECTOR ( 'NONE', #75102, 1000.000000000000000 ) ;
#39501 = CARTESIAN_POINT ( 'NONE',  ( -9.150000000000009237, 12.50000000000000000, -2.857883832488653741 ) ) ;
#39502 = DIRECTION ( 'NONE',  ( -4.274815082592931898E-19, -0.9999939076577903929, -0.003490651415223739937 ) ) ;
#39503 = DIRECTION ( 'NONE',  ( 0.000000000000000000, 0.000000000000000000, 1.000000000000000000 ) ) ;
#39504 = DIRECTION ( 'NONE',  ( 0.000000000000000000, -0.9999939076577903929, 0.003490651415223739937 ) ) ;
#39505 = CARTESIAN_POINT ( 'NONE',  ( -6.450000000000016165, 12.50000000000000000, 6.906693963081109722 ) ) ;
#39506 = DIRECTION ( 'NONE',  ( 0.000000000000000000, -0.9999939076577903929, 0.003490651415223739937 ) ) ;
#39507 = CARTESIAN_POINT ( 'NONE',  ( -12.29999999999999716, 12.50000000000000000, -3.918623584224386391 ) ) ;
#39508 = ORIENTED_EDGE ( 'NONE', *, *, #104290, .F. ) ;
#39509 = ORIENTED_EDGE ( 'NONE', *, *, #49919, .T. ) ;
#39510 = ORIENTED_EDGE ( 'NONE', *, *, #118436, .F. ) ;
#39511 = VERTEX_POINT ( 'NONE', #49160 ) ;
#39512 = CARTESIAN_POINT ( 'NONE',  ( -14.34999999999998543, 2.500000000000000000, 2.611473670974877148 ) ) ;
#39513 = CIRCLE ( 'NONE', #106373, 0.1000000000000002554 ) ;
#39514 = LINE ( 'NONE', #116107, #29730 ) ;
#39516 = VERTEX_POINT ( 'NONE', #82478 ) ;
#39515 = VERTEX_POINT ( 'NONE', #89068 ) ;
#39517 = VERTEX_POINT ( 'NONE', #111249 ) ;
#39518 = CARTESIAN_POINT ( 'NONE',  ( 185.1666666666666856, -6.668395609140176816, -3.850000000000003642 ) ) ;
#39519 = AXIS2_PLACEMENT_3D ( 'NONE', #96199, #66104, #15041 ) ;
#39520 = EDGE_CURVE ( 'NONE', #59400, #84082, #101865, .T. ) ;
#39521 = VECTOR ( 'NONE', #68983, 1000.000000000000000 ) ;
#39522 = CARTESIAN_POINT ( 'NONE',  ( -10.40000000000000213, 12.50000000000000000, 0.6928203230275494784 ) ) ;
#39523 = DIRECTION ( 'NONE',  ( -4.274815082592931898E-19, -0.9999939076577903929, -0.003490651415223739937 ) ) ;
#39524 = DIRECTION ( 'NONE',  ( 0.000000000000000000, 1.000000000000000000, 0.000000000000000000 ) ) ;
#39525 = CARTESIAN_POINT ( 'NONE',  ( -12.69999999999999218, 2.500000000000000000, 4.676537180435972552 ) ) ;
#39526 = FACE_OUTER_BOUND ( 'NONE', #128010, .T. ) ;
#39527 = CARTESIAN_POINT ( 'NONE',  ( 5.849999999999933031, 12.50000000000000000, 7.188010851410848723 ) ) ;
#39528 = ORIENTED_EDGE ( 'NONE', *, *, #89731, .F. ) ;
#39529 = EDGE_CURVE ( 'NONE', #41594, #32478, #87180, .T. ) ;
#39530 = VECTOR ( 'NONE', #89287, 1000.000000000000000 ) ;
#39531 = CARTESIAN_POINT ( 'NONE',  ( 9.349999999999916156, 12.50000000000000000, -2.511473670974877948 ) ) ;
#39532 = EDGE_LOOP ( 'NONE', ( #45857, #104906, #91956, #2609 ) ) ;
#39533 = AXIS2_PLACEMENT_3D ( 'NONE', #49511, #89417, #128055 ) ;
#39534 = ORIENTED_EDGE ( 'NONE', *, *, #125477, .T. ) ;
#39535 = ORIENTED_EDGE ( 'NONE', *, *, #90200, .F. ) ;
#39536 = ADVANCED_FACE ( 'NONE', ( #62197 ), #76734, .T. ) ;
#39538 = EDGE_CURVE ( 'NONE', #96060, #36724, #37025, .T. ) ;
#39537 = DIRECTION ( 'NONE',  ( 0.000000000000000000, 1.000000000000000000, 0.000000000000000000 ) ) ;
#39540 = ORIENTED_EDGE ( 'NONE', *, *, #80486, .F. ) ;
#39539 = EDGE_CURVE ( 'NONE', #81272, #14213, #118577, .T. ) ;
#39541 = EDGE_CURVE ( 'NONE', #119696, #17553, #57956, .T. ) ;
#39543 = ORIENTED_EDGE ( 'NONE', *, *, #83850, .T. ) ;
#39542 = ADVANCED_FACE ( 'NONE', ( #42560 ), #41270, .T. ) ;
#39544 = CONICAL_SURFACE ( 'NONE', #83346, 0.1000000000000002554, 0.003490658503988666988 ) ;
#39545 = FACE_OUTER_BOUND ( 'NONE', #63736, .T. ) ;
#39546 = AXIS2_PLACEMENT_3D ( 'NONE', #50991, #12329, #100704 ) ;
#39547 = DIRECTION ( 'NONE',  ( 0.000000000000000000, 0.000000000000000000, -1.000000000000000000 ) ) ;
#39548 = CARTESIAN_POINT ( 'NONE',  ( -9.350000000000006750, 2.500000000000000000, 1.818653347947321475 ) ) ;
#39549 = DIRECTION ( 'NONE',  ( 0.000000000000000000, 0.000000000000000000, 1.000000000000000000 ) ) ;
#39550 = CARTESIAN_POINT ( 'NONE',  ( 13.29999999999990301, 2.500000000000000000, 4.330127018922196314 ) ) ;
#39551 = ADVANCED_FACE ( 'NONE', ( #121731 ), #80941, .T. ) ;
#39552 = VERTEX_POINT ( 'NONE', #71336 ) ;
#39553 = DIRECTION ( 'NONE',  ( 0.000000000000000000, 1.000000000000000000, 0.000000000000000000 ) ) ;
#39554 = AXIS2_PLACEMENT_3D ( 'NONE', #62022, #82311, #114811 ) ;
#39555 = ADVANCED_FACE ( 'NONE', ( #102107 ), #24502, .T. ) ;
#39556 = EDGE_LOOP ( 'NONE', ( #17391, #21512, #122231, #90324 ) ) ;
#39557 = CARTESIAN_POINT ( 'NONE',  ( -2.500000000000032863, 2.500000000000000000, 5.022947341949748790 ) ) ;
#39558 = ORIENTED_EDGE ( 'NONE', *, *, #52106, .T. ) ;
#39559 = CARTESIAN_POINT ( 'NONE',  ( 1.699999999999950218, 12.50000000000000000, 4.265033745738159077 ) ) ;
#39560 = LINE ( 'NONE', #107621, #47002 ) ;
#39561 = VERTEX_POINT ( 'NONE', #113862 ) ;
#39562 = FACE_OUTER_BOUND ( 'NONE', #40627, .T. ) ;
#39563 = LINE ( 'NONE', #10683, #54063 ) ;
#39564 = ORIENTED_EDGE ( 'NONE', *, *, #128051, .F. ) ;
#39565 = AXIS2_PLACEMENT_3D ( 'NONE', #40349, #48219, #28584 ) ;
#39566 = CARTESIAN_POINT ( 'NONE',  ( -7.300000000000018474, 2.500000000000000000, -3.983716857408426293 ) ) ;
#39567 = ORIENTED_EDGE ( 'NONE', *, *, #58572, .F. ) ;
#39568 = VERTEX_POINT ( 'NONE', #32093 ) ;
#39569 = CARTESIAN_POINT ( 'NONE',  ( -6.850000000000017408, 2.500000000000000000, -2.511473670974877948 ) ) ;
#39570 = CARTESIAN_POINT ( 'NONE',  ( 129.5000000000000000, 0.000000000000000000, 0.000000000000000000 ) ) ;
#39571 = DIRECTION ( 'NONE',  ( 0.000000000000000000, 0.000000000000000000, 1.000000000000000000 ) ) ;
#39573 = CONICAL_SURFACE ( 'NONE', #6066, 0.1000000000000002554, 0.003490658503988666988 ) ;
#39572 = DIRECTION ( 'NONE',  ( -4.274815082592931898E-19, -0.9999939076577903929, -0.003490651415223739937 ) ) ;
#39574 = AXIS2_PLACEMENT_3D ( 'NONE', #17337, #65806, #57292 ) ;
#39575 = CARTESIAN_POINT ( 'NONE',  ( 11.44999999999990692, 2.500000000000000000, -6.841600689897078702 ) ) ;
#39576 = ORIENTED_EDGE ( 'NONE', *, *, #9483, .T. ) ;
#39577 = CARTESIAN_POINT ( 'NONE',  ( 184.1562500006828031, 8.891194145520236347, 5.444286225454521982E-16 ) ) ;
#39578 = EDGE_CURVE ( 'NONE', #30658, #39552, #100793, .T. ) ;
#39579 = EDGE_LOOP ( 'NONE', ( #110721, #95209 ) ) ;
#39580 = DIRECTION ( 'NONE',  ( 0.000000000000000000, -0.9999939076577903929, 0.003490651415223739937 ) ) ;
#39581 = FACE_OUTER_BOUND ( 'NONE', #40481, .T. ) ;
#39582 = EDGE_CURVE ( 'NONE', #124473, #36694, #126911, .T. ) ;
#39583 = CIRCLE ( 'NONE', #125233, 0.1000000000000002554 ) ;
#39584 = AXIS2_PLACEMENT_3D ( 'NONE', #71022, #39011, #70369 ) ;
#39585 = DIRECTION ( 'NONE',  ( 0.000000000000000000, 0.000000000000000000, -1.000000000000000000 ) ) ;
#39586 = DIRECTION ( 'NONE',  ( -0.000000000000000000, -1.000000000000000000, -0.000000000000000000 ) ) ;
#39587 = CARTESIAN_POINT ( 'NONE',  ( -15.39999999999998082, 2.500000000000000000, 0.6928203230275518099 ) ) ;
#39588 = ADVANCED_FACE ( 'NONE', ( #22275 ), #64196, .T. ) ;
#39589 = DIRECTION ( 'NONE',  ( -1.000000000000000000, 0.000000000000000000, 0.000000000000000000 ) ) ;
#39590 = DIRECTION ( 'NONE',  ( -0.000000000000000000, -1.000000000000000000, -0.000000000000000000 ) ) ;
#39591 = ORIENTED_EDGE ( 'NONE', *, *, #23607, .T. ) ;
#39592 = ADVANCED_FACE ( 'NONE', ( #111927 ), #34989, .T. ) ;
#39594 = AXIS2_PLACEMENT_3D ( 'NONE', #98629, #129431, #51498 ) ;
#39593 = CIRCLE ( 'NONE', #118976, 0.1000000000000000472 ) ;
#39595 = CARTESIAN_POINT ( 'NONE',  ( -3.950000000000024603, 2.500000000000000000, 1.918653347947321564 ) ) ;
#39596 = EDGE_CURVE ( 'NONE', #16787, #127183, #108118, .T. ) ;
#39597 = FACE_OUTER_BOUND ( 'NONE', #101679, .T. ) ;
#39598 = ORIENTED_EDGE ( 'NONE', *, *, #78567, .F. ) ;
#39599 = EDGE_CURVE ( 'NONE', #48770, #98786, #52353, .T. ) ;
#39600 = DIRECTION ( 'NONE',  ( -0.000000000000000000, -1.000000000000000000, -0.000000000000000000 ) ) ;
#39601 = ORIENTED_EDGE ( 'NONE', *, *, #20934, .T. ) ;
#39602 = VERTEX_POINT ( 'NONE', #123653 ) ;
#39603 = DIRECTION ( 'NONE',  ( 0.000000000000000000, 1.000000000000000000, 0.000000000000000000 ) ) ;
#39604 = VERTEX_POINT ( 'NONE', #23531 ) ;
#39605 = CARTESIAN_POINT ( 'NONE',  ( 7.899999999999923084, 12.50000000000000000, 0.7579135962115869374 ) ) ;
#39606 = DIRECTION ( 'NONE',  ( 0.000000000000000000, 0.000000000000000000, 1.000000000000000000 ) ) ;
#39607 = ORIENTED_EDGE ( 'NONE', *, *, #117683, .T. ) ;
#39608 = CONICAL_SURFACE ( 'NONE', #20800, 0.09999999999999982514, 0.003490658503988666988 ) ;
#39609 = LINE ( 'NONE', #69682, #38397 ) ;
#39610 = AXIS2_PLACEMENT_3D ( 'NONE', #67343, #87650, #117745 ) ;
#39612 = EDGE_LOOP ( 'NONE', ( #75809, #40194 ) ) ;
#39611 = CARTESIAN_POINT ( 'NONE',  ( -8.150000000000014566, 2.500000000000000000, -6.941600689897073906 ) ) ;
#39613 = CARTESIAN_POINT ( 'NONE',  ( -3.350000000000028511, 12.50000000000000000, 1.472243186433545459 ) ) ;
#39614 = ADVANCED_FACE ( 'NONE', ( #83751 ), #120647, .T. ) ;
#39615 = AXIS2_PLACEMENT_3D ( 'NONE', #65618, #76736, #85263 ) ;
#39616 = ORIENTED_EDGE ( 'NONE', *, *, #67123, .F. ) ;
#39617 = CIRCLE ( 'NONE', #89761, 0.06509327318403745899 ) ;
#39618 = CIRCLE ( 'NONE', #64626, 0.06509327318403745899 ) ;
#39619 = EDGE_LOOP ( 'NONE', ( #120088, #53349, #63646, #99835 ) ) ;
#39620 = ORIENTED_EDGE ( 'NONE', *, *, #128199, .F. ) ;
#39621 = PLANE ( 'NONE',  #111045 ) ;
#39622 = LINE ( 'NONE', #79523, #68841 ) ;
#39623 = CARTESIAN_POINT ( 'NONE',  ( -6.850000000000017408, 2.500000000000000000, -1.918653347947325782 ) ) ;
#39624 = FACE_BOUND ( 'NONE', #123577, .T. ) ;
#39625 = ORIENTED_EDGE ( 'NONE', *, *, #78843, .F. ) ;
#39626 = AXIS2_PLACEMENT_3D ( 'NONE', #82091, #32383, #21232 ) ;
#39627 = DIRECTION ( 'NONE',  ( 0.000000000000000000, 1.000000000000000000, 0.000000000000000000 ) ) ;
#39628 = CARTESIAN_POINT ( 'NONE',  ( -12.09999999999999609, 2.500000000000000000, -0.6928203230275501445 ) ) ;
#39629 = ORIENTED_EDGE ( 'NONE', *, *, #78075, .T. ) ;
#39631 = CARTESIAN_POINT ( 'NONE',  ( 9.349999999999919709, 12.50000000000000000, 2.511473670974873507 ) ) ;
#39630 = AXIS2_PLACEMENT_3D ( 'NONE', #89293, #119384, #29725 ) ;
#39632 = FACE_OUTER_BOUND ( 'NONE', #84599, .T. ) ;
#39633 = CIRCLE ( 'NONE', #43828, 0.1000000000000002554 ) ;
#39634 = EDGE_CURVE ( 'NONE', #83642, #37705, #1952, .T. ) ;
#39635 = CARTESIAN_POINT ( 'NONE',  ( 11.84999999999990372, 2.500000000000000000, -6.741600689897078169 ) ) ;
#39636 = DIRECTION ( 'NONE',  ( 0.000000000000000000, 0.000000000000000000, 1.000000000000000000 ) ) ;
#39637 = DIRECTION ( 'NONE',  ( 0.000000000000000000, 0.000000000000000000, 1.000000000000000000 ) ) ;
#39638 = LINE ( 'NONE', #68411, #112065 ) ;
#39639 = CARTESIAN_POINT ( 'NONE',  ( -6.900000000000019007, 12.50000000000000000, -0.4115034346978157509 ) ) ;
#39640 = ORIENTED_EDGE ( 'NONE', *, *, #100595, .T. ) ;
#39641 = ORIENTED_EDGE ( 'NONE', *, *, #64325, .F. ) ;
#39642 = ORIENTED_EDGE ( 'NONE', *, *, #27677, .T. ) ;
#39643 = ORIENTED_EDGE ( 'NONE', *, *, #29648, .F. ) ;
#39644 = VERTEX_POINT ( 'NONE', #26126 ) ;
#39645 = AXIS2_PLACEMENT_3D ( 'NONE', #78358, #48901, #88803 ) ;
#39646 = FACE_OUTER_BOUND ( 'NONE', #21097, .T. ) ;
#39647 = DIRECTION ( 'NONE',  ( 0.000000000000000000, 1.000000000000000000, 0.000000000000000000 ) ) ;
#39648 = EDGE_LOOP ( 'NONE', ( #63622, #60124 ) ) ;
#39649 = EDGE_CURVE ( 'NONE', #52738, #94125, #43295, .T. ) ;
#39650 = FACE_BOUND ( 'NONE', #37489, .T. ) ;
#39651 = CARTESIAN_POINT ( 'NONE',  ( 8.749999999999920064, 2.500000000000000000, -2.957883832488653830 ) ) ;
#39652 = DIRECTION ( 'NONE',  ( -0.000000000000000000, 1.000000000000000000, -0.000000000000000000 ) ) ;
#39653 = DIRECTION ( 'NONE',  ( 0.000000000000000000, 1.000000000000000000, 0.000000000000000000 ) ) ;
#39654 = DIRECTION ( 'NONE',  ( 0.000000000000000000, 0.000000000000000000, 1.000000000000000000 ) ) ;
#39655 = DIRECTION ( 'NONE',  ( -4.274815082592931898E-19, -0.9999939076577903929, -0.003490651415223739937 ) ) ;
#39656 = DIRECTION ( 'NONE',  ( 0.000000000000000000, -0.000000000000000000, 1.000000000000000000 ) ) ;
#39657 = VERTEX_POINT ( 'NONE', #5813 ) ;
#39658 = AXIS2_PLACEMENT_3D ( 'NONE', #76705, #7299, #87795 ) ;
#39659 = VERTEX_POINT ( 'NONE', #64105 ) ;
#39660 = VERTEX_POINT ( 'NONE', #46389 ) ;
#39661 = VERTEX_POINT ( 'NONE', #104040 ) ;
#39662 = ORIENTED_EDGE ( 'NONE', *, *, #22464, .T. ) ;
#39663 = CARTESIAN_POINT ( 'NONE',  ( 14.93723468728821580, 2.499999999999999556, 6.174425104148618892 ) ) ;
#39664 = CARTESIAN_POINT ( 'NONE',  ( 17.49862860983166257, -2.500000000000000000, -4.081131818001380474 ) ) ;
#39665 = CONICAL_SURFACE ( 'NONE', #112804, 0.09999999999999999167, 0.003490658503988666988 ) ;
#39666 = VERTEX_POINT ( 'NONE', #45772 ) ;
#39667 = CARTESIAN_POINT ( 'NONE',  ( 6.249999999999932498, 2.500000000000000000, -2.757883832488654097 ) ) ;
#39668 = CARTESIAN_POINT ( 'NONE',  ( -0.8000000000000376810, 2.500000000000000000, -4.430127018922202176 ) ) ;
#39669 = EDGE_CURVE ( 'NONE', #70557, #87886, #70466, .T. ) ;
#39672 = VECTOR ( 'NONE', #50867, 1000.000000000000000 ) ;
#39671 = DIRECTION ( 'NONE',  ( 0.000000000000000000, 1.000000000000000000, 0.000000000000000000 ) ) ;
#39670 = CIRCLE ( 'NONE', #129464, 0.06509327318403745899 ) ;
#39673 = DIRECTION ( 'NONE',  ( -0.000000000000000000, 1.000000000000000000, -0.000000000000000000 ) ) ;
#39674 = CARTESIAN_POINT ( 'NONE',  ( 12.49999999999993960, 2.500000000000000000, 4.330127018922196314 ) ) ;
#39675 = LINE ( 'NONE', #32437, #78178 ) ;
#39676 = AXIS2_PLACEMENT_3D ( 'NONE', #34981, #64410, #65035 ) ;
#39677 = CARTESIAN_POINT ( 'NONE',  ( 127.5000000000000000, 5.000000000000000000, -4.999999999999998224 ) ) ;
#39678 = EDGE_LOOP ( 'NONE', ( #117294, #73739 ) ) ;
#39679 = DIRECTION ( 'NONE',  ( 0.000000000000000000, -0.9999939076577903929, 0.003490651415223739937 ) ) ;
#39680 = EDGE_CURVE ( 'NONE', #57147, #14174, #7762, .T. ) ;
#39682 = AXIS2_PLACEMENT_3D ( 'NONE', #23003, #32834, #41370 ) ;
#39681 = AXIS2_PLACEMENT_3D ( 'NONE', #22007, #30541, #101836 ) ;
#39683 = ORIENTED_EDGE ( 'NONE', *, *, #4734, .T. ) ;
#39684 = ORIENTED_EDGE ( 'NONE', *, *, #23770, .F. ) ;
#39685 = CARTESIAN_POINT ( 'NONE',  ( 1.249999999999986899, 2.500000000000000000, 6.495190528383297135 ) ) ;
#39686 = EDGE_CURVE ( 'NONE', #75669, #65538, #112430, .T. ) ;
#39687 = DIRECTION ( 'NONE',  ( 0.000000000000000000, 1.000000000000000000, 0.000000000000000000 ) ) ;
#39689 = EDGE_CURVE ( 'NONE', #92601, #109495, #116519, .T. ) ;
#39688 = CARTESIAN_POINT ( 'NONE',  ( -2.700000000000030376, 2.500000000000000000, 3.983716857408420964 ) ) ;
#39690 = EDGE_CURVE ( 'NONE', #128991, #11848, #26656, .T. ) ;
#39691 = EDGE_CURVE ( 'NONE', #84059, #111941, #77154, .T. ) ;
#39692 = ORIENTED_EDGE ( 'NONE', *, *, #95409, .F. ) ;
#39693 = VERTEX_POINT ( 'NONE', #76515 ) ;
#39694 = FACE_OUTER_BOUND ( 'NONE', #11496, .T. ) ;
#39696 = EDGE_CURVE ( 'NONE', #65503, #129420, #72713, .T. ) ;
#39695 = DIRECTION ( 'NONE',  ( -0.000000000000000000, 1.000000000000000000, -0.000000000000000000 ) ) ;
#39697 = CARTESIAN_POINT ( 'NONE',  ( -9.400000000000007461, 12.50000000000000000, -0.3464101615137783474 ) ) ;
#39698 = EDGE_CURVE ( 'NONE', #50747, #86566, #114466, .T. ) ;
#39699 = CARTESIAN_POINT ( 'NONE',  ( 3.149999999999944400, 12.50000000000000000, 2.511473670974873507 ) ) ;
#39700 = ORIENTED_EDGE ( 'NONE', *, *, #47219, .F. ) ;
#39701 = ADVANCED_FACE ( 'NONE', ( #124322 ), #26766, .T. ) ;
#39702 = CARTESIAN_POINT ( 'NONE',  ( -2.100000000000033396, 2.500000000000000000, -5.022947341949754119 ) ) ;
#39703 = ADVANCED_FACE ( 'NONE', ( #104661 ), #24192, .T. ) ;
#39704 = ORIENTED_EDGE ( 'NONE', *, *, #14959, .F. ) ;
#39705 = CARTESIAN_POINT ( 'NONE',  ( -11.44999999999999929, 2.500000000000000000, -1.918653347947322230 ) ) ;
#39706 = EDGE_CURVE ( 'NONE', #89734, #16131, #65387, .T. ) ;
#39707 = AXIS2_PLACEMENT_3D ( 'NONE', #61137, #30412, #9460 ) ;
#39708 = ADVANCED_FACE ( 'NONE', ( #85027 ), #89436, .T. ) ;
#39709 = ORIENTED_EDGE ( 'NONE', *, *, #70683, .T. ) ;
#39710 = DIRECTION ( 'NONE',  ( 0.000000000000000000, 0.000000000000000000, 1.000000000000000000 ) ) ;
#39711 = CARTESIAN_POINT ( 'NONE',  ( 87.50000000000001421, -3.975344334345451980, 6.360552532166690476 ) ) ;
#39712 = CARTESIAN_POINT ( 'NONE',  ( -1.050000000000038680, 2.500000000000000000, 2.511473670974873507 ) ) ;
#39714 = EDGE_CURVE ( 'NONE', #42111, #56218, #33019, .T. ) ;
#39713 = PLANE ( 'NONE',  #104428 ) ;
#39715 = ORIENTED_EDGE ( 'NONE', *, *, #52228, .T. ) ;
#39717 = VECTOR ( 'NONE', #104841, 1000.000000000000000 ) ;
#39716 = CIRCLE ( 'NONE', #98156, 0.06509327318403745899 ) ;
#39718 = DIRECTION ( 'NONE',  ( 0.000000000000000000, 0.000000000000000000, -1.000000000000000000 ) ) ;
#39719 = ORIENTED_EDGE ( 'NONE', *, *, #72002, .F. ) ;
#39720 = ORIENTED_EDGE ( 'NONE', *, *, #99658, .T. ) ;
#39721 = LINE ( 'NONE', #48882, #54106 ) ;
#39722 = FACE_OUTER_BOUND ( 'NONE', #60813, .T. ) ;
#39723 = CARTESIAN_POINT ( 'NONE',  ( 6.899999999999926636, 2.500000000000000000, 0.4464101615137736623 ) ) ;
#39724 = CARTESIAN_POINT ( 'NONE',  ( 187.3593750003414016, 0.000000000000000000, 7.564683531250000925 ) ) ;
#39725 = CARTESIAN_POINT ( 'NONE',  ( -14.14999999999998614, 2.500000000000000000, 2.065063509461101621 ) ) ;
#39726 = FACE_OUTER_BOUND ( 'NONE', #77737, .T. ) ;
#39727 = AXIS2_PLACEMENT_3D ( 'NONE', #47293, #66273, #15877 ) ;
#39728 = AXIS2_PLACEMENT_3D ( 'NONE', #112030, #40734, #100900 ) ;
#39729 = DIRECTION ( 'NONE',  ( 0.000000000000000000, 1.000000000000000000, 0.000000000000000000 ) ) ;
#39730 = DIRECTION ( 'NONE',  ( 0.000000000000000000, 0.000000000000000000, -1.000000000000000000 ) ) ;
#39731 = DIRECTION ( 'NONE',  ( -4.274815082592931898E-19, -0.9999939076577903929, -0.003490651415223739937 ) ) ;
#39732 = VECTOR ( 'NONE', #53737, 1000.000000000000000 ) ;
#39733 = ORIENTED_EDGE ( 'NONE', *, *, #37404, .T. ) ;
#39734 = PLANE ( 'NONE',  #17018 ) ;
#39735 = CARTESIAN_POINT ( 'NONE',  ( 9.999999999999912959, 12.50000000000000000, -5.088040615133791356 ) ) ;
#39736 = DIRECTION ( 'NONE',  ( 0.000000000000000000, 1.000000000000000000, 0.000000000000000000 ) ) ;
#39737 = CARTESIAN_POINT ( 'NONE',  ( 3.749999999999940492, 12.50000000000000000, 2.922977105672686982 ) ) ;
#39738 = DIRECTION ( 'NONE',  ( 0.000000000000000000, 0.000000000000000000, -1.000000000000000000 ) ) ;
#39739 = ORIENTED_EDGE ( 'NONE', *, *, #20870, .F. ) ;
#39740 = FACE_OUTER_BOUND ( 'NONE', #82870, .T. ) ;
#39741 = EDGE_CURVE ( 'NONE', #70146, #128034, #99813, .T. ) ;
#39742 = EDGE_CURVE ( 'NONE', #51279, #41599, #1630, .T. ) ;
#39743 = LINE ( 'NONE', #33755, #43012 ) ;
#39745 = VERTEX_POINT ( 'NONE', #117693 ) ;
#39744 = PLANE ( 'NONE',  #19693 ) ;
#39746 = ORIENTED_EDGE ( 'NONE', *, *, #50400, .F. ) ;
#39747 = EDGE_CURVE ( 'NONE', #59105, #2046, #118671, .T. ) ;
#39748 = DIRECTION ( 'NONE',  ( 0.000000000000000000, 0.000000000000000000, 1.000000000000000000 ) ) ;
#39749 = ORIENTED_EDGE ( 'NONE', *, *, #6828, .T. ) ;
#39750 = ORIENTED_EDGE ( 'NONE', *, *, #95508, .F. ) ;
#39751 = ORIENTED_EDGE ( 'NONE', *, *, #17151, .F. ) ;
#39752 = PLANE ( 'NONE',  #69702 ) ;
#39753 = AXIS2_PLACEMENT_3D ( 'NONE', #78480, #118372, #28722 ) ;
#39754 = DIRECTION ( 'NONE',  ( 0.000000000000000000, 0.000000000000000000, -1.000000000000000000 ) ) ;
#39755 = CARTESIAN_POINT ( 'NONE',  ( 2.699999999999946443, 2.500000000000000000, -3.983716857408426293 ) ) ;
#39756 = PLANE ( 'NONE',  #85527 ) ;
#39757 = ORIENTED_EDGE ( 'NONE', *, *, #110402, .T. ) ;
#39759 = AXIS2_PLACEMENT_3D ( 'NONE', #26561, #86094, #66471 ) ;
#39758 = AXIS2_PLACEMENT_3D ( 'NONE', #48094, #55961, #87348 ) ;
#39760 = DIRECTION ( 'NONE',  ( 0.000000000000000000, -0.000000000000000000, 1.000000000000000000 ) ) ;
#39761 = EDGE_LOOP ( 'NONE', ( #104355, #94472 ) ) ;
#39762 = CARTESIAN_POINT ( 'NONE',  ( -12.69999999999999218, 12.50000000000000000, 4.741630453620009789 ) ) ;
#39763 = CARTESIAN_POINT ( 'NONE',  ( 19.61395058415635617, 2.556813634648583022, 4.305699210822707457 ) ) ;
#39764 = DIRECTION ( 'NONE',  ( 0.000000000000000000, 1.000000000000000000, 0.000000000000000000 ) ) ;
#39765 = FACE_OUTER_BOUND ( 'NONE', #24207, .T. ) ;
#39766 = EDGE_LOOP ( 'NONE', ( #80423, #28686, #119198, #121937 ) ) ;
#39767 = CIRCLE ( 'NONE', #123365, 0.1000000000000002554 ) ;
#39768 = ORIENTED_EDGE ( 'NONE', *, *, #102197, .F. ) ;
#39769 = EDGE_LOOP ( 'NONE', ( #51660, #120661, #11229, #3665 ) ) ;
#39770 = VERTEX_POINT ( 'NONE', #109838 ) ;
#39771 = VERTEX_POINT ( 'NONE', #47703 ) ;
#39772 = CARTESIAN_POINT ( 'NONE',  ( -7.499999999999980460, 2.500000000000000000, -0.1000000000000022815 ) ) ;
#39773 = DIRECTION ( 'NONE',  ( 0.000000000000000000, 0.000000000000000000, -1.000000000000000000 ) ) ;
#39774 = DIRECTION ( 'NONE',  ( 0.000000000000000000, 0.000000000000000000, -1.000000000000000000 ) ) ;
#39775 = FACE_BOUND ( 'NONE', #6113, .T. ) ;
#39776 = DIRECTION ( 'NONE',  ( 0.000000000000000000, 0.000000000000000000, 1.000000000000000000 ) ) ;
#39777 = CARTESIAN_POINT ( 'NONE',  ( 187.1145833340161175, 6.668395609140177704, -3.849999999999998312 ) ) ;
#39778 = CARTESIAN_POINT ( 'NONE',  ( 9.599999999999917932, 2.500000000000000000, -2.276824562219559311E-15 ) ) ;
#39779 = CARTESIAN_POINT ( 'NONE',  ( -13.94999999999998863, 2.500000000000000000, -1.718653347947323828 ) ) ;
#39780 = FACE_OUTER_BOUND ( 'NONE', #58970, .T. ) ;
#39781 = CARTESIAN_POINT ( 'NONE',  ( 15.59999999999988951, 12.50000000000000000, -0.3464101615137783474 ) ) ;
#39782 = FACE_OUTER_BOUND ( 'NONE', #64294, .T. ) ;
#39783 = AXIS2_PLACEMENT_3D ( 'NONE', #88260, #28080, #47725 ) ;
#39784 = AXIS2_PLACEMENT_3D ( 'NONE', #38868, #19847, #8073 ) ;
#39785 = PLANE ( 'NONE',  #55675 ) ;
#39786 = VERTEX_POINT ( 'NONE', #38546 ) ;
#39787 = ORIENTED_EDGE ( 'NONE', *, *, #120891, .T. ) ;
#39788 = VERTEX_POINT ( 'NONE', #87605 ) ;
#39789 = VERTEX_POINT ( 'NONE', #18865 ) ;
#39790 = EDGE_CURVE ( 'NONE', #24400, #54589, #62261, .T. ) ;
#39791 = DIRECTION ( 'NONE',  ( 0.000000000000000000, 0.000000000000000000, -1.000000000000000000 ) ) ;
#39792 = DIRECTION ( 'NONE',  ( 0.000000000000000000, 0.000000000000000000, 1.000000000000000000 ) ) ;
#39793 = EDGE_CURVE ( 'NONE', #56486, #83051, #22552, .T. ) ;
#39794 = FACE_BOUND ( 'NONE', #3047, .T. ) ;
#39795 = AXIS2_PLACEMENT_3D ( 'NONE', #121662, #61482, #90923 ) ;
#39796 = CARTESIAN_POINT ( 'NONE',  ( -0.4000000000000392131, 2.500000000000000000, -4.430127018922202176 ) ) ;
#39797 = ORIENTED_EDGE ( 'NONE', *, *, #98643, .T. ) ;
#39798 = DIRECTION ( 'NONE',  ( 0.000000000000000000, 0.000000000000000000, 1.000000000000000000 ) ) ;
#39799 = FACE_OUTER_BOUND ( 'NONE', #76247, .T. ) ;
#39800 = EDGE_CURVE ( 'NONE', #90204, #28068, #85229, .T. ) ;
#39801 = DIRECTION ( 'NONE',  ( 0.000000000000000000, 0.000000000000000000, -1.000000000000000000 ) ) ;
#39802 = DIRECTION ( 'NONE',  ( 0.000000000000000000, 0.000000000000000000, 1.000000000000000000 ) ) ;
#39803 = CIRCLE ( 'NONE', #125455, 0.06509327318403745899 ) ;
#39804 = VERTEX_POINT ( 'NONE', #109171 ) ;
#39805 = DIRECTION ( 'NONE',  ( 0.000000000000000000, -0.000000000000000000, 1.000000000000000000 ) ) ;
#39806 = CIRCLE ( 'NONE', #54443, 0.1000000000000002554 ) ;
#39807 = AXIS2_PLACEMENT_3D ( 'NONE', #116995, #19455, #119579 ) ;
#39808 = VERTEX_POINT ( 'NONE', #19512 ) ;
#39809 = VERTEX_POINT ( 'NONE', #59476 ) ;
#39810 = CARTESIAN_POINT ( 'NONE',  ( -12.49999999999999289, 2.500000000000000000, -0.5928203230275499447 ) ) ;
#39811 = DIRECTION ( 'NONE',  ( 0.000000000000000000, 1.000000000000000000, 0.000000000000000000 ) ) ;
#39812 = ORIENTED_EDGE ( 'NONE', *, *, #49299, .F. ) ;
#39813 = AXIS2_PLACEMENT_3D ( 'NONE', #20905, #109280, #30752 ) ;
#39814 = DIRECTION ( 'NONE',  ( -4.274815082592931898E-19, -0.9999939076577903929, -0.003490651415223739937 ) ) ;
#39816 = EDGE_CURVE ( 'NONE', #31177, #127925, #95704, .T. ) ;
#39815 = CARTESIAN_POINT ( 'NONE',  ( 2.099999999999950351, 2.500000000000000000, -0.5928203230275541635 ) ) ;
#39817 = ORIENTED_EDGE ( 'NONE', *, *, #68482, .T. ) ;
#39818 = DIRECTION ( 'NONE',  ( 0.000000000000000000, 1.000000000000000000, 0.000000000000000000 ) ) ;
#39819 = CONICAL_SURFACE ( 'NONE', #4177, 0.1000000000000002554, 0.003490658503988666988 ) ;
#39820 = EDGE_LOOP ( 'NONE', ( #119447, #28285 ) ) ;
#39821 = DIRECTION ( 'NONE',  ( -0.000000000000000000, -1.000000000000000000, -0.000000000000000000 ) ) ;
#39822 = ORIENTED_EDGE ( 'NONE', *, *, #75437, .F. ) ;
#39823 = FACE_BOUND ( 'NONE', #4996, .T. ) ;
#39824 = EDGE_CURVE ( 'NONE', #37787, #97225, #79730, .T. ) ;
#39825 = ORIENTED_EDGE ( 'NONE', *, *, #100963, .T. ) ;
#39826 = DIRECTION ( 'NONE',  ( -0.000000000000000000, 1.000000000000000000, -0.000000000000000000 ) ) ;
#39827 = ORIENTED_EDGE ( 'NONE', *, *, #50173, .F. ) ;
#39828 = DIRECTION ( 'NONE',  ( 0.000000000000000000, 0.000000000000000000, 1.000000000000000000 ) ) ;
#39829 = CARTESIAN_POINT ( 'NONE',  ( -7.300000000000018474, 2.500000000000000000, 0.3464101615137735735 ) ) ;
#39830 = EDGE_CURVE ( 'NONE', #37733, #120555, #83093, .T. ) ;
#39831 = CARTESIAN_POINT ( 'NONE',  ( -4.150000000000024336, 2.500000000000000000, 2.165063509461097713 ) ) ;
#39833 = EDGE_CURVE ( 'NONE', #77015, #12520, #76829, .T. ) ;
#39832 = DIRECTION ( 'NONE',  ( 1.000000000000000000, 0.000000000000000000, 0.000000000000000000 ) ) ;
#39834 = ADVANCED_FACE ( 'NONE', ( #101950 ), #74773, .T. ) ;
#39835 = CARTESIAN_POINT ( 'NONE',  ( -8.950000000000009948, 12.50000000000000000, 2.446380397790835826 ) ) ;
#39836 = EDGE_CURVE ( 'NONE', #109336, #34349, #74268, .T. ) ;
#39837 = ORIENTED_EDGE ( 'NONE', *, *, #81404, .F. ) ;
#39838 = ORIENTED_EDGE ( 'NONE', *, *, #33077, .F. ) ;
#39839 = ORIENTED_EDGE ( 'NONE', *, *, #12136, .T. ) ;
#39840 = DIRECTION ( 'NONE',  ( 0.000000000000000000, 1.000000000000000000, 0.000000000000000000 ) ) ;
#39841 = DIRECTION ( 'NONE',  ( -0.000000000000000000, 1.000000000000000000, -0.000000000000000000 ) ) ;
#39842 = ADVANCED_FACE ( 'NONE', ( #92114 ), #2438, .T. ) ;
#39844 = DIRECTION ( 'NONE',  ( 0.000000000000000000, 0.000000000000000000, -1.000000000000000000 ) ) ;
#39843 = CIRCLE ( 'NONE', #117150, 0.1000000000000002554 ) ;
#39846 = VERTEX_POINT ( 'NONE', #20814 ) ;
#39845 = ORIENTED_EDGE ( 'NONE', *, *, #19450, .T. ) ;
#39847 = ORIENTED_EDGE ( 'NONE', *, *, #62616, .T. ) ;
#39848 = VECTOR ( 'NONE', #86823, 1000.000000000000000 ) ;
#39849 = EDGE_CURVE ( 'NONE', #107424, #2395, #11630, .T. ) ;
#39850 = CARTESIAN_POINT ( 'NONE',  ( -6.450000000000019718, 2.500000000000000000, -1.818653347947326138 ) ) ;
#39851 = EDGE_LOOP ( 'NONE', ( #76739, #28838, #124041, #105818 ) ) ;
#39852 = DIRECTION ( 'NONE',  ( 0.000000000000000000, 1.000000000000000000, 0.000000000000000000 ) ) ;
#39854 = ADVANCED_FACE ( 'NONE', ( #51572 ), #129176, .T. ) ;
#39853 = CIRCLE ( 'NONE', #31425, 2.000000000000000000 ) ;
#39855 = DIRECTION ( 'NONE',  ( -0.000000000000000000, -1.000000000000000000, -0.000000000000000000 ) ) ;
#39856 = DIRECTION ( 'NONE',  ( 0.000000000000000000, 0.000000000000000000, 1.000000000000000000 ) ) ;
#39857 = DIRECTION ( 'NONE',  ( 0.000000000000000000, 0.000000000000000000, 1.000000000000000000 ) ) ;
#39858 = FACE_OUTER_BOUND ( 'NONE', #584, .T. ) ;
#39859 = CARTESIAN_POINT ( 'NONE',  ( -6.450000000000014388, 2.500000000000000000, 1.818653347947321475 ) ) ;
#39860 = EDGE_CURVE ( 'NONE', #20844, #104463, #28805, .T. ) ;
#39862 = EDGE_CURVE ( 'NONE', #116681, #15958, #101958, .T. ) ;
#39861 = CARTESIAN_POINT ( 'NONE',  ( -9.350000000000006750, 2.500000000000000000, -2.411473670974877859 ) ) ;
#39863 = ORIENTED_EDGE ( 'NONE', *, *, #42955, .F. ) ;
#39864 = ORIENTED_EDGE ( 'NONE', *, *, #69851, .T. ) ;
#39865 = DIRECTION ( 'NONE',  ( 0.000000000000000000, 0.000000000000000000, 1.000000000000000000 ) ) ;
#39866 = ORIENTED_EDGE ( 'NONE', *, *, #19684, .T. ) ;
#39867 = VERTEX_POINT ( 'NONE', #111772 ) ;
#39868 = CARTESIAN_POINT ( 'NONE',  ( 1.649999999999951950, 2.500000000000000000, -7.288010851410854585 ) ) ;
#39869 = LINE ( 'NONE', #16937, #36473 ) ;
#39870 = DIRECTION ( 'NONE',  ( 0.000000000000000000, 0.000000000000000000, 1.000000000000000000 ) ) ;
#39871 = DIRECTION ( 'NONE',  ( 0.000000000000000000, -0.9999939076577903929, 0.003490651415223739937 ) ) ;
#39872 = CARTESIAN_POINT ( 'NONE',  ( 3.749999999999975131, 2.500000000000000000, 6.595190528383296780 ) ) ;
#39873 = DIRECTION ( 'NONE',  ( 0.000000000000000000, 1.000000000000000000, 0.000000000000000000 ) ) ;
#39874 = CARTESIAN_POINT ( 'NONE',  ( 13.29999999999989946, 12.50000000000000000, -0.06509327318403980434 ) ) ;
#39875 = DIRECTION ( 'NONE',  ( -0.000000000000000000, -1.000000000000000000, -0.000000000000000000 ) ) ;
#39876 = CIRCLE ( 'NONE', #100488, 0.06509327318403745899 ) ;
#39878 = EDGE_LOOP ( 'NONE', ( #123631, #82295 ) ) ;
#39877 = AXIS2_PLACEMENT_3D ( 'NONE', #13576, #54789, #24705 ) ;
#39879 = ORIENTED_EDGE ( 'NONE', *, *, #20183, .T. ) ;
#39880 = ORIENTED_EDGE ( 'NONE', *, *, #1544, .T. ) ;
#39881 = ORIENTED_EDGE ( 'NONE', *, *, #119582, .F. ) ;
#39882 = DIRECTION ( 'NONE',  ( -0.000000000000000000, -1.000000000000000000, -0.000000000000000000 ) ) ;
#39883 = CARTESIAN_POINT ( 'NONE',  ( -11.84999999999999609, 2.500000000000000000, 6.741600689897071952 ) ) ;
#39884 = CONICAL_SURFACE ( 'NONE', #113019, 0.1000000000000002554, 0.003490658503988666988 ) ;
#39885 = VERTEX_POINT ( 'NONE', #65065 ) ;
#39886 = DIRECTION ( 'NONE',  ( -0.000000000000000000, -1.000000000000000000, -0.000000000000000000 ) ) ;
#39887 = EDGE_CURVE ( 'NONE', #120491, #47940, #91486, .T. ) ;
#39888 = DIRECTION ( 'NONE',  ( 0.000000000000000000, 0.000000000000000000, -1.000000000000000000 ) ) ;
#39889 = ADVANCED_FACE ( 'NONE', ( #30646 ), #10959, .T. ) ;
#39890 = LINE ( 'NONE', #71254, #65771 ) ;
#39892 = ORIENTED_EDGE ( 'NONE', *, *, #7695, .T. ) ;
#39891 = CARTESIAN_POINT ( 'NONE',  ( 0.000000000000000000, 0.000000000000000000, -5.000000000000004441 ) ) ;
#39893 =( BOUNDED_SURFACE ( )  B_SPLINE_SURFACE ( 3, 2, ( 
 ( #98865, #9200, #49150 ),
 ( #89058, #129008, #26913 ),
 ( #28203, #69400, #68113 ),
 ( #47854, #39337, #109334 ) ),
 .UNSPECIFIED., .F., .F., .F. ) 
 B_SPLINE_SURFACE_WITH_KNOTS ( ( 4, 4 ),
 ( 3, 3 ),
 ( 0.000000000000000000, 0.002140783067917607571 ),
 ( 0.000000000000000000, 1.000000000000000000 ),
 .UNSPECIFIED. ) 
 GEOMETRIC_REPRESENTATION_ITEM ( )  RATIONAL_B_SPLINE_SURFACE ( (
 ( 1.000000000000000000, 0.7071067811865471286, 1.000000000000000000),
 ( 1.000000000000000000, 0.7083221562484207645, 1.000000000000000000),
 ( 1.000000000000000000, 0.7095583416414845690, 1.000000000000000000),
 ( 1.000000000000000000, 0.7108129113927459386, 1.000000000000000000) ) ) 
 REPRESENTATION_ITEM ( '' )  SURFACE ( )  );
#39894 = DIRECTION ( 'NONE',  ( 0.000000000000000000, 0.000000000000000000, -1.000000000000000000 ) ) ;
#39895 = DIRECTION ( 'NONE',  ( 0.000000000000000000, 1.000000000000000000, 0.000000000000000000 ) ) ;
#39896 = AXIS2_PLACEMENT_3D ( 'NONE', #121657, #113128, #111181 ) ;
#39897 = ORIENTED_EDGE ( 'NONE', *, *, #21998, .T. ) ;
#39898 = AXIS2_PLACEMENT_3D ( 'NONE', #442, #60056, #71791 ) ;
#39899 = EDGE_LOOP ( 'NONE', ( #46816, #60776, #7193, #98671 ) ) ;
#39900 = EDGE_LOOP ( 'NONE', ( #45653, #115537 ) ) ;
#39901 = VERTEX_POINT ( 'NONE', #101313 ) ;
#39902 = DIRECTION ( 'NONE',  ( 0.000000000000000000, -0.000000000000000000, 1.000000000000000000 ) ) ;
#39903 = AXIS2_PLACEMENT_3D ( 'NONE', #24781, #114431, #84975 ) ;
#39904 = CARTESIAN_POINT ( 'NONE',  ( 8.749999999999957367, 2.500000000000000000, -6.495190528383302464 ) ) ;
#39905 = CARTESIAN_POINT ( 'NONE',  ( -14.99999999999994671, 12.50000000000000000, 0.000000000000000000 ) ) ;
#39906 = AXIS2_PLACEMENT_3D ( 'NONE', #95307, #6254, #116219 ) ;
#39907 = ORIENTED_EDGE ( 'NONE', *, *, #25311, .F. ) ;
#39908 = DIRECTION ( 'NONE',  ( 0.000000000000000000, 0.000000000000000000, 1.000000000000000000 ) ) ;
#39909 = CARTESIAN_POINT ( 'NONE',  ( 20.37757664703730853, -0.6627606010239102119, -4.188167776336774395 ) ) ;
#39910 = CARTESIAN_POINT ( 'NONE',  ( -1.650000000000034772, 2.500000000000000000, 6.395190528383296602 ) ) ;
#39911 = DIRECTION ( 'NONE',  ( -0.000000000000000000, 1.000000000000000000, -0.000000000000000000 ) ) ;
#39912 = ORIENTED_EDGE ( 'NONE', *, *, #100947, .F. ) ;
#39913 = PLANE ( 'NONE',  #29098 ) ;
#39914 = ORIENTED_EDGE ( 'NONE', *, *, #104676, .T. ) ;
#39915 = VERTEX_POINT ( 'NONE', #84723 ) ;
#39916 = CARTESIAN_POINT ( 'NONE',  ( 13.34999999999990017, 12.50000000000000000, 2.165063509461097713 ) ) ;
#39917 = CARTESIAN_POINT ( 'NONE',  ( 7.099999999999927702, 2.500000000000000000, -3.637306695894650055 ) ) ;
#39918 = FACE_BOUND ( 'NONE', #95628, .T. ) ;
#39919 = CARTESIAN_POINT ( 'NONE',  ( 7.299999999999927880, 12.50000000000000000, 3.983716857408420964 ) ) ;
#39920 = CARTESIAN_POINT ( 'NONE',  ( 1.849999999999949685, 2.500000000000000000, 1.918653347947321564 ) ) ;
#39921 = DIRECTION ( 'NONE',  ( 0.000000000000000000, 0.000000000000000000, 1.000000000000000000 ) ) ;
#39922 = EDGE_CURVE ( 'NONE', #120005, #117161, #14677, .T. ) ;
#39923 = CIRCLE ( 'NONE', #46163, 0.06509327318403741736 ) ;
#39924 = CONICAL_SURFACE ( 'NONE', #117245, 0.09999999999999999167, 0.003490658503988666988 ) ;
#39926 = AXIS2_PLACEMENT_3D ( 'NONE', #89413, #37738, #48195 ) ;
#39925 = LINE ( 'NONE', #99489, #27550 ) ;
#39927 = DIRECTION ( 'NONE',  ( 0.000000000000000000, 1.000000000000000000, 0.000000000000000000 ) ) ;
#39928 = CARTESIAN_POINT ( 'NONE',  ( 8.099999999999923261, 2.500000000000000000, 4.083716857408420609 ) ) ;
#39929 = ORIENTED_EDGE ( 'NONE', *, *, #118219, .T. ) ;
#39930 = EDGE_CURVE ( 'NONE', #37231, #46960, #127002, .T. ) ;
#39931 = DIRECTION ( 'NONE',  ( 0.000000000000000000, -0.000000000000000000, 1.000000000000000000 ) ) ;
#39932 = LINE ( 'NONE', #100136, #68383 ) ;
#39933 = ORIENTED_EDGE ( 'NONE', *, *, #17479, .F. ) ;
#39934 = ORIENTED_EDGE ( 'NONE', *, *, #44062, .T. ) ;
#39935 = EDGE_CURVE ( 'NONE', #106998, #108508, #104012, .T. ) ;
#39936 = CARTESIAN_POINT ( 'NONE',  ( 11.84999999999990727, 12.50000000000000000, -1.818653347947326138 ) ) ;
#39938 = ADVANCED_FACE ( 'NONE', ( #1166 ), #74914, .T. ) ;
#39937 = DIRECTION ( 'NONE',  ( 1.000000000000000000, 0.000000000000000000, 0.000000000000000000 ) ) ;
#39939 = FACE_BOUND ( 'NONE', #5590, .T. ) ;
#39940 = CARTESIAN_POINT ( 'NONE',  ( -10.40000000000000213, 12.50000000000000000, 3.572213422710607489 ) ) ;
#39941 = DIRECTION ( 'NONE',  ( 0.000000000000000000, 0.000000000000000000, 1.000000000000000000 ) ) ;
#39942 = ORIENTED_EDGE ( 'NONE', *, *, #64943, .T. ) ;
#39943 = CARTESIAN_POINT ( 'NONE',  ( -1.700000000000035261, 12.50000000000000000, 4.330127018922196314 ) ) ;
#39944 = EDGE_CURVE ( 'NONE', #113749, #64996, #7851, .T. ) ;
#39945 = CARTESIAN_POINT ( 'NONE',  ( -6.450000000000017941, 12.50000000000000000, -6.841600689897077814 ) ) ;
#39946 = EDGE_LOOP ( 'NONE', ( #5324, #15850, #13325, #9185 ) ) ;
#39947 = LINE ( 'NONE', #69385, #5041 ) ;
#39948 = DIRECTION ( 'NONE',  ( 0.000000000000000000, 0.000000000000000000, -1.000000000000000000 ) ) ;
#39949 = CIRCLE ( 'NONE', #54586, 0.09999999999999982514 ) ;
#39950 = CARTESIAN_POINT ( 'NONE',  ( 185.7395833340161175, 4.445597072760159030, 7.699999999999928235 ) ) ;
#39951 = DIRECTION ( 'NONE',  ( 0.000000000000000000, 1.000000000000000000, 0.000000000000000000 ) ) ;
#39952 = VECTOR ( 'NONE', #58860, 1000.000000000000000 ) ;
#39953 = CIRCLE ( 'NONE', #77582, 0.1000000000000000472 ) ;
#39954 = EDGE_LOOP ( 'NONE', ( #90915, #97414 ) ) ;
#39955 = CARTESIAN_POINT ( 'NONE',  ( -2.500000000000031086, 12.50000000000000000, 3.572213422710607489 ) ) ;
#39956 = DIRECTION ( 'NONE',  ( -0.000000000000000000, 1.000000000000000000, -0.000000000000000000 ) ) ;
#39957 = DIRECTION ( 'NONE',  ( 0.000000000000000000, 1.000000000000000000, 0.000000000000000000 ) ) ;
#39958 = DIRECTION ( 'NONE',  ( 0.000000000000000000, 1.000000000000000000, 0.000000000000000000 ) ) ;
#39959 = EDGE_LOOP ( 'NONE', ( #24361, #51981 ) ) ;
#39960 = VERTEX_POINT ( 'NONE', #5503 ) ;
#39961 = DIRECTION ( 'NONE',  ( 0.000000000000000000, 1.000000000000000000, 0.000000000000000000 ) ) ;
#39962 = CIRCLE ( 'NONE', #113109, 0.06509327318403741736 ) ;
#39963 = VERTEX_POINT ( 'NONE', #81022 ) ;
#39964 = FACE_OUTER_BOUND ( 'NONE', #79875, .T. ) ;
#39965 = AXIS2_PLACEMENT_3D ( 'NONE', #2632, #22318, #12463 ) ;
#39966 = CARTESIAN_POINT ( 'NONE',  ( 87.50000000000000000, -7.032605354647524010, -2.693424153406288823 ) ) ;
#39967 = EDGE_CURVE ( 'NONE', #100871, #79060, #51791, .T. ) ;
#39968 = LINE ( 'NONE', #100173, #50796 ) ;
#39969 = ORIENTED_EDGE ( 'NONE', *, *, #88293, .F. ) ;
#39970 = DIRECTION ( 'NONE',  ( 0.000000000000000000, 0.000000000000000000, -1.000000000000000000 ) ) ;
#39971 = DIRECTION ( 'NONE',  ( -0.000000000000000000, -1.000000000000000000, -0.000000000000000000 ) ) ;
#39972 = DIRECTION ( 'NONE',  ( -4.274815082592931898E-19, -0.9999939076577903929, -0.003490651415223739937 ) ) ;
#39973 = CARTESIAN_POINT ( 'NONE',  ( 4.149999999999941735, 2.500000000000000000, -2.857883832488653741 ) ) ;
#39974 = DIRECTION ( 'NONE',  ( 0.000000000000000000, 1.000000000000000000, 0.000000000000000000 ) ) ;
#39975 = EDGE_CURVE ( 'NONE', #121075, #70528, #68499, .T. ) ;
#39976 = CARTESIAN_POINT ( 'NONE',  ( 9.349999999999916156, 2.500000000000000000, 6.941600689897073018 ) ) ;
#39977 = EDGE_CURVE ( 'NONE', #75731, #91809, #125300, .T. ) ;
#39978 = AXIS2_PLACEMENT_3D ( 'NONE', #68535, #117608, #27309 ) ;
#39979 = ORIENTED_EDGE ( 'NONE', *, *, #70825, .T. ) ;
#39980 = VECTOR ( 'NONE', #19956, 1000.000000000000000 ) ;
#39981 = ORIENTED_EDGE ( 'NONE', *, *, #112931, .T. ) ;
#39982 = CARTESIAN_POINT ( 'NONE',  ( 2.099999999999949463, 2.500000000000000000, -3.637306695894650055 ) ) ;
#39983 = ORIENTED_EDGE ( 'NONE', *, *, #78683, .T. ) ;
#39984 = CARTESIAN_POINT ( 'NONE',  ( 104.0450469811252532, 7.064712996401804723, 3.075733052666039580 ) ) ;
#39985 = ADVANCED_FACE ( 'NONE', ( #105664 ), #17244, .T. ) ;
#39987 = ORIENTED_EDGE ( 'NONE', *, *, #21025, .F. ) ;
#39986 = VERTEX_POINT ( 'NONE', #85991 ) ;
#39988 = EDGE_CURVE ( 'NONE', #28707, #58259, #91863, .T. ) ;
#39989 = ORIENTED_EDGE ( 'NONE', *, *, #128504, .F. ) ;
#39990 = EDGE_CURVE ( 'NONE', #47267, #77184, #24688, .T. ) ;
#39991 = FACE_OUTER_BOUND ( 'NONE', #75164, .T. ) ;
#39993 = EDGE_CURVE ( 'NONE', #126433, #115678, #70650, .T. ) ;
#39992 = VECTOR ( 'NONE', #44912, 1000.000000000000000 ) ;
#39994 = DIRECTION ( 'NONE',  ( 0.000000000000000000, 0.000000000000000000, 1.000000000000000000 ) ) ;
#39995 = CARTESIAN_POINT ( 'NONE',  ( -11.25000000000000178, 12.50000000000000000, -5.802370205355746435 ) ) ;
#39996 = ADVANCED_FACE ( 'NONE', ( #17910 ), #76909, .T. ) ;
#39997 = DIRECTION ( 'NONE',  ( -4.274815082592931898E-19, -0.9999939076577903929, -0.003490651415223739937 ) ) ;
#39998 = AXIS2_PLACEMENT_3D ( 'NONE', #104326, #27057, #84681 ) ;
#39999 = AXIS2_PLACEMENT_3D ( 'NONE', #124194, #33256, #35184 ) ;
#40000 = DIRECTION ( 'NONE',  ( 0.000000000000000000, 1.000000000000000000, 0.000000000000000000 ) ) ;
#40001 = CARTESIAN_POINT ( 'NONE',  ( 185.7500000000000000, 9.429780353434619030E-16, -7.700000000000000178 ) ) ;
#40002 = DIRECTION ( 'NONE',  ( 0.000000000000000000, 0.000000000000000000, 1.000000000000000000 ) ) ;
#40003 = CARTESIAN_POINT ( 'NONE',  ( 13.74999999999993427, 2.500000000000000000, 2.165063509461097713 ) ) ;
#40005 = EDGE_CURVE ( 'NONE', #15792, #77218, #97124, .T. ) ;
#40004 = DIRECTION ( 'NONE',  ( 0.000000000000000000, -0.000000000000000000, 1.000000000000000000 ) ) ;
#40006 = EDGE_LOOP ( 'NONE', ( #84142, #123286, #118928, #103056 ) ) ;
#40007 = VERTEX_POINT ( 'NONE', #46743 ) ;
#40008 = DIRECTION ( 'NONE',  ( 0.000000000000000000, 1.000000000000000000, 0.000000000000000000 ) ) ;
#40009 = EDGE_LOOP ( 'NONE', ( #87018, #99047, #59133, #94523 ) ) ;
#40010 = ORIENTED_EDGE ( 'NONE', *, *, #54603, .T. ) ;
#40011 = CARTESIAN_POINT ( 'NONE',  ( 1.649999999999951061, 12.50000000000000000, -6.560283801567339701 ) ) ;
#40012 = CARTESIAN_POINT ( 'NONE',  ( -5.850000000000021849, 2.500000000000000000, -2.957883832488653830 ) ) ;
#40013 = LINE ( 'NONE', #60925, #67342 ) ;
#40014 = DIRECTION ( 'NONE',  ( -0.000000000000000000, 1.000000000000000000, -0.000000000000000000 ) ) ;
#40015 = AXIS2_PLACEMENT_3D ( 'NONE', #113235, #42596, #63512 ) ;
#40016 = DIRECTION ( 'NONE',  ( 0.000000000000000000, 1.000000000000000000, 0.000000000000000000 ) ) ;
#40017 = VERTEX_POINT ( 'NONE', #87293 ) ;
#40018 = CIRCLE ( 'NONE', #272, 0.06509327318403745899 ) ;
#40019 = AXIS2_PLACEMENT_3D ( 'NONE', #59168, #107610, #99086 ) ;
#40020 = ORIENTED_EDGE ( 'NONE', *, *, #69369, .F. ) ;
#40021 = DIRECTION ( 'NONE',  ( -0.000000000000000000, -1.000000000000000000, -0.000000000000000000 ) ) ;
#40022 = AXIS2_PLACEMENT_3D ( 'NONE', #66119, #6520, #77235 ) ;
#40023 = ORIENTED_EDGE ( 'NONE', *, *, #103814, .F. ) ;
#40024 = AXIS2_PLACEMENT_3D ( 'NONE', #16759, #105155, #55427 ) ;
#40025 = ORIENTED_EDGE ( 'NONE', *, *, #33624, .F. ) ;
#40026 = VECTOR ( 'NONE', #87303, 1000.000000000000000 ) ;
#40027 = ORIENTED_EDGE ( 'NONE', *, *, #124342, .F. ) ;
#40028 = CARTESIAN_POINT ( 'NONE',  ( 3.749999999999940492, 2.500000000000000000, 2.757883832488649656 ) ) ;
#40029 = DIRECTION ( 'NONE',  ( -4.274815082592931898E-19, -0.9999939076577903929, -0.003490651415223739937 ) ) ;
#40030 = FACE_OUTER_BOUND ( 'NONE', #72335, .T. ) ;
#40031 = EDGE_CURVE ( 'NONE', #39771, #16038, #28901, .T. ) ;
#40032 = CARTESIAN_POINT ( 'NONE',  ( 0.8499999999999527933, 2.500000000000000000, 7.188010851410848723 ) ) ;
#40033 = FACE_OUTER_BOUND ( 'NONE', #45212, .T. ) ;
#40034 = VERTEX_POINT ( 'NONE', #47391 ) ;
#40035 = DIRECTION ( 'NONE',  ( 0.000000000000000000, 1.000000000000000000, 0.000000000000000000 ) ) ;
#40036 = LINE ( 'NONE', #79945, #55781 ) ;
#40037 = DIRECTION ( 'NONE',  ( 0.000000000000000000, 0.000000000000000000, 1.000000000000000000 ) ) ;
#40038 = DIRECTION ( 'NONE',  ( 0.000000000000000000, 0.000000000000000000, -1.000000000000000000 ) ) ;
#40040 = ADVANCED_FACE ( 'NONE', ( #65725 ), #28395, .T. ) ;
#40039 = CARTESIAN_POINT ( 'NONE',  ( 12.49999999999990052, 2.500000000000000000, 0.5928203230275495006 ) ) ;
#40041 = VERTEX_POINT ( 'NONE', #55905 ) ;
#40042 = ORIENTED_EDGE ( 'NONE', *, *, #88118, .F. ) ;
#40043 = DIRECTION ( 'NONE',  ( -0.000000000000000000, -1.000000000000000000, -0.000000000000000000 ) ) ;
#40044 = ORIENTED_EDGE ( 'NONE', *, *, #92673, .T. ) ;
#40045 = CARTESIAN_POINT ( 'NONE',  ( 4.799999999999935874, 2.500000000000000000, 3.983716857408420964 ) ) ;
#40046 = AXIS2_PLACEMENT_3D ( 'NONE', #86211, #68514, #37779 ) ;
#40047 = DIRECTION ( 'NONE',  ( 0.000000000000000000, 0.000000000000000000, -1.000000000000000000 ) ) ;
#40048 = CIRCLE ( 'NONE', #8622, 0.1000000000000002554 ) ;
#40049 = ORIENTED_EDGE ( 'NONE', *, *, #75726, .F. ) ;
#40050 = DIRECTION ( 'NONE',  ( 0.000000000000000000, -0.000000000000000000, 1.000000000000000000 ) ) ;
#40051 = CARTESIAN_POINT ( 'NONE',  ( 11.04999999999990656, 12.50000000000000000, 2.446380397790835826 ) ) ;
#40052 = CARTESIAN_POINT ( 'NONE',  ( -7.500000000000001776, -2.500000000000000000, -9.000000000000000000 ) ) ;
#40053 = CARTESIAN_POINT ( 'NONE',  ( -5.850000000000021849, 2.500000000000000000, -7.188010851410854052 ) ) ;
#40054 = AXIS2_PLACEMENT_3D ( 'NONE', #41846, #41206, #21543 ) ;
#40055 = CIRCLE ( 'NONE', #52567, 0.09999999999999982514 ) ;
#40056 = CARTESIAN_POINT ( 'NONE',  ( -10.85000000000000142, 2.500000000000000000, 2.065063509461097624 ) ) ;
#40057 = CONICAL_SURFACE ( 'NONE', #88138, 0.1000000000000000472, 0.003490658503988666988 ) ;
#40058 = EDGE_LOOP ( 'NONE', ( #38157, #125915, #45592, #7431 ) ) ;
#40059 = CARTESIAN_POINT ( 'NONE',  ( 14.59999999999989484, 12.50000000000000000, -0.6277270498435166823 ) ) ;
#40060 = DIRECTION ( 'NONE',  ( 0.000000000000000000, 1.000000000000000000, 0.000000000000000000 ) ) ;
#40061 = CARTESIAN_POINT ( 'NONE',  ( -15.19999999999998330, 12.50000000000000000, 0.4115034346978132529 ) ) ;
#40062 = AXIS2_PLACEMENT_3D ( 'NONE', #100569, #10884, #80309 ) ;
#40063 = AXIS2_PLACEMENT_3D ( 'NONE', #23162, #43472, #34298 ) ;
#40064 = EDGE_CURVE ( 'NONE', #117090, #13161, #56059, .T. ) ;
#40065 = VERTEX_POINT ( 'NONE', #45467 ) ;
#40066 = DIRECTION ( 'NONE',  ( 0.000000000000000000, 1.000000000000000000, 0.000000000000000000 ) ) ;
#40067 = AXIS2_PLACEMENT_3D ( 'NONE', #18130, #128099, #37786 ) ;
#40068 = ORIENTED_EDGE ( 'NONE', *, *, #112203, .T. ) ;
#40069 = DIRECTION ( 'NONE',  ( 0.000000000000000000, 0.000000000000000000, 1.000000000000000000 ) ) ;
#40070 = DIRECTION ( 'NONE',  ( 0.000000000000000000, -0.000000000000000000, 1.000000000000000000 ) ) ;
#40071 = AXIS2_PLACEMENT_3D ( 'NONE', #99807, #98493, #29770 ) ;
#40072 = PLANE ( 'NONE',  #7842 ) ;
#40073 = ORIENTED_EDGE ( 'NONE', *, *, #66656, .T. ) ;
#40074 = EDGE_CURVE ( 'NONE', #111424, #33882, #79077, .T. ) ;
#40075 = DIRECTION ( 'NONE',  ( 0.000000000000000000, 1.000000000000000000, 0.000000000000000000 ) ) ;
#40076 = CARTESIAN_POINT ( 'NONE',  ( 185.4062500006828031, -8.891194145520236347, -1.633285867636356299E-15 ) ) ;
#40077 = CIRCLE ( 'NONE', #35965, 0.09999999999999982514 ) ;
#40078 = AXIS2_PLACEMENT_3D ( 'NONE', #112926, #114220, #93936 ) ;
#40079 = VERTEX_POINT ( 'NONE', #48040 ) ;
#40080 = EDGE_CURVE ( 'NONE', #121980, #14780, #99908, .T. ) ;
#40081 = DIRECTION ( 'NONE',  ( -0.000000000000000000, -1.000000000000000000, -0.000000000000000000 ) ) ;
#40082 = EDGE_CURVE ( 'NONE', #127955, #69509, #35637, .T. ) ;
#40083 = VERTEX_POINT ( 'NONE', #6151 ) ;
#40084 = DIRECTION ( 'NONE',  ( -0.000000000000000000, -1.000000000000000000, -0.000000000000000000 ) ) ;
#40085 = ORIENTED_EDGE ( 'NONE', *, *, #76416, .F. ) ;
#40086 = DIRECTION ( 'NONE',  ( -0.000000000000000000, 1.000000000000000000, -0.000000000000000000 ) ) ;
#40087 = ADVANCED_FACE ( 'NONE', ( #56544 ), #46098, .T. ) ;
#40088 = ORIENTED_EDGE ( 'NONE', *, *, #60092, .F. ) ;
#40089 = VERTEX_POINT ( 'NONE', #116115 ) ;
#40090 = ADVANCED_FACE ( 'NONE', ( #40146 ), #51272, .T. ) ;
#40091 = DIRECTION ( 'NONE',  ( -0.000000000000000000, -1.000000000000000000, -0.000000000000000000 ) ) ;
#40092 = CARTESIAN_POINT ( 'NONE',  ( 0.7999999999999553024, 2.500000000000000000, -4.230127018922201998 ) ) ;
#40093 = EDGE_LOOP ( 'NONE', ( #3819, #30642, #47044, #26753 ) ) ;
#40094 = CARTESIAN_POINT ( 'NONE',  ( -13.54999999999998828, 2.500000000000000000, -2.511473670974875727 ) ) ;
#40095 = CARTESIAN_POINT ( 'NONE',  ( 187.0260416670080588, -6.551208109652273848, -3.782341765625003571 ) ) ;
#40096 = FACE_OUTER_BOUND ( 'NONE', #12730, .T. ) ;
#40097 = AXIS2_PLACEMENT_3D ( 'NONE', #111206, #121683, #60219 ) ;
#40098 = DIRECTION ( 'NONE',  ( 0.000000000000000000, 0.000000000000000000, 1.000000000000000000 ) ) ;
#40099 = DIRECTION ( 'NONE',  ( -4.274815082592931898E-19, -0.9999939076577903929, -0.003490651415223739937 ) ) ;
#40100 = CIRCLE ( 'NONE', #69322, 0.06509327318403745899 ) ;
#40101 = AXIS2_PLACEMENT_3D ( 'NONE', #115304, #6014, #25663 ) ;
#40102 = FACE_OUTER_BOUND ( 'NONE', #84901, .T. ) ;
#40103 = DIRECTION ( 'NONE',  ( -0.000000000000000000, 1.000000000000000000, -0.000000000000000000 ) ) ;
#40104 = AXIS2_PLACEMENT_3D ( 'NONE', #69335, #41205, #100109 ) ;
#40105 = ORIENTED_EDGE ( 'NONE', *, *, #82452, .T. ) ;
#40107 = ORIENTED_EDGE ( 'NONE', *, *, #40847, .F. ) ;
#40106 = CIRCLE ( 'NONE', #63085, 0.06509327318403745899 ) ;
#40108 = EDGE_LOOP ( 'NONE', ( #21951, #31986 ) ) ;
#40109 = DIRECTION ( 'NONE',  ( 0.000000000000000000, 0.000000000000000000, 1.000000000000000000 ) ) ;
#40110 = CARTESIAN_POINT ( 'NONE',  ( -11.89999999999999680, 2.500000000000000000, -4.676537180435976104 ) ) ;
#40111 = AXIS2_PLACEMENT_3D ( 'NONE', #19334, #68439, #69740 ) ;
#40112 = DIRECTION ( 'NONE',  ( -0.000000000000000000, 1.000000000000000000, -0.000000000000000000 ) ) ;
#40113 = EDGE_LOOP ( 'NONE', ( #40233, #18766, #58477, #56651 ) ) ;
#40114 = FACE_BOUND ( 'NONE', #48137, .T. ) ;
#40115 = ORIENTED_EDGE ( 'NONE', *, *, #104221, .F. ) ;
#40116 = DIRECTION ( 'NONE',  ( 0.000000000000000000, 0.000000000000000000, -1.000000000000000000 ) ) ;
#40117 = DIRECTION ( 'NONE',  ( 0.000000000000000000, 1.000000000000000000, 0.000000000000000000 ) ) ;
#40118 = DIRECTION ( 'NONE',  ( -4.274815082592931898E-19, -0.9999939076577903929, -0.003490651415223739937 ) ) ;
#40119 = CARTESIAN_POINT ( 'NONE',  ( 7.299999999999924327, 2.500000000000000000, 0.2464101615137735679 ) ) ;
#40120 = CARTESIAN_POINT ( 'NONE',  ( 8.099999999999923261, 12.50000000000000000, 4.741630453620009789 ) ) ;
#40121 = CARTESIAN_POINT ( 'NONE',  ( 6.249999999999965361, 2.500000000000000000, 2.165063509461097713 ) ) ;
#40122 = DIRECTION ( 'NONE',  ( 0.000000000000000000, 1.000000000000000000, 0.000000000000000000 ) ) ;
#40123 = DIRECTION ( 'NONE',  ( 0.000000000000000000, 1.000000000000000000, 0.000000000000000000 ) ) ;
#40124 = DIRECTION ( 'NONE',  ( 0.000000000000000000, -0.9999939076577903929, 0.003490651415223739937 ) ) ;
#40125 = ORIENTED_EDGE ( 'NONE', *, *, #49530, .T. ) ;
#40126 = ORIENTED_EDGE ( 'NONE', *, *, #83385, .F. ) ;
#40127 = ORIENTED_EDGE ( 'NONE', *, *, #92792, .F. ) ;
#40128 = VERTEX_POINT ( 'NONE', #79437 ) ;
#40129 = CARTESIAN_POINT ( 'NONE',  ( -12.49999999999995914, 2.500000000000000000, 0.1000000000000018513 ) ) ;
#40130 = ADVANCED_FACE ( 'NONE', ( #21137 ), #120634, .T. ) ;
#40131 = DIRECTION ( 'NONE',  ( -0.000000000000000000, 1.000000000000000000, -0.000000000000000000 ) ) ;
#40132 = EDGE_CURVE ( 'NONE', #85147, #72947, #70249, .T. ) ;
#40134 = ORIENTED_EDGE ( 'NONE', *, *, #51657, .F. ) ;
#40133 = VERTEX_POINT ( 'NONE', #60450 ) ;
#40135 = EDGE_LOOP ( 'NONE', ( #120855, #56282, #67009, #27980 ) ) ;
#40136 = EDGE_CURVE ( 'NONE', #78385, #74255, #83187, .T. ) ;
#40137 = CARTESIAN_POINT ( 'NONE',  ( -4.150000000000024336, 2.500000000000000000, 2.165063509461097713 ) ) ;
#40138 = EDGE_CURVE ( 'NONE', #113689, #107267, #129264, .T. ) ;
#40139 = CONICAL_SURFACE ( 'NONE', #98691, 0.1000000000000002554, 0.003490658503988666988 ) ;
#40140 = AXIS2_PLACEMENT_3D ( 'NONE', #26977, #105536, #116629 ) ;
#40141 = DIRECTION ( 'NONE',  ( 0.000000000000000000, 0.000000000000000000, 1.000000000000000000 ) ) ;
#40142 = CARTESIAN_POINT ( 'NONE',  ( -6.900000000000015454, 12.50000000000000000, 4.611443907251934426 ) ) ;
#40143 = CARTESIAN_POINT ( 'NONE',  ( 11.84999999999990727, 12.50000000000000000, -2.576566944158915184 ) ) ;
#40144 = EDGE_CURVE ( 'NONE', #95427, #113919, #25056, .T. ) ;
#40145 = DIRECTION ( 'NONE',  ( -0.000000000000000000, -1.000000000000000000, -0.000000000000000000 ) ) ;
#40146 = FACE_OUTER_BOUND ( 'NONE', #14191, .T. ) ;
#40147 = DIRECTION ( 'NONE',  ( 0.000000000000000000, 0.000000000000000000, 1.000000000000000000 ) ) ;
#40148 = ORIENTED_EDGE ( 'NONE', *, *, #77901, .F. ) ;
#40149 = AXIS2_PLACEMENT_3D ( 'NONE', #18798, #27984, #69178 ) ;
#40150 = AXIS2_PLACEMENT_3D ( 'NONE', #31781, #80239, #122734 ) ;
#40152 = EDGE_CURVE ( 'NONE', #83642, #44247, #48678, .T. ) ;
#40151 = DIRECTION ( 'NONE',  ( -0.000000000000000000, -1.000000000000000000, -0.000000000000000000 ) ) ;
#40153 = ORIENTED_EDGE ( 'NONE', *, *, #121130, .T. ) ;
#40154 = CONICAL_SURFACE ( 'NONE', #123742, 0.09999999999999999167, 0.003490658503988666988 ) ;
#40155 = EDGE_CURVE ( 'NONE', #43896, #46586, #122892, .T. ) ;
#40156 = ORIENTED_EDGE ( 'NONE', *, *, #73844, .T. ) ;
#40157 = AXIS2_PLACEMENT_3D ( 'NONE', #3010, #23276, #63209 ) ;
#40158 = EDGE_LOOP ( 'NONE', ( #36301, #118478, #43591, #114253 ) ) ;
#40159 = DIRECTION ( 'NONE',  ( 0.000000000000000000, 0.000000000000000000, 1.000000000000000000 ) ) ;
#40160 = EDGE_LOOP ( 'NONE', ( #81837, #92328 ) ) ;
#40161 = ORIENTED_EDGE ( 'NONE', *, *, #87238, .F. ) ;
#40162 = AXIS2_PLACEMENT_3D ( 'NONE', #83214, #941, #40894 ) ;
#40163 = CARTESIAN_POINT ( 'NONE',  ( -11.64999999999999680, 12.50000000000000000, 2.857883832488649301 ) ) ;
#40164 = AXIS2_PLACEMENT_3D ( 'NONE', #33501, #123774, #92389 ) ;
#40165 = DIRECTION ( 'NONE',  ( 0.000000000000000000, 0.000000000000000000, -1.000000000000000000 ) ) ;
#40166 = DIRECTION ( 'NONE',  ( 0.000000000000000000, 0.000000000000000000, -1.000000000000000000 ) ) ;
#40167 = DIRECTION ( 'NONE',  ( 0.000000000000000000, 0.000000000000000000, -1.000000000000000000 ) ) ;
#40168 = AXIS2_PLACEMENT_3D ( 'NONE', #30927, #117992, #78746 ) ;
#40169 = AXIS2_PLACEMENT_3D ( 'NONE', #113393, #84583, #54472 ) ;
#40170 = VECTOR ( 'NONE', #115947, 1000.000000000000000 ) ;
#40171 = DIRECTION ( 'NONE',  ( 0.000000000000000000, 0.000000000000000000, 1.000000000000000000 ) ) ;
#40172 = CIRCLE ( 'NONE', #100775, 0.06509327318403745899 ) ;
#40173 = VERTEX_POINT ( 'NONE', #81370 ) ;
#40174 = DIRECTION ( 'NONE',  ( 0.000000000000000000, -0.000000000000000000, 1.000000000000000000 ) ) ;
#40175 = VERTEX_POINT ( 'NONE', #29676 ) ;
#40176 = FACE_OUTER_BOUND ( 'NONE', #58547, .T. ) ;
#40177 = VERTEX_POINT ( 'NONE', #121279 ) ;
#40178 = CARTESIAN_POINT ( 'NONE',  ( 112.9918852365773603, 8.695328135426091620, 0.3304444235703573596 ) ) ;
#40179 = CIRCLE ( 'NONE', #56866, 0.06509327318403745899 ) ;
#40180 = CARTESIAN_POINT ( 'NONE',  ( -9.400000000000007461, 2.500000000000000000, 4.776537180435972196 ) ) ;
#40181 = ORIENTED_EDGE ( 'NONE', *, *, #109575, .F. ) ;
#40182 = CARTESIAN_POINT ( 'NONE',  ( 108.0000000000000142, 9.000000000000001776, 0.000000000000000000 ) ) ;
#40183 = DIRECTION ( 'NONE',  ( 0.000000000000000000, 1.000000000000000000, 0.000000000000000000 ) ) ;
#40184 = ORIENTED_EDGE ( 'NONE', *, *, #120226, .F. ) ;
#40185 = CARTESIAN_POINT ( 'NONE',  ( 15.59999999999988951, 12.50000000000000000, -0.3464101615137783474 ) ) ;
#40186 = EDGE_LOOP ( 'NONE', ( #7634, #20086, #42176, #36277 ) ) ;
#40187 = ORIENTED_EDGE ( 'NONE', *, *, #96341, .F. ) ;
#40188 = PLANE ( 'NONE',  #99896 ) ;
#40189 = FACE_OUTER_BOUND ( 'NONE', #96222, .T. ) ;
#40190 = CARTESIAN_POINT ( 'NONE',  ( 183.9635416670080872, -4.367472073101519747, 7.564683531249999149 ) ) ;
#40191 = CARTESIAN_POINT ( 'NONE',  ( -10.40000000000000213, 12.50000000000000000, 4.330127018922196314 ) ) ;
#40193 = EDGE_CURVE ( 'NONE', #125178, #75848, #41433, .T. ) ;
#40192 = CARTESIAN_POINT ( 'NONE',  ( -1.650000000000035660, 2.500000000000000000, 7.188010851410848723 ) ) ;
#40194 = ORIENTED_EDGE ( 'NONE', *, *, #68310, .T. ) ;
#40195 = CARTESIAN_POINT ( 'NONE',  ( 12.89999999999989910, 2.500000000000000000, 0.7928203230275495672 ) ) ;
#40196 = AXIS2_PLACEMENT_3D ( 'NONE', #54714, #92065, #63259 ) ;
#40197 = AXIS2_PLACEMENT_3D ( 'NONE', #109996, #109343, #110632 ) ;
#40198 = CIRCLE ( 'NONE', #113335, 5.000000000000000000 ) ;
#40199 = ORIENTED_EDGE ( 'NONE', *, *, #45858, .T. ) ;
#40200 = FACE_OUTER_BOUND ( 'NONE', #104715, .T. ) ;
#40201 = CARTESIAN_POINT ( 'NONE',  ( -8.150000000000009237, 2.500000000000000000, 6.841600689897072485 ) ) ;
#40202 = AXIS2_PLACEMENT_3D ( 'NONE', #122460, #114544, #51779 ) ;
#40203 = AXIS2_PLACEMENT_3D ( 'NONE', #117220, #23891, #27558 ) ;
#40204 = AXIS2_PLACEMENT_3D ( 'NONE', #95187, #45453, #55266 ) ;
#40205 = CIRCLE ( 'NONE', #56896, 0.1000000000000002554 ) ;
#40206 = CARTESIAN_POINT ( 'NONE',  ( 186.7552083336747444, 6.551208109652275624, -3.782341765624998686 ) ) ;
#40207 = CARTESIAN_POINT ( 'NONE',  ( -14.79999999999998295, 12.50000000000000000, -0.3464101615137760715 ) ) ;
#40208 = LINE ( 'NONE', #58564, #96630 ) ;
#40209 = FACE_OUTER_BOUND ( 'NONE', #106913, .T. ) ;
#40210 = LINE ( 'NONE', #87988, #97701 ) ;
#40211 = VERTEX_POINT ( 'NONE', #8718 ) ;
#40212 = VECTOR ( 'NONE', #100686, 1000.000000000000000 ) ;
#40213 = CARTESIAN_POINT ( 'NONE',  ( -11.24999999999999822, 2.500000000000000000, 5.902370205355745192 ) ) ;
#40214 = DIRECTION ( 'NONE',  ( 0.000000000000000000, 0.000000000000000000, -1.000000000000000000 ) ) ;
#40215 = CARTESIAN_POINT ( 'NONE',  ( 1.322875655532295136, -1.500000000000000222, 6.000000000000005329 ) ) ;
#40216 = ORIENTED_EDGE ( 'NONE', *, *, #5794, .F. ) ;
#40217 = DIRECTION ( 'NONE',  ( 0.000000000000000000, 0.000000000000000000, 1.000000000000000000 ) ) ;
#40218 = ORIENTED_EDGE ( 'NONE', *, *, #99982, .F. ) ;
#40219 = ORIENTED_EDGE ( 'NONE', *, *, #26190, .F. ) ;
#40220 = CARTESIAN_POINT ( 'NONE',  ( 8.949999999999921130, 2.500000000000000000, 1.918653347947321564 ) ) ;
#40221 = ORIENTED_EDGE ( 'NONE', *, *, #25814, .F. ) ;
#40222 = DIRECTION ( 'NONE',  ( 0.000000000000000000, 0.000000000000000000, -1.000000000000000000 ) ) ;
#40223 = CARTESIAN_POINT ( 'NONE',  ( 4.599999999999937472, 2.500000000000000000, 0.7928203230275495672 ) ) ;
#40224 = CIRCLE ( 'NONE', #105046, 0.06509327318403745899 ) ;
#40225 = VERTEX_POINT ( 'NONE', #80721 ) ;
#40226 = EDGE_CURVE ( 'NONE', #20798, #42905, #1493, .T. ) ;
#40227 = DIRECTION ( 'NONE',  ( 0.000000000000000000, -0.000000000000000000, 1.000000000000000000 ) ) ;
#40228 = CARTESIAN_POINT ( 'NONE',  ( -9.350000000000006750, 2.500000000000000000, 1.918653347947321564 ) ) ;
#40229 = DIRECTION ( 'NONE',  ( -0.000000000000000000, -1.000000000000000000, -0.000000000000000000 ) ) ;
#40230 = ADVANCED_FACE ( 'NONE', ( #128551 ), #71523, .T. ) ;
#40231 = AXIS2_PLACEMENT_3D ( 'NONE', #110255, #123141, #83221 ) ;
#40232 = EDGE_CURVE ( 'NONE', #21808, #115792, #104104, .T. ) ;
#40233 = ORIENTED_EDGE ( 'NONE', *, *, #48962, .F. ) ;
#40234 = AXIS2_PLACEMENT_3D ( 'NONE', #61784, #72249, #44715 ) ;
#40235 = ORIENTED_EDGE ( 'NONE', *, *, #57877, .F. ) ;
#40236 = ORIENTED_EDGE ( 'NONE', *, *, #34029, .T. ) ;
#40237 = DIRECTION ( 'NONE',  ( 0.000000000000000000, 0.000000000000000000, 1.000000000000000000 ) ) ;
#40238 = CARTESIAN_POINT ( 'NONE',  ( 183.9062500006828031, -8.891194145520236347, -1.633285867636356299E-15 ) ) ;
#40239 = EDGE_CURVE ( 'NONE', #19953, #40728, #108863, .T. ) ;
#40240 = EDGE_CURVE ( 'NONE', #128103, #79041, #119336, .T. ) ;
#40241 = FACE_OUTER_BOUND ( 'NONE', #86462, .T. ) ;
#40242 = EDGE_CURVE ( 'NONE', #2868, #110722, #58145, .T. ) ;
#40243 = FACE_BOUND ( 'NONE', #46332, .T. ) ;
#40245 = ADVANCED_FACE ( 'NONE', ( #39526 ), #109531, .T. ) ;
#40244 = ORIENTED_EDGE ( 'NONE', *, *, #98125, .T. ) ;
#40246 = EDGE_CURVE ( 'NONE', #23183, #6037, #33557, .T. ) ;
#40247 = CARTESIAN_POINT ( 'NONE',  ( 5.599999999999934808, 12.50000000000000000, -4.676537180435978769 ) ) ;
#40248 = DIRECTION ( 'NONE',  ( 0.000000000000000000, 1.000000000000000000, 0.000000000000000000 ) ) ;
#40249 = VECTOR ( 'NONE', #92888, 1000.000000000000000 ) ;
#40250 = EDGE_LOOP ( 'NONE', ( #2402, #49653, #89383, #78339 ) ) ;
#40251 = CONICAL_SURFACE ( 'NONE', #115524, 0.1000000000000002554, 0.003490658503988666988 ) ;
#40252 = DIRECTION ( 'NONE',  ( 1.000000000000000000, -0.000000000000000000, -0.000000000000000000 ) ) ;
#40253 = CARTESIAN_POINT ( 'NONE',  ( 13.54999999999989768, 12.50000000000000000, -2.511473670974877948 ) ) ;
#40254 = CONICAL_SURFACE ( 'NONE', #71637, 0.1000000000000002554, 0.003490658503988666988 ) ;
#40255 = AXIS2_PLACEMENT_3D ( 'NONE', #11814, #59668, #71366 ) ;
#40256 = AXIS2_PLACEMENT_3D ( 'NONE', #51729, #13709, #101469 ) ;
#40257 = LINE ( 'NONE', #108961, #79980 ) ;
#40258 = CARTESIAN_POINT ( 'NONE',  ( 9.799999999999915445, 12.50000000000000000, 4.048810130592458201 ) ) ;
#40259 = CARTESIAN_POINT ( 'NONE',  ( 10.64999999999991331, 2.500000000000000000, 6.741600689897071952 ) ) ;
#40260 = ADVANCED_FACE ( 'NONE', ( #52538 ), #14200, .T. ) ;
#40261 = CARTESIAN_POINT ( 'NONE',  ( -13.09999999999999076, 2.500000000000000000, 4.576537180435972019 ) ) ;
#40262 = CONICAL_SURFACE ( 'NONE', #77889, 0.09999999999999982514, 0.003490658503988666988 ) ;
#40263 = DIRECTION ( 'NONE',  ( 0.000000000000000000, 1.000000000000000000, 0.000000000000000000 ) ) ;
#40264 = VERTEX_POINT ( 'NONE', #34851 ) ;
#40265 = AXIS2_PLACEMENT_3D ( 'NONE', #3875, #34658, #24170 ) ;
#40266 = VERTEX_POINT ( 'NONE', #114039 ) ;
#40267 = ORIENTED_EDGE ( 'NONE', *, *, #46600, .F. ) ;
#40268 = EDGE_LOOP ( 'NONE', ( #19776, #91056, #84646, #108472 ) ) ;
#40269 = CARTESIAN_POINT ( 'NONE',  ( 6.649999999999928413, 2.500000000000000000, 2.757883832488649656 ) ) ;
#40270 = CARTESIAN_POINT ( 'NONE',  ( 8.749999999999953815, 2.500000000000000000, 6.495190528383297135 ) ) ;
#40271 = EDGE_LOOP ( 'NONE', ( #42473, #50890, #104009, #36338 ) ) ;
#40272 = FACE_BOUND ( 'NONE', #106643, .T. ) ;
#40273 = DIRECTION ( 'NONE',  ( 0.000000000000000000, -0.9999939076577903929, 0.003490651415223739937 ) ) ;
#40274 = DIRECTION ( 'NONE',  ( 0.000000000000000000, 0.000000000000000000, -1.000000000000000000 ) ) ;
#40275 = CARTESIAN_POINT ( 'NONE',  ( -1.050000000000038236, 12.50000000000000000, -6.148780366869526226 ) ) ;
#40276 = CARTESIAN_POINT ( 'NONE',  ( 11.04999999999990834, 12.50000000000000000, -6.841600689897077814 ) ) ;
#40277 = CARTESIAN_POINT ( 'NONE',  ( -8.550000000000011369, 12.50000000000000000, 1.818653347947321475 ) ) ;
#40278 = DIRECTION ( 'NONE',  ( 0.000000000000000000, 0.000000000000000000, 1.000000000000000000 ) ) ;
#40279 = AXIS2_PLACEMENT_3D ( 'NONE', #64323, #44046, #123875 ) ;
#40280 = CARTESIAN_POINT ( 'NONE',  ( 3.749999999999975131, 2.500000000000000000, 6.495190528383297135 ) ) ;
#40281 = ORIENTED_EDGE ( 'NONE', *, *, #19491, .F. ) ;
#40282 = ORIENTED_EDGE ( 'NONE', *, *, #102585, .F. ) ;
#40283 = ORIENTED_EDGE ( 'NONE', *, *, #71727, .T. ) ;
#40284 = EDGE_LOOP ( 'NONE', ( #61722, #201, #51639, #127305 ) ) ;
#40285 = ORIENTED_EDGE ( 'NONE', *, *, #60858, .T. ) ;
#40286 = CONICAL_SURFACE ( 'NONE', #88276, 0.1000000000000002554, 0.003490658503988666988 ) ;
#40287 = ORIENTED_EDGE ( 'NONE', *, *, #114150, .T. ) ;
#40288 = AXIS2_PLACEMENT_3D ( 'NONE', #31443, #92942, #54291 ) ;
#40290 = EDGE_CURVE ( 'NONE', #40089, #2945, #53197, .T. ) ;
#40289 = AXIS2_PLACEMENT_3D ( 'NONE', #46433, #90057, #66076 ) ;
#40291 = CARTESIAN_POINT ( 'NONE',  ( -5.650000000000019895, 2.500000000000000000, 6.941600689897073018 ) ) ;
#40292 = CARTESIAN_POINT ( 'NONE',  ( -5.850000000000018296, 12.50000000000000000, 7.122917578226811486 ) ) ;
#40293 = EDGE_CURVE ( 'NONE', #102428, #45275, #5878, .T. ) ;
#40294 = VERTEX_POINT ( 'NONE', #2789 ) ;
#40295 = DIRECTION ( 'NONE',  ( 0.000000000000000000, 1.000000000000000000, 0.000000000000000000 ) ) ;
#40296 = ADVANCED_FACE ( 'NONE', ( #62372 ), #95782, .T. ) ;
#40297 = AXIS2_PLACEMENT_3D ( 'NONE', #73838, #83666, #71251 ) ;
#40298 = ADVANCED_FACE ( 'NONE', ( #81989 ), #94382, .T. ) ;
#40299 = AXIS2_PLACEMENT_3D ( 'NONE', #14723, #54652, #85419 ) ;
#40300 = CARTESIAN_POINT ( 'NONE',  ( 1.849999999999950129, 2.500000000000000000, -6.841600689897078702 ) ) ;
#40301 = CARTESIAN_POINT ( 'NONE',  ( 184.7343750003414016, 8.734944146203032389, 5.348610694689227483E-16 ) ) ;
#40302 = DIRECTION ( 'NONE',  ( 0.000000000000000000, 0.000000000000000000, -1.000000000000000000 ) ) ;
#40303 = CARTESIAN_POINT ( 'NONE',  ( -15.19999999999998153, 2.500000000000000000, -0.3464101615137759604 ) ) ;
#40304 = CIRCLE ( 'NONE', #109228, 0.06509327318403741736 ) ;
#40305 = CIRCLE ( 'NONE', #29833, 0.06509327318403745899 ) ;
#40306 = EDGE_CURVE ( 'NONE', #85331, #79392, #43476, .T. ) ;
#40307 = ORIENTED_EDGE ( 'NONE', *, *, #50024, .F. ) ;
#40308 = DIRECTION ( 'NONE',  ( -0.000000000000000000, -1.000000000000000000, -0.000000000000000000 ) ) ;
#40309 = AXIS2_PLACEMENT_3D ( 'NONE', #101839, #122769, #71736 ) ;
#40310 = ADVANCED_FACE ( 'NONE', ( #32282 ), #127102, .T. ) ;
#40311 = EDGE_CURVE ( 'NONE', #36380, #54095, #117824, .T. ) ;
#40312 = ORIENTED_EDGE ( 'NONE', *, *, #22047, .T. ) ;
#40313 = EDGE_CURVE ( 'NONE', #98576, #91821, #93119, .T. ) ;
#40314 = EDGE_LOOP ( 'NONE', ( #163, #72333, #15045, #21408 ) ) ;
#40315 = FACE_OUTER_BOUND ( 'NONE', #75588, .T. ) ;
#40316 = DIRECTION ( 'NONE',  ( 0.000000000000000000, -0.9999939076577903929, 0.003490651415223739937 ) ) ;
#40317 = DIRECTION ( 'NONE',  ( -0.000000000000000000, -1.000000000000000000, -0.000000000000000000 ) ) ;
#40318 = ORIENTED_EDGE ( 'NONE', *, *, #40313, .T. ) ;
#40319 = EDGE_CURVE ( 'NONE', #60096, #37015, #91819, .T. ) ;
#40320 = VERTEX_POINT ( 'NONE', #23731 ) ;
#40321 = CONICAL_SURFACE ( 'NONE', #102988, 0.1000000000000000472, 0.003490658503988666988 ) ;
#40322 = DIRECTION ( 'NONE',  ( 0.000000000000000000, 0.000000000000000000, 1.000000000000000000 ) ) ;
#40323 = DIRECTION ( 'NONE',  ( 0.000000000000000000, 0.000000000000000000, 1.000000000000000000 ) ) ;
#40324 = FACE_OUTER_BOUND ( 'NONE', #127264, .T. ) ;
#40325 = FACE_OUTER_BOUND ( 'NONE', #59859, .T. ) ;
#40326 = ORIENTED_EDGE ( 'NONE', *, *, #117363, .F. ) ;
#40327 = DIRECTION ( 'NONE',  ( 0.000000000000000000, 1.000000000000000000, 0.000000000000000000 ) ) ;
#40329 = ORIENTED_EDGE ( 'NONE', *, *, #84151, .F. ) ;
#40328 = AXIS2_PLACEMENT_3D ( 'NONE', #36836, #46645, #99464 ) ;
#40330 = PLANE ( 'NONE',  #116759 ) ;
#40331 = AXIS2_PLACEMENT_3D ( 'NONE', #76311, #126702, #37033 ) ;
#40332 = CONICAL_SURFACE ( 'NONE', #115508, 0.09999999999999999167, 0.003490658503988666988 ) ;
#40333 = ORIENTED_EDGE ( 'NONE', *, *, #43516, .T. ) ;
#40334 = DIRECTION ( 'NONE',  ( -0.000000000000000000, 1.000000000000000000, -0.000000000000000000 ) ) ;
#40335 = DIRECTION ( 'NONE',  ( 0.000000000000000000, 1.000000000000000000, 0.000000000000000000 ) ) ;
#40336 = FACE_OUTER_BOUND ( 'NONE', #122515, .T. ) ;
#40337 = EDGE_CURVE ( 'NONE', #67756, #95287, #64715, .T. ) ;
#40339 = AXIS2_PLACEMENT_3D ( 'NONE', #87710, #96238, #26870 ) ;
#40338 = DIRECTION ( 'NONE',  ( 0.000000000000000000, 1.000000000000000000, 0.000000000000000000 ) ) ;
#40340 = ORIENTED_EDGE ( 'NONE', *, *, #84111, .F. ) ;
#40341 = COLOUR_RGB ( '', 0.40784314, 0.44705882, 0.49803922) ;
#40342 = AXIS2_PLACEMENT_3D ( 'NONE', #56369, #17056, #126410 ) ;
#40343 = CARTESIAN_POINT ( 'NONE',  ( 7.899999999999924860, 2.500000000000000000, 4.230127018922196669 ) ) ;
#40344 = AXIS2_PLACEMENT_3D ( 'NONE', #17808, #97667, #77388 ) ;
#40345 = CARTESIAN_POINT ( 'NONE',  ( 17.50000000000000000, -2.500000000000000000, 4.000000000000001776 ) ) ;
#40346 = ORIENTED_EDGE ( 'NONE', *, *, #18456, .T. ) ;
#40347 = ORIENTED_EDGE ( 'NONE', *, *, #32351, .T. ) ;
#40348 = ORIENTED_EDGE ( 'NONE', *, *, #111197, .F. ) ;
#40349 = CARTESIAN_POINT ( 'NONE',  ( -5.850000000000019185, 12.50000000000000000, 2.165063509461097713 ) ) ;
#40350 = DIRECTION ( 'NONE',  ( 0.000000000000000000, 0.000000000000000000, 1.000000000000000000 ) ) ;
#40351 = LINE ( 'NONE', #39723, #21907 ) ;
#40352 = CARTESIAN_POINT ( 'NONE',  ( 187.1510416670080303, 4.367472073101518859, -7.564683531249999149 ) ) ;
#40353 = CIRCLE ( 'NONE', #73773, 0.06509327318403745899 ) ;
#40354 = DIRECTION ( 'NONE',  ( 0.000000000000000000, 1.000000000000000000, 0.000000000000000000 ) ) ;
#40355 = LINE ( 'NONE', #1689, #571 ) ;
#40356 = CIRCLE ( 'NONE', #96466, 0.06509327318403745899 ) ;
#40358 = EDGE_CURVE ( 'NONE', #88083, #20150, #85648, .T. ) ;
#40357 = CARTESIAN_POINT ( 'NONE',  ( -1.850000000000033840, 12.50000000000000000, 2.576566944158910744 ) ) ;
#40359 = CONICAL_SURFACE ( 'NONE', #52863, 0.1000000000000000056, 0.003490658503988666988 ) ;
#40360 = CARTESIAN_POINT ( 'NONE',  ( -11.84999999999999609, 2.500000000000000000, 6.841600689897072485 ) ) ;
#40361 = VECTOR ( 'NONE', #48369, 1000.000000000000000 ) ;
#40362 = CIRCLE ( 'NONE', #44449, 0.1000000000000002554 ) ;
#40363 = DIRECTION ( 'NONE',  ( 0.000000000000000000, 1.000000000000000000, 0.000000000000000000 ) ) ;
#40364 = VECTOR ( 'NONE', #56653, 1000.000000000000000 ) ;
#40365 = ORIENTED_EDGE ( 'NONE', *, *, #98264, .T. ) ;
#40366 = FACE_OUTER_BOUND ( 'NONE', #68629, .T. ) ;
#40367 = EDGE_CURVE ( 'NONE', #103425, #21203, #127514, .T. ) ;
#40368 = CARTESIAN_POINT ( 'NONE',  ( 9.349999999999919709, 12.50000000000000000, 2.511473670974873507 ) ) ;
#40369 = FACE_OUTER_BOUND ( 'NONE', #17785, .T. ) ;
#40370 = CARTESIAN_POINT ( 'NONE',  ( -2.900000000000029665, 2.500000000000000000, 3.637306695894644726 ) ) ;
#40371 = CARTESIAN_POINT ( 'NONE',  ( -1.650000000000035660, 12.50000000000000000, 7.253104124594885960 ) ) ;
#40372 = VERTEX_POINT ( 'NONE', #104210 ) ;
#40373 = CARTESIAN_POINT ( 'NONE',  ( -7.700000000000014388, 12.50000000000000000, -0.4115034346978156399 ) ) ;
#40374 = FACE_OUTER_BOUND ( 'NONE', #104155, .T. ) ;
#40376 = ORIENTED_EDGE ( 'NONE', *, *, #78366, .T. ) ;
#40375 = DIRECTION ( 'NONE',  ( -4.274815082592931898E-19, -0.9999939076577903929, -0.003490651415223739937 ) ) ;
#40377 = CIRCLE ( 'NONE', #113517, 0.1000000000000000472 ) ;
#40378 = AXIS2_PLACEMENT_3D ( 'NONE', #120371, #81715, #121640 ) ;
#40379 = VERTEX_POINT ( 'NONE', #84574 ) ;
#40380 = LINE ( 'NONE', #60028, #111616 ) ;
#40381 = CIRCLE ( 'NONE', #88677, 0.1000000000000002554 ) ;
#40382 = EDGE_LOOP ( 'NONE', ( #38615, #84162 ) ) ;
#40383 = AXIS2_PLACEMENT_3D ( 'NONE', #109969, #20291, #100151 ) ;
#40384 = ORIENTED_EDGE ( 'NONE', *, *, #8458, .T. ) ;
#40385 = CARTESIAN_POINT ( 'NONE',  ( 6.449999999999933564, 12.50000000000000000, -6.906693963081115939 ) ) ;
#40386 = AXIS2_PLACEMENT_3D ( 'NONE', #77780, #18869, #118361 ) ;
#40387 = AXIS2_PLACEMENT_3D ( 'NONE', #57237, #48722, #29711 ) ;
#40388 = CARTESIAN_POINT ( 'NONE',  ( 19.08853762629022199, 0.5565172524007554467, -4.470057054643568506 ) ) ;
#40389 = DIRECTION ( 'NONE',  ( -0.000000000000000000, -1.000000000000000000, -0.000000000000000000 ) ) ;
#40390 = DIRECTION ( 'NONE',  ( 1.000000000000000000, -0.000000000000000000, -0.000000000000000000 ) ) ;
#40392 = EDGE_LOOP ( 'NONE', ( #36859, #94790 ) ) ;
#40391 = AXIS2_PLACEMENT_3D ( 'NONE', #120533, #53082, #1390 ) ;
#40393 = AXIS2_PLACEMENT_3D ( 'NONE', #99285, #89455, #107808 ) ;
#40395 = EDGE_CURVE ( 'NONE', #110679, #109560, #54463, .T. ) ;
#40394 = CIRCLE ( 'NONE', #65500, 0.1000000000000002554 ) ;
#40396 = DIRECTION ( 'NONE',  ( -0.000000000000000000, 1.000000000000000000, -0.000000000000000000 ) ) ;
#40398 = EDGE_LOOP ( 'NONE', ( #69341, #59129, #106683, #67230 ) ) ;
#40397 = AXIS2_PLACEMENT_3D ( 'NONE', #44314, #15490, #86153 ) ;
#40399 = PLANE ( 'NONE',  #95670 ) ;
#40400 = CIRCLE ( 'NONE', #71781, 0.06509327318403745899 ) ;
#40401 = CARTESIAN_POINT ( 'NONE',  ( -12.09999999999999609, 2.500000000000000000, 0.6928203230275535862 ) ) ;
#40402 = CARTESIAN_POINT ( 'NONE',  ( 7.049999999999928768, 2.500000000000000000, -2.065063509461102065 ) ) ;
#40403 = EDGE_CURVE ( 'NONE', #127796, #91980, #124512, .T. ) ;
#40404 = ORIENTED_EDGE ( 'NONE', *, *, #48811, .T. ) ;
#40405 = ORIENTED_EDGE ( 'NONE', *, *, #42404, .T. ) ;
#40406 = ORIENTED_EDGE ( 'NONE', *, *, #124911, .T. ) ;
#40407 = ORIENTED_EDGE ( 'NONE', *, *, #40786, .T. ) ;
#40408 = ORIENTED_EDGE ( 'NONE', *, *, #128325, .F. ) ;
#40409 = CARTESIAN_POINT ( 'NONE',  ( -2.000000000000000000, 2.449293598294706414E-16, 6.000000000000005329 ) ) ;
#40410 = CARTESIAN_POINT ( 'NONE',  ( 16.56576425165006583, 2.500000000000000000, 6.084390597445811899 ) ) ;
#40411 = EDGE_CURVE ( 'NONE', #123530, #32792, #52205, .T. ) ;
#40412 = EDGE_CURVE ( 'NONE', #95641, #31177, #106147, .T. ) ;
#40413 = LINE ( 'NONE', #128802, #60817 ) ;
#40414 = EDGE_CURVE ( 'NONE', #13317, #3943, #68921, .T. ) ;
#40415 = FACE_BOUND ( 'NONE', #20335, .T. ) ;
#40416 = EDGE_CURVE ( 'NONE', #13662, #7603, #96311, .T. ) ;
#40417 = CARTESIAN_POINT ( 'NONE',  ( -3.550000000000027356, 2.500000000000000000, -2.511473670974877948 ) ) ;
#40418 = CARTESIAN_POINT ( 'NONE',  ( 8.949999999999917577, 2.500000000000000000, 6.148780366869520009 ) ) ;
#40419 = DIRECTION ( 'NONE',  ( -0.000000000000000000, 1.000000000000000000, -0.000000000000000000 ) ) ;
#40420 = CARTESIAN_POINT ( 'NONE',  ( -10.84999999999999964, 2.500000000000000000, 7.288010851410849256 ) ) ;
#40421 = AXIS2_PLACEMENT_3D ( 'NONE', #58432, #9960, #40070 ) ;
#40422 = DIRECTION ( 'NONE',  ( 0.000000000000000000, 0.000000000000000000, -1.000000000000000000 ) ) ;
#40423 = DIRECTION ( 'NONE',  ( -0.000000000000000000, -1.000000000000000000, -0.000000000000000000 ) ) ;
#40424 = EDGE_CURVE ( 'NONE', #3575, #12586, #12485, .T. ) ;
#40425 = LINE ( 'NONE', #118316, #61729 ) ;
#40426 = CONICAL_SURFACE ( 'NONE', #113566, 0.09999999999999982514, 0.003490658503988666988 ) ;
#40428 = ADVANCED_FACE ( 'NONE', ( #125761 ), #110773, .T. ) ;
#40427 = AXIS2_PLACEMENT_3D ( 'NONE', #26418, #66323, #4814 ) ;
#40429 = CIRCLE ( 'NONE', #98989, 0.06509327318403745899 ) ;
#40430 = EDGE_CURVE ( 'NONE', #27399, #66014, #54345, .T. ) ;
#40431 = FACE_OUTER_BOUND ( 'NONE', #113421, .T. ) ;
#40432 = ORIENTED_EDGE ( 'NONE', *, *, #95730, .F. ) ;
#40433 = ORIENTED_EDGE ( 'NONE', *, *, #77516, .T. ) ;
#40434 = EDGE_LOOP ( 'NONE', ( #92150, #110221, #27652, #34043 ) ) ;
#40435 = EDGE_LOOP ( 'NONE', ( #104110, #62196 ) ) ;
#40436 = DIRECTION ( 'NONE',  ( -0.000000000000000000, 1.000000000000000000, -0.000000000000000000 ) ) ;
#40437 = CARTESIAN_POINT ( 'NONE',  ( 9.349999999999916156, 12.50000000000000000, 6.083687093685482772 ) ) ;
#40438 = FACE_BOUND ( 'NONE', #27448, .T. ) ;
#40439 = AXIS2_PLACEMENT_3D ( 'NONE', #3221, #52312, #21564 ) ;
#40440 = CIRCLE ( 'NONE', #59219, 0.1000000000000000472 ) ;
#40441 = DIRECTION ( 'NONE',  ( 0.000000000000000000, 0.000000000000000000, 1.000000000000000000 ) ) ;
#40442 = CONICAL_SURFACE ( 'NONE', #113585, 0.1000000000000002554, 0.003490658503988666988 ) ;
#40443 = VERTEX_POINT ( 'NONE', #95691 ) ;
#40444 = CARTESIAN_POINT ( 'NONE',  ( 11.89999999999990798, 2.500000000000000000, -4.676537180435977881 ) ) ;
#40445 = DIRECTION ( 'NONE',  ( 0.000000000000000000, 0.000000000000000000, -1.000000000000000000 ) ) ;
#40446 = DIRECTION ( 'NONE',  ( -0.000000000000000000, 1.000000000000000000, -0.000000000000000000 ) ) ;
#40447 = DIRECTION ( 'NONE',  ( 0.000000000000000000, 1.000000000000000000, 0.000000000000000000 ) ) ;
#40448 = ORIENTED_EDGE ( 'NONE', *, *, #53814, .F. ) ;
#40449 = DIRECTION ( 'NONE',  ( 0.000000000000000000, 0.000000000000000000, 1.000000000000000000 ) ) ;
#40450 = AXIS2_PLACEMENT_3D ( 'NONE', #32375, #43465, #72279 ) ;
#40451 = AXIS2_PLACEMENT_3D ( 'NONE', #55937, #105028, #114847 ) ;
#40452 = AXIS2_PLACEMENT_3D ( 'NONE', #19517, #59482, #129510 ) ;
#40453 = VERTEX_POINT ( 'NONE', #57030 ) ;
#40454 = VERTEX_POINT ( 'NONE', #117225 ) ;
#40455 = DIRECTION ( 'NONE',  ( 0.000000000000000000, 0.000000000000000000, 1.000000000000000000 ) ) ;
#40456 = DIRECTION ( 'NONE',  ( 0.000000000000000000, 0.000000000000000000, -1.000000000000000000 ) ) ;
#40457 = VECTOR ( 'NONE', #90647, 1000.000000000000000 ) ;
#40458 = ORIENTED_EDGE ( 'NONE', *, *, #89171, .F. ) ;
#40459 = DIRECTION ( 'NONE',  ( 0.000000000000000000, 0.000000000000000000, -1.000000000000000000 ) ) ;
#40460 = DIRECTION ( 'NONE',  ( 0.000000000000000000, 0.000000000000000000, 1.000000000000000000 ) ) ;
#40461 = PLANE ( 'NONE',  #72440 ) ;
#40462 = VERTEX_POINT ( 'NONE', #36124 ) ;
#40463 = DIRECTION ( 'NONE',  ( 0.000000000000000000, 1.000000000000000000, 0.000000000000000000 ) ) ;
#40464 = EDGE_CURVE ( 'NONE', #7910, #8844, #66854, .T. ) ;
#40465 = VERTEX_POINT ( 'NONE', #15819 ) ;
#40466 = CARTESIAN_POINT ( 'NONE',  ( -7.900000000000014566, 12.50000000000000000, -5.022947341949754119 ) ) ;
#40467 = EDGE_CURVE ( 'NONE', #125626, #7881, #127088, .T. ) ;
#40468 = EDGE_LOOP ( 'NONE', ( #27635, #113269 ) ) ;
#40470 = EDGE_CURVE ( 'NONE', #70629, #96127, #100328, .T. ) ;
#40469 = DIRECTION ( 'NONE',  ( -0.000000000000000000, 1.000000000000000000, -0.000000000000000000 ) ) ;
#40471 = ORIENTED_EDGE ( 'NONE', *, *, #114967, .F. ) ;
#40472 = CARTESIAN_POINT ( 'NONE',  ( -11.64999999999999680, 2.500000000000000000, -7.188010851410850499 ) ) ;
#40473 = DIRECTION ( 'NONE',  ( 0.000000000000000000, -0.000000000000000000, 1.000000000000000000 ) ) ;
#40474 = AXIS2_PLACEMENT_3D ( 'NONE', #103423, #34035, #32773 ) ;
#40475 = DIRECTION ( 'NONE',  ( 0.000000000000000000, 0.000000000000000000, 1.000000000000000000 ) ) ;
#40476 = CONICAL_SURFACE ( 'NONE', #94733, 0.1000000000000002554, 0.003490658503988666988 ) ;
#40477 = DIRECTION ( 'NONE',  ( 0.000000000000000000, 0.000000000000000000, 1.000000000000000000 ) ) ;
#40478 = CARTESIAN_POINT ( 'NONE',  ( 12.69999999999990337, 12.50000000000000000, -4.676537180435978769 ) ) ;
#40479 = ORIENTED_EDGE ( 'NONE', *, *, #98224, .F. ) ;
#40480 = ADVANCED_FACE ( 'NONE', ( #96963 ), #56396, .T. ) ;
#40481 = EDGE_LOOP ( 'NONE', ( #86819, #684, #94763, #28276 ) ) ;
#40482 = ORIENTED_EDGE ( 'NONE', *, *, #99721, .T. ) ;
#40483 = CARTESIAN_POINT ( 'NONE',  ( -9.400000000000007461, 12.50000000000000000, -0.4115034346978157509 ) ) ;
#40484 = CIRCLE ( 'NONE', #17356, 0.06509327318403745899 ) ;
#40485 = AXIS2_PLACEMENT_3D ( 'NONE', #19055, #59008, #21006 ) ;
#40486 = CARTESIAN_POINT ( 'NONE',  ( -5.450000000000023270, 2.500000000000000000, -6.595190528383302109 ) ) ;
#40487 = AXIS2_PLACEMENT_3D ( 'NONE', #113707, #103244, #1169 ) ;
#40489 = DIRECTION ( 'NONE',  ( 0.000000000000000000, 0.000000000000000000, 1.000000000000000000 ) ) ;
#40488 = AXIS2_PLACEMENT_3D ( 'NONE', #112145, #90559, #22496 ) ;
#40491 = VERTEX_POINT ( 'NONE', #26309 ) ;
#40490 = VERTEX_POINT ( 'NONE', #5357 ) ;
#40492 = ORIENTED_EDGE ( 'NONE', *, *, #64285, .T. ) ;
#40493 = FACE_OUTER_BOUND ( 'NONE', #55456, .T. ) ;
#40494 = VERTEX_POINT ( 'NONE', #67480 ) ;
#40495 = DIRECTION ( 'NONE',  ( 0.000000000000000000, 0.000000000000000000, -1.000000000000000000 ) ) ;
#40496 = CIRCLE ( 'NONE', #96893, 0.06509327318403745899 ) ;
#40497 = CIRCLE ( 'NONE', #65499, 0.06509327318403745899 ) ;
#40498 = AXIS2_PLACEMENT_3D ( 'NONE', #27050, #54554, #116065 ) ;
#40499 = CONTEXT_DEPENDENT_SHAPE_REPRESENTATION ( #86544, #104704 ) ;
#40500 = FACE_OUTER_BOUND ( 'NONE', #38226, .T. ) ;
#40501 = CARTESIAN_POINT ( 'NONE',  ( -6.900000000000019007, 2.500000000000000000, -3.883716857408426648 ) ) ;
#40502 = DIRECTION ( 'NONE',  ( 0.000000000000000000, 0.000000000000000000, 1.000000000000000000 ) ) ;
#40503 = CARTESIAN_POINT ( 'NONE',  ( 185.6666666666666856, -6.668395609140176816, -3.850000000000003642 ) ) ;
#40504 = CARTESIAN_POINT ( 'NONE',  ( 12.09999999999990550, 2.500000000000000000, -5.022947341949754119 ) ) ;
#40505 = ADVANCED_FACE ( 'NONE', ( #66210 ), #17751, .T. ) ;
#40506 = LINE ( 'NONE', #70584, #8095 ) ;
#40507 = VERTEX_POINT ( 'NONE', #127714 ) ;
#40508 = ORIENTED_EDGE ( 'NONE', *, *, #72059, .F. ) ;
#40509 = LINE ( 'NONE', #88267, #34074 ) ;
#40510 = CARTESIAN_POINT ( 'NONE',  ( 7.949999999999925571, 12.50000000000000000, 2.165063509461097713 ) ) ;
#40511 = ORIENTED_EDGE ( 'NONE', *, *, #55927, .F. ) ;
#40512 = EDGE_LOOP ( 'NONE', ( #30148, #67151 ) ) ;
#40513 = CARTESIAN_POINT ( 'NONE',  ( 186.4427083336747160, -6.551208109652278289, 3.782341765624995134 ) ) ;
#40514 = DIRECTION ( 'NONE',  ( 0.000000000000000000, 0.000000000000000000, 1.000000000000000000 ) ) ;
#40515 = CARTESIAN_POINT ( 'NONE',  ( 21.23528140090950700, 2.699413673072311948, 2.293764360948889802 ) ) ;
#40516 = CIRCLE ( 'NONE', #768, 0.06509327318403745899 ) ;
#40517 = CARTESIAN_POINT ( 'NONE',  ( -4.350000000000023626, 12.50000000000000000, -2.576566944158915184 ) ) ;
#40518 = CARTESIAN_POINT ( 'NONE',  ( -8.750000000000012434, 12.50000000000000000, -5.802370205355744659 ) ) ;
#40519 = EDGE_CURVE ( 'NONE', #66127, #107210, #77969, .T. ) ;
#40520 = CARTESIAN_POINT ( 'NONE',  ( 10.84999999999990905, 2.500000000000000000, -6.495190528383302464 ) ) ;
#40521 = DIRECTION ( 'NONE',  ( -0.000000000000000000, -1.000000000000000000, -0.000000000000000000 ) ) ;
#40522 = AXIS2_PLACEMENT_3D ( 'NONE', #4281, #93985, #125378 ) ;
#40524 = VECTOR ( 'NONE', #122524, 1000.000000000000000 ) ;
#40523 = FACE_OUTER_BOUND ( 'NONE', #49829, .T. ) ;
#40525 = ORIENTED_EDGE ( 'NONE', *, *, #121529, .F. ) ;
#40526 = CONICAL_SURFACE ( 'NONE', #48832, 0.09999999999999982514, 0.003490658503988666988 ) ;
#40527 = ORIENTED_EDGE ( 'NONE', *, *, #12243, .T. ) ;
#40528 = VERTEX_POINT ( 'NONE', #15158 ) ;
#40529 = EDGE_LOOP ( 'NONE', ( #58012, #96314 ) ) ;
#40531 = ORIENTED_EDGE ( 'NONE', *, *, #43252, .F. ) ;
#40530 = EDGE_CURVE ( 'NONE', #66994, #47269, #55118, .T. ) ;
#40532 = AXIS2_PLACEMENT_3D ( 'NONE', #111720, #82916, #42343 ) ;
#40533 = DIRECTION ( 'NONE',  ( 0.000000000000000000, 1.000000000000000000, 0.000000000000000000 ) ) ;
#40534 = CARTESIAN_POINT ( 'NONE',  ( -2.900000000000030109, 2.500000000000000000, 0.5928203230275495006 ) ) ;
#40535 = AXIS2_PLACEMENT_3D ( 'NONE', #38886, #96460, #46097 ) ;
#40536 = ORIENTED_EDGE ( 'NONE', *, *, #75814, .F. ) ;
#40537 = DIRECTION ( 'NONE',  ( -0.000000000000000000, 1.000000000000000000, -0.000000000000000000 ) ) ;
#40538 = AXIS2_PLACEMENT_3D ( 'NONE', #85438, #54669, #84793 ) ;
#40539 = DIRECTION ( 'NONE',  ( 0.000000000000000000, 0.000000000000000000, 1.000000000000000000 ) ) ;
#40540 = DIRECTION ( 'NONE',  ( 0.000000000000000000, 0.000000000000000000, 1.000000000000000000 ) ) ;
#40542 = VERTEX_POINT ( 'NONE', #35485 ) ;
#40541 = FACE_OUTER_BOUND ( 'NONE', #15625, .T. ) ;
#40543 = ADVANCED_FACE ( 'NONE', ( #75382 ), #48011, .T. ) ;
#40544 = CARTESIAN_POINT ( 'NONE',  ( 5.849999999999933920, 12.50000000000000000, -2.165063509461101710 ) ) ;
#40545 = CONICAL_SURFACE ( 'NONE', #4993, 0.09999999999999982514, 0.003490658503988666988 ) ;
#40546 = DIRECTION ( 'NONE',  ( 0.000000000000000000, -0.000000000000000000, 1.000000000000000000 ) ) ;
#40547 = ORIENTED_EDGE ( 'NONE', *, *, #30336, .F. ) ;
#40548 = VECTOR ( 'NONE', #20430, 1000.000000000000000 ) ;
#40549 = CONICAL_SURFACE ( 'NONE', #9129, 0.09999999999999999167, 0.003490658503988666988 ) ;
#40550 = CONICAL_SURFACE ( 'NONE', #111533, 0.1000000000000002554, 0.003490658503988666988 ) ;
#40551 = EDGE_LOOP ( 'NONE', ( #45051, #27452 ) ) ;
#40552 = ORIENTED_EDGE ( 'NONE', *, *, #41038, .T. ) ;
#40553 = ORIENTED_EDGE ( 'NONE', *, *, #32022, .T. ) ;
#40554 = CARTESIAN_POINT ( 'NONE',  ( -4.350000000000023626, 12.50000000000000000, 6.776507416713035248 ) ) ;
#40555 = LINE ( 'NONE', #100100, #75993 ) ;
#40556 = FACE_OUTER_BOUND ( 'NONE', #39469, .T. ) ;
#40557 = CIRCLE ( 'NONE', #28013, 0.1000000000000002554 ) ;
#40558 = EDGE_CURVE ( 'NONE', #41701, #87369, #45957, .T. ) ;
#40559 = DIRECTION ( 'NONE',  ( -4.274815082592931898E-19, -0.9999939076577903929, -0.003490651415223739937 ) ) ;
#40560 = VERTEX_POINT ( 'NONE', #49824 ) ;
#40561 = CARTESIAN_POINT ( 'NONE',  ( 12.09999999999990550, 2.500000000000000000, -4.922947341949753586 ) ) ;
#40562 = CARTESIAN_POINT ( 'NONE',  ( 17.37282530749035203, -0.4689596142739269613, -5.357821376857504703 ) ) ;
#40563 = CARTESIAN_POINT ( 'NONE',  ( 10.84999999999990905, 2.500000000000000000, 1.472243186433545459 ) ) ;
#40564 = CARTESIAN_POINT ( 'NONE',  ( -9.550000000000006040, 2.500000000000000000, 2.265063509461097357 ) ) ;
#40565 = EDGE_CURVE ( 'NONE', #16136, #12100, #129038, .T. ) ;
#40566 = EDGE_LOOP ( 'NONE', ( #121013, #54034 ) ) ;
#40567 = DIRECTION ( 'NONE',  ( 0.000000000000000000, 1.000000000000000000, 0.000000000000000000 ) ) ;
#40568 = VERTEX_POINT ( 'NONE', #10508 ) ;
#40569 = ORIENTED_EDGE ( 'NONE', *, *, #28365, .T. ) ;
#40571 = AXIS2_PLACEMENT_3D ( 'NONE', #82354, #3774, #94089 ) ;
#40570 = CARTESIAN_POINT ( 'NONE',  ( -9.400000000000007461, 2.500000000000000000, 4.776537180435972196 ) ) ;
#40572 = EDGE_CURVE ( 'NONE', #118390, #30572, #68143, .T. ) ;
#40573 = CIRCLE ( 'NONE', #69791, 0.06509327318403745899 ) ;
#40574 = EDGE_CURVE ( 'NONE', #46603, #6145, #119101, .T. ) ;
#40575 = FACE_OUTER_BOUND ( 'NONE', #54381, .T. ) ;
#40576 = EDGE_CURVE ( 'NONE', #100714, #39233, #86088, .T. ) ;
#40577 = FACE_BOUND ( 'NONE', #128426, .T. ) ;
#40578 = EDGE_CURVE ( 'NONE', #91444, #2822, #25014, .T. ) ;
#40579 = CARTESIAN_POINT ( 'NONE',  ( 12.04999999999990479, 12.50000000000000000, 2.165063509461097713 ) ) ;
#40580 = CARTESIAN_POINT ( 'NONE',  ( 3.349999999999941913, 2.500000000000000000, 6.495190528383297135 ) ) ;
#40581 = CARTESIAN_POINT ( 'NONE',  ( -0.2000000000000339284, 2.500000000000000000, -0.3464101615137759604 ) ) ;
#40582 = CONICAL_SURFACE ( 'NONE', #124176, 0.1000000000000002554, 0.003490658503988666988 ) ;
#40583 = AXIS2_PLACEMENT_3D ( 'NONE', #82720, #60504, #21865 ) ;
#40584 = CONICAL_SURFACE ( 'NONE', #55230, 0.09999999999999982514, 0.003490658503988666988 ) ;
#40585 = ADVANCED_FACE ( 'NONE', ( #18409 ), #98157, .T. ) ;
#40586 = DIRECTION ( 'NONE',  ( 0.000000000000000000, -0.000000000000000000, 1.000000000000000000 ) ) ;
#40587 = DIRECTION ( 'NONE',  ( 0.000000000000000000, 0.000000000000000000, -1.000000000000000000 ) ) ;
#40588 = EDGE_CURVE ( 'NONE', #92137, #105738, #125359, .T. ) ;
#40589 = CARTESIAN_POINT ( 'NONE',  ( 0.4499999999999569344, 2.500000000000000000, 2.265063509461097357 ) ) ;
#40590 = DIRECTION ( 'NONE',  ( 0.000000000000000000, -0.9999939076577903929, 0.003490651415223739937 ) ) ;
#40591 = ORIENTED_EDGE ( 'NONE', *, *, #46024, .T. ) ;
#40593 = DIRECTION ( 'NONE',  ( -0.000000000000000000, -1.000000000000000000, -0.000000000000000000 ) ) ;
#40592 = CONICAL_SURFACE ( 'NONE', #38530, 0.1000000000000002554, 0.003490658503988666988 ) ;
#40594 = EDGE_CURVE ( 'NONE', #95698, #101033, #79282, .T. ) ;
#40595 = AXIS2_PLACEMENT_3D ( 'NONE', #34048, #56253, #93607 ) ;
#40596 = AXIS2_PLACEMENT_3D ( 'NONE', #110119, #20453, #60397 ) ;
#40597 = ADVANCED_FACE ( 'NONE', ( #110653 ), #2014, .T. ) ;
#40598 = DIRECTION ( 'NONE',  ( 0.000000000000000000, 0.000000000000000000, -1.000000000000000000 ) ) ;
#40599 = EDGE_LOOP ( 'NONE', ( #102616, #35842 ) ) ;
#40600 = ORIENTED_EDGE ( 'NONE', *, *, #64015, .T. ) ;
#40601 = AXIS2_PLACEMENT_3D ( 'NONE', #118405, #16945, #78511 ) ;
#40602 = DIRECTION ( 'NONE',  ( 0.000000000000000000, 0.000000000000000000, 1.000000000000000000 ) ) ;
#40603 = EDGE_CURVE ( 'NONE', #20290, #61759, #4147, .T. ) ;
#40604 = PLANE ( 'NONE',  #113312 ) ;
#40605 = FACE_BOUND ( 'NONE', #102931, .T. ) ;
#40606 = EDGE_CURVE ( 'NONE', #58961, #8339, #94061, .T. ) ;
#40607 = DIRECTION ( 'NONE',  ( 0.000000000000000000, 1.000000000000000000, 0.000000000000000000 ) ) ;
#40608 = DIRECTION ( 'NONE',  ( 0.000000000000000000, 0.000000000000000000, 1.000000000000000000 ) ) ;
#40609 = AXIS2_PLACEMENT_3D ( 'NONE', #114340, #114973, #24682 ) ;
#40610 = EDGE_LOOP ( 'NONE', ( #107998, #46626 ) ) ;
#40611 = CARTESIAN_POINT ( 'NONE',  ( 8.949999999999919353, 2.500000000000000000, -6.048780366869526581 ) ) ;
#40612 = CARTESIAN_POINT ( 'NONE',  ( 0.3999999999999568345, 2.500000000000000000, -5.022947341949754119 ) ) ;
#40614 = EDGE_LOOP ( 'NONE', ( #29591, #14830, #47877, #46656 ) ) ;
#40613 = AXIS2_PLACEMENT_3D ( 'NONE', #28814, #99490, #60220 ) ;
#40615 = DIRECTION ( 'NONE',  ( -4.274815082592931898E-19, -0.9999939076577903929, -0.003490651415223739937 ) ) ;
#40616 = CARTESIAN_POINT ( 'NONE',  ( -10.84999999999999964, 2.500000000000000000, 5.802370205355744659 ) ) ;
#40617 = DIRECTION ( 'NONE',  ( 0.000000000000000000, 1.000000000000000000, 0.000000000000000000 ) ) ;
#40618 = CARTESIAN_POINT ( 'NONE',  ( 145.7653593504141725, 0.5000000000000000000, -3.576063159858998475 ) ) ;
#40619 = AXIS2_PLACEMENT_3D ( 'NONE', #13840, #4020, #45255 ) ;
#40620 = VECTOR ( 'NONE', #57629, 1000.000000000000000 ) ;
#40621 = ORIENTED_EDGE ( 'NONE', *, *, #4892, .F. ) ;
#40622 = CARTESIAN_POINT ( 'NONE',  ( -7.700000000000010836, 12.50000000000000000, 3.983716857408420964 ) ) ;
#40623 = CARTESIAN_POINT ( 'NONE',  ( 3.349999999999941913, 12.50000000000000000, 5.802370205355744659 ) ) ;
#40624 = EDGE_LOOP ( 'NONE', ( #112323, #108475, #66204, #104888 ) ) ;
#40625 = VERTEX_POINT ( 'NONE', #69433 ) ;
#40626 = CARTESIAN_POINT ( 'NONE',  ( 145.7653593504141725, 2.500000000000000000, -1.098523788719517169 ) ) ;
#40627 = EDGE_LOOP ( 'NONE', ( #65864, #59906 ) ) ;
#40628 = DIRECTION ( 'NONE',  ( -0.000000000000000000, -1.000000000000000000, -0.000000000000000000 ) ) ;
#40629 = CARTESIAN_POINT ( 'NONE',  ( 17.50000000000000000, -2.499999999999999556, -1.333333333333328596 ) ) ;
#40630 = AXIS2_PLACEMENT_3D ( 'NONE', #932, #51347, #80797 ) ;
#40631 = EDGE_CURVE ( 'NONE', #106830, #106590, #20900, .T. ) ;
#40632 = CARTESIAN_POINT ( 'NONE',  ( -11.05000000000000071, 2.500000000000000000, -6.741600689897074616 ) ) ;
#40633 = ORIENTED_EDGE ( 'NONE', *, *, #112627, .F. ) ;
#40635 = EDGE_CURVE ( 'NONE', #22601, #44517, #10429, .T. ) ;
#40634 = CARTESIAN_POINT ( 'NONE',  ( 1.899999999999951283, 2.500000000000000000, 0.3464101615137736845 ) ) ;
#40636 = DIRECTION ( 'NONE',  ( 0.000000000000000000, 0.000000000000000000, -1.000000000000000000 ) ) ;
#40637 = DIRECTION ( 'NONE',  ( -1.000000000000000000, 0.000000000000000000, 0.000000000000000000 ) ) ;
#40638 = CARTESIAN_POINT ( 'NONE',  ( 129.5000000000000000, 0.000000000000000000, 6.000000000000000000 ) ) ;
#40639 = CARTESIAN_POINT ( 'NONE',  ( 12.29999999999990656, 2.500000000000000000, 3.883716857408421319 ) ) ;
#40640 = DIRECTION ( 'NONE',  ( 0.000000000000000000, 0.000000000000000000, 1.000000000000000000 ) ) ;
#40641 = EDGE_LOOP ( 'NONE', ( #127631, #47403 ) ) ;
#40642 = VERTEX_POINT ( 'NONE', #38729 ) ;
#40643 = DIRECTION ( 'NONE',  ( 0.000000000000000000, 1.000000000000000000, 0.000000000000000000 ) ) ;
#40645 = ORIENTED_EDGE ( 'NONE', *, *, #35527, .T. ) ;
#40644 = AXIS2_PLACEMENT_3D ( 'NONE', #24941, #104763, #74043 ) ;
#40646 = VECTOR ( 'NONE', #71055, 1000.000000000000000 ) ;
#40647 = DIRECTION ( 'NONE',  ( 0.000000000000000000, 0.000000000000000000, -1.000000000000000000 ) ) ;
#40649 = ORIENTED_EDGE ( 'NONE', *, *, #72373, .T. ) ;
#40648 = ORIENTED_EDGE ( 'NONE', *, *, #102682, .F. ) ;
#40650 = ORIENTED_EDGE ( 'NONE', *, *, #73518, .T. ) ;
#40651 = AXIS2_PLACEMENT_3D ( 'NONE', #61028, #70214, #13203 ) ;
#40652 = CARTESIAN_POINT ( 'NONE',  ( 11.04999999999991012, 2.500000000000000000, -1.818653347947326138 ) ) ;
#40653 = AXIS2_PLACEMENT_3D ( 'NONE', #62631, #102532, #70497 ) ;
#40654 = CARTESIAN_POINT ( 'NONE',  ( -10.65000000000000391, 2.500000000000000000, -6.048780366869523029 ) ) ;
#40655 = DIRECTION ( 'NONE',  ( 0.000000000000000000, 0.000000000000000000, 1.000000000000000000 ) ) ;
#40656 = DIRECTION ( 'NONE',  ( -4.274815082592931898E-19, -0.9999939076577903929, -0.003490651415223739937 ) ) ;
#40657 = DIRECTION ( 'NONE',  ( 0.000000000000000000, 1.000000000000000000, 0.000000000000000000 ) ) ;
#40658 = DIRECTION ( 'NONE',  ( 0.000000000000000000, 0.000000000000000000, -1.000000000000000000 ) ) ;
#40659 = FACE_OUTER_BOUND ( 'NONE', #37690, .T. ) ;
#40660 = DIRECTION ( 'NONE',  ( 0.000000000000000000, 0.000000000000000000, 1.000000000000000000 ) ) ;
#40661 = LINE ( 'NONE', #13082, #8000 ) ;
#40662 = ORIENTED_EDGE ( 'NONE', *, *, #114950, .F. ) ;
#40663 = AXIS2_PLACEMENT_3D ( 'NONE', #54186, #12942, #14236 ) ;
#40664 = CARTESIAN_POINT ( 'NONE',  ( 9.349999999999919709, 12.50000000000000000, -6.776507416713040577 ) ) ;
#40665 = AXIS2_PLACEMENT_3D ( 'NONE', #120815, #31167, #2980 ) ;
#40666 = AXIS2_PLACEMENT_3D ( 'NONE', #93408, #4347, #104506 ) ;
#40667 = ORIENTED_EDGE ( 'NONE', *, *, #122642, .T. ) ;
#40668 = ORIENTED_EDGE ( 'NONE', *, *, #50079, .T. ) ;
#40669 = LINE ( 'NONE', #70747, #81669 ) ;
#40670 = DIRECTION ( 'NONE',  ( 0.000000000000000000, -0.000000000000000000, 1.000000000000000000 ) ) ;
#40671 = ADVANCED_FACE ( 'NONE', ( #39368 ), #35492, .T. ) ;
#40672 = CIRCLE ( 'NONE', #124175, 0.1000000000000002554 ) ;
#40673 = VECTOR ( 'NONE', #42419, 1000.000000000000000 ) ;
#40674 = CARTESIAN_POINT ( 'NONE',  ( 107.5000000000000142, 0.000000000000000000, 0.000000000000000000 ) ) ;
#40676 = CARTESIAN_POINT ( 'NONE',  ( -1.650000000000034328, 2.500000000000000000, -7.088010851410853519 ) ) ;
#40675 = AXIS2_PLACEMENT_3D ( 'NONE', #84091, #124684, #106324 ) ;
#40677 = DIRECTION ( 'NONE',  ( 0.000000000000000000, -0.9999939076577903929, 0.003490651415223739937 ) ) ;
#40678 = PLANE ( 'NONE',  #126245 ) ;
#40679 = VERTEX_POINT ( 'NONE', #59661 ) ;
#40681 = EDGE_LOOP ( 'NONE', ( #123758, #34023, #86395, #120343 ) ) ;
#40680 = AXIS2_PLACEMENT_3D ( 'NONE', #62075, #102619, #11668 ) ;
#40682 = CARTESIAN_POINT ( 'NONE',  ( -0.4000000000000396572, 12.50000000000000000, 3.702399969078682407 ) ) ;
#40683 = VECTOR ( 'NONE', #35287, 1000.000000000000000 ) ;
#40684 = ORIENTED_EDGE ( 'NONE', *, *, #74829, .F. ) ;
#40685 = DIRECTION ( 'NONE',  ( 0.000000000000000000, 0.000000000000000000, 1.000000000000000000 ) ) ;
#40686 = ORIENTED_EDGE ( 'NONE', *, *, #105840, .F. ) ;
#40687 = AXIS2_PLACEMENT_3D ( 'NONE', #6986, #127443, #25346 ) ;
#40688 = EDGE_CURVE ( 'NONE', #69752, #18590, #91910, .T. ) ;
#40689 = EDGE_CURVE ( 'NONE', #105649, #115836, #92475, .T. ) ;
#40690 = ORIENTED_EDGE ( 'NONE', *, *, #11883, .T. ) ;
#40691 = CARTESIAN_POINT ( 'NONE',  ( 4.599999999999937472, 12.50000000000000000, 0.7579135962115869374 ) ) ;
#40692 = DIRECTION ( 'NONE',  ( -0.000000000000000000, 1.000000000000000000, -0.000000000000000000 ) ) ;
#40693 = CARTESIAN_POINT ( 'NONE',  ( -3.550000000000027800, 2.500000000000000000, 6.148780366869520009 ) ) ;
#40694 = DIRECTION ( 'NONE',  ( 0.000000000000000000, -0.000000000000000000, 1.000000000000000000 ) ) ;
#40695 = CARTESIAN_POINT ( 'NONE',  ( 87.50000000000002842, 0.7169905660283034665, 7.500000000000000888 ) ) ;
#40696 = ORIENTED_EDGE ( 'NONE', *, *, #26079, .T. ) ;
#40697 = DIRECTION ( 'NONE',  ( 0.000000000000000000, 0.000000000000000000, 1.000000000000000000 ) ) ;
#40698 = CARTESIAN_POINT ( 'NONE',  ( 3.349999999999944578, 2.500000000000000000, -1.472243186433550122 ) ) ;
#40699 = EDGE_CURVE ( 'NONE', #102274, #88216, #98898, .T. ) ;
#40700 = CARTESIAN_POINT ( 'NONE',  ( -10.85000000000000142, 2.500000000000000000, -7.188010851410850499 ) ) ;
#40701 = CARTESIAN_POINT ( 'NONE',  ( 7.699999999999923794, 2.500000000000000000, -4.083716857408426826 ) ) ;
#40702 = VECTOR ( 'NONE', #3470, 1000.000000000000000 ) ;
#40703 = CARTESIAN_POINT ( 'NONE',  ( 6.049999999999932321, 2.500000000000000000, 6.941600689897073018 ) ) ;
#40704 = ORIENTED_EDGE ( 'NONE', *, *, #78020, .T. ) ;
#40705 = ORIENTED_EDGE ( 'NONE', *, *, #26984, .F. ) ;
#40706 = CARTESIAN_POINT ( 'NONE',  ( 6.899999999999926636, 12.50000000000000000, 0.3464101615137736845 ) ) ;
#40707 = ORIENTED_EDGE ( 'NONE', *, *, #75288, .T. ) ;
#40708 = CONICAL_SURFACE ( 'NONE', #53219, 0.1000000000000002554, 0.003490658503988666988 ) ;
#40709 = DIRECTION ( 'NONE',  ( -4.274815082592931898E-19, -0.9999939076577903929, -0.003490651415223739937 ) ) ;
#40710 = DIRECTION ( 'NONE',  ( 0.000000000000000000, 0.000000000000000000, -1.000000000000000000 ) ) ;
#40711 = AXIS2_PLACEMENT_3D ( 'NONE', #18331, #9165, #109954 ) ;
#40712 = EDGE_LOOP ( 'NONE', ( #13464, #52779, #17929, #49239 ) ) ;
#40713 = FACE_OUTER_BOUND ( 'NONE', #14932, .T. ) ;
#40714 = CARTESIAN_POINT ( 'NONE',  ( 8.349999999999923261, 2.500000000000000000, 1.472243186433545459 ) ) ;
#40715 = CARTESIAN_POINT ( 'NONE',  ( -2.300000000000033573, 2.500000000000000000, 4.676537180435972552 ) ) ;
#40716 = CARTESIAN_POINT ( 'NONE',  ( -6.505213034913026604E-15, 12.50000000000000000, 4.395220292106234439 ) ) ;
#40717 = AXIS2_PLACEMENT_3D ( 'NONE', #26383, #36205, #16527 ) ;
#40718 = EDGE_CURVE ( 'NONE', #108142, #90854, #15181, .T. ) ;
#40719 = DIRECTION ( 'NONE',  ( -0.000000000000000000, -1.000000000000000000, -0.000000000000000000 ) ) ;
#40720 = CIRCLE ( 'NONE', #11536, 0.06509327318403745899 ) ;
#40721 = EDGE_LOOP ( 'NONE', ( #88327, #116338, #65051, #99708 ) ) ;
#40722 = EDGE_CURVE ( 'NONE', #52069, #1010, #112601, .T. ) ;
#40723 = CARTESIAN_POINT ( 'NONE',  ( 3.549999999999942091, 2.500000000000000000, 2.611473670974873151 ) ) ;
#40724 = DIRECTION ( 'NONE',  ( 0.000000000000000000, -0.000000000000000000, 1.000000000000000000 ) ) ;
#40725 = EDGE_CURVE ( 'NONE', #8118, #21551, #14370, .T. ) ;
#40726 = CARTESIAN_POINT ( 'NONE',  ( -12.09999999999999609, 2.500000000000000000, 1.734723475976807094E-15 ) ) ;
#40727 = DIRECTION ( 'NONE',  ( 0.000000000000000000, 0.000000000000000000, 1.000000000000000000 ) ) ;
#40728 = VERTEX_POINT ( 'NONE', #73957 ) ;
#40729 = AXIS2_PLACEMENT_3D ( 'NONE', #6271, #76329, #104489 ) ;
#40730 = ADVANCED_FACE ( 'NONE', ( #83773 ), #53033, .T. ) ;
#40731 = EDGE_CURVE ( 'NONE', #124558, #128215, #27715, .T. ) ;
#40733 = VERTEX_POINT ( 'NONE', #54317 ) ;
#40732 = CIRCLE ( 'NONE', #73874, 0.06509327318403745899 ) ;
#40734 = DIRECTION ( 'NONE',  ( -0.000000000000000000, -1.000000000000000000, -0.000000000000000000 ) ) ;
#40735 = CARTESIAN_POINT ( 'NONE',  ( -13.54999999999998828, 2.500000000000000000, 1.918653347947325338 ) ) ;
#40736 = EDGE_CURVE ( 'NONE', #43212, #24381, #4369, .T. ) ;
#40737 = CARTESIAN_POINT ( 'NONE',  ( -9.600000000000006750, 12.50000000000000000, 0.6928203230275494784 ) ) ;
#40738 = AXIS2_PLACEMENT_3D ( 'NONE', #57957, #79527, #18665 ) ;
#40739 = ORIENTED_EDGE ( 'NONE', *, *, #107150, .T. ) ;
#40740 = CARTESIAN_POINT ( 'NONE',  ( -2.050000000000033129, 12.50000000000000000, 6.495190528383297135 ) ) ;
#40741 = ADVANCED_FACE ( 'NONE', ( #93595 ), #48572, .T. ) ;
#40742 = DIRECTION ( 'NONE',  ( 0.000000000000000000, 0.000000000000000000, 1.000000000000000000 ) ) ;
#40743 = ORIENTED_EDGE ( 'NONE', *, *, #19703, .T. ) ;
#40744 = PLANE ( 'NONE',  #97049 ) ;
#40745 = ORIENTED_EDGE ( 'NONE', *, *, #108875, .T. ) ;
#40746 = ADVANCED_FACE ( 'NONE', ( #72674 ), #62848, .T. ) ;
#40747 = DIRECTION ( 'NONE',  ( -1.000000000000000000, 0.000000000000000000, 0.000000000000000000 ) ) ;
#40748 = AXIS2_PLACEMENT_3D ( 'NONE', #40518, #41808, #88955 ) ;
#40749 = VERTEX_POINT ( 'NONE', #2619 ) ;
#40750 = CARTESIAN_POINT ( 'NONE',  ( 108.0000000000000142, 8.500000000000000000, 0.000000000000000000 ) ) ;
#40751 = CARTESIAN_POINT ( 'NONE',  ( 7.173569985920779324, 2.499999999999999112, -8.713264184442468974 ) ) ;
#40752 = CONICAL_SURFACE ( 'NONE', #92969, 0.1000000000000000472, 0.003490658503988666988 ) ;
#40753 = AXIS2_PLACEMENT_3D ( 'NONE', #17947, #117407, #108258 ) ;
#40754 = ORIENTED_EDGE ( 'NONE', *, *, #60099, .T. ) ;
#40755 = ORIENTED_EDGE ( 'NONE', *, *, #20196, .F. ) ;
#40756 = LINE ( 'NONE', #112054, #114586 ) ;
#40757 = CARTESIAN_POINT ( 'NONE',  ( -0.6500000000000394351, 12.50000000000000000, 2.576566944158910744 ) ) ;
#40758 = ORIENTED_EDGE ( 'NONE', *, *, #31960, .T. ) ;
#40759 = FACE_OUTER_BOUND ( 'NONE', #59799, .T. ) ;
#40760 = CARTESIAN_POINT ( 'NONE',  ( 1.849999999999949685, 2.500000000000000000, -2.411473670974877859 ) ) ;
#40761 = AXIS2_PLACEMENT_3D ( 'NONE', #12919, #127414, #64617 ) ;
#40762 = CONICAL_SURFACE ( 'NONE', #76255, 0.1000000000000000472, 0.003490658503988666988 ) ;
#40763 = CARTESIAN_POINT ( 'NONE',  ( 13.29999999999990301, 12.50000000000000000, 4.395220292106234439 ) ) ;
#40764 = CARTESIAN_POINT ( 'NONE',  ( 106.3580756688206321, 7.300875089796112327, -4.733840378913477309 ) ) ;
#40765 = DIRECTION ( 'NONE',  ( 0.000000000000000000, 1.000000000000000000, 0.000000000000000000 ) ) ;
#40766 = AXIS2_PLACEMENT_3D ( 'NONE', #19411, #60658, #100559 ) ;
#40767 = DIRECTION ( 'NONE',  ( 0.000000000000000000, 0.000000000000000000, 1.000000000000000000 ) ) ;
#40768 = DIRECTION ( 'NONE',  ( 0.000000000000000000, 0.000000000000000000, 1.000000000000000000 ) ) ;
#40769 = CIRCLE ( 'NONE', #90920, 0.06509327318403745899 ) ;
#40770 = VECTOR ( 'NONE', #91297, 1000.000000000000000 ) ;
#40771 = EDGE_LOOP ( 'NONE', ( #121724, #20163, #53519, #78912 ) ) ;
#40772 = EDGE_LOOP ( 'NONE', ( #8204, #116627 ) ) ;
#40773 = ORIENTED_EDGE ( 'NONE', *, *, #25263, .T. ) ;
#40774 = FACE_OUTER_BOUND ( 'NONE', #13488, .T. ) ;
#40775 = DIRECTION ( 'NONE',  ( -4.274815082592931898E-19, -0.9999939076577903929, -0.003490651415223739937 ) ) ;
#40776 = AXIS2_PLACEMENT_3D ( 'NONE', #35202, #75114, #102625 ) ;
#40777 = DIRECTION ( 'NONE',  ( 0.000000000000000000, 0.000000000000000000, 1.000000000000000000 ) ) ;
#40779 = ORIENTED_EDGE ( 'NONE', *, *, #84425, .T. ) ;
#40778 = ORIENTED_EDGE ( 'NONE', *, *, #80020, .F. ) ;
#40780 = FACE_BOUND ( 'NONE', #7269, .T. ) ;
#40781 = EDGE_LOOP ( 'NONE', ( #119177, #80715 ) ) ;
#40782 = DIRECTION ( 'NONE',  ( 0.000000000000000000, 0.000000000000000000, 1.000000000000000000 ) ) ;
#40783 = CARTESIAN_POINT ( 'NONE',  ( -6.850000000000013856, 2.500000000000000000, 2.511473670974873507 ) ) ;
#40784 = CARTESIAN_POINT ( 'NONE',  ( -9.400000000000007461, 2.500000000000000000, 0.2464101615137735679 ) ) ;
#40785 = CARTESIAN_POINT ( 'NONE',  ( 8.549999999999922551, 2.500000000000000000, -6.048780366869526581 ) ) ;
#40786 = EDGE_CURVE ( 'NONE', #88966, #44639, #123061, .T. ) ;
#40787 = CARTESIAN_POINT ( 'NONE',  ( 184.4062500006827747, -8.891194145520236347, -1.633285867636356299E-15 ) ) ;
#40788 = CARTESIAN_POINT ( 'NONE',  ( -3.150000000000030553, 12.50000000000000000, 6.083687093685482772 ) ) ;
#40789 = DIRECTION ( 'NONE',  ( 0.000000000000000000, -0.9999939076577903929, 0.003490651415223739937 ) ) ;
#40790 = DIRECTION ( 'NONE',  ( 0.000000000000000000, 0.000000000000000000, -1.000000000000000000 ) ) ;
#40791 = CARTESIAN_POINT ( 'NONE',  ( -4.600000000000025402, 2.500000000000000000, 0.09999999999999761857 ) ) ;
#40792 = AXIS2_PLACEMENT_3D ( 'NONE', #59108, #31577, #9356 ) ;
#40793 = DIRECTION ( 'NONE',  ( -0.000000000000000000, -1.000000000000000000, -0.000000000000000000 ) ) ;
#40794 = EDGE_CURVE ( 'NONE', #60983, #7100, #23510, .T. ) ;
#40795 = ORIENTED_EDGE ( 'NONE', *, *, #68890, .T. ) ;
#40796 = VERTEX_POINT ( 'NONE', #1982 ) ;
#40797 = ORIENTED_EDGE ( 'NONE', *, *, #74240, .T. ) ;
#40798 = EDGE_LOOP ( 'NONE', ( #86681, #73798 ) ) ;
#40799 = CARTESIAN_POINT ( 'NONE',  ( -12.89999999999999147, 2.500000000000000000, -5.022947341949751454 ) ) ;
#40800 = DIRECTION ( 'NONE',  ( -4.274815082592931898E-19, -0.9999939076577903929, -0.003490651415223739937 ) ) ;
#40802 = EDGE_LOOP ( 'NONE', ( #89229, #126062, #29632, #67122 ) ) ;
#40801 = ORIENTED_EDGE ( 'NONE', *, *, #7628, .F. ) ;
#40803 = ORIENTED_EDGE ( 'NONE', *, *, #128005, .F. ) ;
#40804 = DIRECTION ( 'NONE',  ( 0.000000000000000000, -0.9999939076577903929, 0.003490651415223739937 ) ) ;
#40805 = AXIS2_PLACEMENT_3D ( 'NONE', #67925, #99334, #70502 ) ;
#40806 = CARTESIAN_POINT ( 'NONE',  ( -3.469446951953614189E-14, 12.50000000000000000, -0.6928203230275519209 ) ) ;
#40807 =( NAMED_UNIT ( * ) PLANE_ANGLE_UNIT ( ) SI_UNIT ( $, .RADIAN. ) );
#40808 = DIRECTION ( 'NONE',  ( -0.000000000000000000, 1.000000000000000000, -0.000000000000000000 ) ) ;
#40809 = DIRECTION ( 'NONE',  ( 0.000000000000000000, 0.000000000000000000, 1.000000000000000000 ) ) ;
#40810 = DIRECTION ( 'NONE',  ( 0.000000000000000000, 1.000000000000000000, 0.000000000000000000 ) ) ;
#40811 = DIRECTION ( 'NONE',  ( 0.000000000000000000, 0.000000000000000000, 1.000000000000000000 ) ) ;
#40812 = ORIENTED_EDGE ( 'NONE', *, *, #109896, .T. ) ;
#40813 = DIRECTION ( 'NONE',  ( 0.000000000000000000, 0.000000000000000000, 1.000000000000000000 ) ) ;
#40814 = VERTEX_POINT ( 'NONE', #111276 ) ;
#40815 = AXIS2_PLACEMENT_3D ( 'NONE', #62918, #53106, #64197 ) ;
#40816 = ORIENTED_EDGE ( 'NONE', *, *, #15056, .T. ) ;
#40817 = VERTEX_POINT ( 'NONE', #121120 ) ;
#40818 = VECTOR ( 'NONE', #37219, 1000.000000000000000 ) ;
#40819 = CARTESIAN_POINT ( 'NONE',  ( 3.749999999999978684, 2.500000000000000000, -6.495190528383302464 ) ) ;
#40820 = ORIENTED_EDGE ( 'NONE', *, *, #50809, .T. ) ;
#40821 = EDGE_LOOP ( 'NONE', ( #84318, #29981, #95771, #55611 ) ) ;
#40822 = VERTEX_POINT ( 'NONE', #61577 ) ;
#40823 = CARTESIAN_POINT ( 'NONE',  ( -4.550000000000022915, 12.50000000000000000, -2.165063509461101710 ) ) ;
#40824 = ADVANCED_FACE ( 'NONE', ( #33407 ), #40254, .T. ) ;
#40826 = AXIS2_PLACEMENT_3D ( 'NONE', #61836, #102395, #53933 ) ;
#40825 = CARTESIAN_POINT ( 'NONE',  ( -8.350000000000013856, 2.500000000000000000, -6.495190528383297135 ) ) ;
#40827 = CARTESIAN_POINT ( 'NONE',  ( 6.649999999999928413, 12.50000000000000000, 2.857883832488649301 ) ) ;
#40828 = CONICAL_SURFACE ( 'NONE', #24083, 0.1000000000000002554, 0.003490658503988666988 ) ;
#40829 = DIRECTION ( 'NONE',  ( -0.000000000000000000, 1.000000000000000000, -0.000000000000000000 ) ) ;
#40830 = CARTESIAN_POINT ( 'NONE',  ( -3.300000000000027800, 12.50000000000000000, -2.276824562219559311E-15 ) ) ;
#40831 = CARTESIAN_POINT ( 'NONE',  ( -1.050000000000038680, 12.50000000000000000, 6.841600689897072485 ) ) ;
#40832 = CARTESIAN_POINT ( 'NONE',  ( -3.300000000000028244, 12.50000000000000000, 4.265033745738159077 ) ) ;
#40833 = EDGE_CURVE ( 'NONE', #127817, #77958, #81830, .T. ) ;
#40834 = ORIENTED_EDGE ( 'NONE', *, *, #73839, .T. ) ;
#40835 = FACE_OUTER_BOUND ( 'NONE', #106260, .T. ) ;
#40836 = EDGE_LOOP ( 'NONE', ( #120826, #14178, #49371, #21860 ) ) ;
#40837 = CARTESIAN_POINT ( 'NONE',  ( 111.7562837278403549, 8.047280753376885087, 3.315426444331004863 ) ) ;
#40838 = DIRECTION ( 'NONE',  ( 0.000000000000000000, 1.000000000000000000, 0.000000000000000000 ) ) ;
#40839 = VERTEX_POINT ( 'NONE', #11806 ) ;
#40841 = EDGE_CURVE ( 'NONE', #4435, #9738, #41932, .T. ) ;
#40840 = CARTESIAN_POINT ( 'NONE',  ( -5.850000000000021849, 2.500000000000000000, -1.372243186433550033 ) ) ;
#40842 = DIRECTION ( 'NONE',  ( 0.000000000000000000, 1.000000000000000000, 0.000000000000000000 ) ) ;
#40843 = ADVANCED_FACE ( 'NONE', ( #63496 ), #122423, .T. ) ;
#40844 = CIRCLE ( 'NONE', #118174, 0.06509327318403745899 ) ;
#40845 = ORIENTED_EDGE ( 'NONE', *, *, #122133, .F. ) ;
#40846 = CONICAL_SURFACE ( 'NONE', #103514, 0.09999999999999999167, 0.003490658503988666988 ) ;
#40847 = EDGE_CURVE ( 'NONE', #51297, #63587, #121757, .T. ) ;
#40849 = CARTESIAN_POINT ( 'NONE',  ( -0.2000000000000412836, 12.50000000000000000, 4.611443907251934426 ) ) ;
#40848 = VECTOR ( 'NONE', #57248, 1000.000000000000000 ) ;
#40850 = ORIENTED_EDGE ( 'NONE', *, *, #31383, .T. ) ;
#40851 = CIRCLE ( 'NONE', #118181, 0.09999999999999999167 ) ;
#40852 = VERTEX_POINT ( 'NONE', #17598 ) ;
#40853 = DIRECTION ( 'NONE',  ( 0.000000000000000000, 0.000000000000000000, 1.000000000000000000 ) ) ;
#40854 = CARTESIAN_POINT ( 'NONE',  ( -9.200000000000009948, 2.500000000000000000, -4.330127018922197202 ) ) ;
#40855 = ADVANCED_FACE ( 'NONE', ( #34700 ), #104687, .T. ) ;
#40856 = CARTESIAN_POINT ( 'NONE',  ( 185.0052083336747444, -6.551208109652278289, 3.782341765624995134 ) ) ;
#40857 = CARTESIAN_POINT ( 'NONE',  ( -13.94999999999998685, 2.500000000000000000, -2.611473670974875372 ) ) ;
#40858 = CIRCLE ( 'NONE', #32536, 0.1000000000000002554 ) ;
#40859 = DIRECTION ( 'NONE',  ( 0.000000000000000000, 1.000000000000000000, 0.000000000000000000 ) ) ;
#40860 = CIRCLE ( 'NONE', #70078, 0.09999999999999982514 ) ;
#40861 = ORIENTED_EDGE ( 'NONE', *, *, #61831, .T. ) ;
#40862 = AXIS2_PLACEMENT_3D ( 'NONE', #97636, #111141, #50974 ) ;
#40863 = DIRECTION ( 'NONE',  ( 0.000000000000000000, 1.000000000000000000, 0.000000000000000000 ) ) ;
#40864 = VECTOR ( 'NONE', #84790, 1000.000000000000000 ) ;
#40865 = ORIENTED_EDGE ( 'NONE', *, *, #39432, .T. ) ;
#40866 = CONICAL_SURFACE ( 'NONE', #42924, 0.09999999999999982514, 0.003490658503988666988 ) ;
#40867 = CARTESIAN_POINT ( 'NONE',  ( -5.450000000000023270, 12.50000000000000000, -2.165063509461101710 ) ) ;
#40869 = CONICAL_SURFACE ( 'NONE', #99438, 0.1000000000000002554, 0.003490658503988666988 ) ;
#40868 = CARTESIAN_POINT ( 'NONE',  ( -8.550000000000013145, 2.500000000000000000, -6.841600689897073373 ) ) ;
#40870 = ADVANCED_FACE ( 'NONE', ( #15656 ), #96660, .T. ) ;
#40871 = AXIS2_PLACEMENT_3D ( 'NONE', #97651, #116642, #108750 ) ;
#40872 = FACE_OUTER_BOUND ( 'NONE', #121413, .T. ) ;
#40873 = CARTESIAN_POINT ( 'NONE',  ( 11.04999999999990656, 2.500000000000000000, 2.511473670974873507 ) ) ;
#40874 = DIRECTION ( 'NONE',  ( 0.000000000000000000, 1.000000000000000000, 0.000000000000000000 ) ) ;
#40875 = CARTESIAN_POINT ( 'NONE',  ( 1.249999999999952482, 12.50000000000000000, -5.737276932171712751 ) ) ;
#40876 = CARTESIAN_POINT ( 'NONE',  ( -9.150000000000005684, 12.50000000000000000, 6.560283801567334372 ) ) ;
#40877 = VERTEX_POINT ( 'NONE', #117082 ) ;
#40878 = DIRECTION ( 'NONE',  ( 0.000000000000000000, 0.000000000000000000, -1.000000000000000000 ) ) ;
#40879 = EDGE_CURVE ( 'NONE', #82797, #7894, #107132, .T. ) ;
#40880 = CARTESIAN_POINT ( 'NONE',  ( 6.449999999999931788, 2.500000000000000000, 6.048780366869520364 ) ) ;
#40881 = DIRECTION ( 'NONE',  ( 0.000000000000000000, 0.000000000000000000, -1.000000000000000000 ) ) ;
#40882 = AXIS2_PLACEMENT_3D ( 'NONE', #48479, #129003, #60256 ) ;
#40883 = ORIENTED_EDGE ( 'NONE', *, *, #28024, .F. ) ;
#40884 = ADVANCED_FACE ( 'NONE', ( #54952 ), #45795, .F. ) ;
#40885 = DIRECTION ( 'NONE',  ( -0.000000000000000000, 1.000000000000000000, -0.000000000000000000 ) ) ;
#40886 = ORIENTED_EDGE ( 'NONE', *, *, #29123, .F. ) ;
#40887 = B_SPLINE_SURFACE_WITH_KNOTS ( 'NONE', 3, 1, ( 
 ( #21020, #41333 ),
 ( #81863, #90 ),
 ( #91055, #1373 ),
 ( #32802, #22966 ),
 ( #99599, #79942 ),
 ( #40695, #119868 ),
 ( #20388, #70770 ),
 ( #60330, #50484 ),
 ( #90391, #730 ),
 ( #73995, #104722 ) ),
 .UNSPECIFIED., .F., .F., .F.,
 ( 4, 2, 2, 2, 4 ),
 ( 2, 2 ),
 ( 0.000000000000000000, 0.2499999999999999445, 0.4999999999999998890, 0.7499999999999998890, 1.000000000000000000 ),
 ( 0.000000000000000000, 1.000000000000000000 ),
 .UNSPECIFIED. ) ;
#40888 = ORIENTED_EDGE ( 'NONE', *, *, #105533, .T. ) ;
#40889 = FACE_OUTER_BOUND ( 'NONE', #105247, .T. ) ;
#40890 = EDGE_CURVE ( 'NONE', #124382, #117877, #56238, .T. ) ;
#40891 = AXIS2_PLACEMENT_3D ( 'NONE', #12567, #30952, #51242 ) ;
#40892 = ORIENTED_EDGE ( 'NONE', *, *, #88119, .T. ) ;
#40893 = DIRECTION ( 'NONE',  ( 0.000000000000000000, 0.000000000000000000, 1.000000000000000000 ) ) ;
#40895 = EDGE_CURVE ( 'NONE', #104198, #77609, #24856, .T. ) ;
#40894 = DIRECTION ( 'NONE',  ( 0.000000000000000000, 0.000000000000000000, -1.000000000000000000 ) ) ;
#40896 = EDGE_CURVE ( 'NONE', #76783, #70057, #6462, .T. ) ;
#40897 = AXIS2_PLACEMENT_3D ( 'NONE', #27198, #125408, #84181 ) ;
#40898 = ORIENTED_EDGE ( 'NONE', *, *, #1637, .T. ) ;
#40899 = CARTESIAN_POINT ( 'NONE',  ( -9.350000000000004974, 2.500000000000000000, 6.248780366869521430 ) ) ;
#40900 = ADVANCED_FACE ( 'NONE', ( #46417 ), #6763, .T. ) ;
#40901 = DIRECTION ( 'NONE',  ( 0.000000000000000000, 1.000000000000000000, 0.000000000000000000 ) ) ;
#40902 = CARTESIAN_POINT ( 'NONE',  ( 4.149999999999938183, 2.500000000000000000, 5.802370205355744659 ) ) ;
#40903 = ORIENTED_EDGE ( 'NONE', *, *, #77093, .F. ) ;
#40904 = EDGE_CURVE ( 'NONE', #46019, #94540, #67397, .T. ) ;
#40905 = VECTOR ( 'NONE', #86410, 1000.000000000000000 ) ;
#40906 = ADVANCED_FACE ( 'NONE', ( #125615 ), #117580, .T. ) ;
#40907 = VERTEX_POINT ( 'NONE', #37267 ) ;
#40908 = CIRCLE ( 'NONE', #114049, 0.09999999999999982514 ) ;
#40909 = ORIENTED_EDGE ( 'NONE', *, *, #40635, .T. ) ;
#40910 = CARTESIAN_POINT ( 'NONE',  ( -14.54999999999998472, 12.50000000000000000, 2.165063509461101265 ) ) ;
#40911 = DIRECTION ( 'NONE',  ( 0.000000000000000000, -0.9999939076577903929, 0.003490651415223739937 ) ) ;
#40912 = CARTESIAN_POINT ( 'NONE',  ( 9.399999999999918643, 2.500000000000000000, -0.2464101615137782308 ) ) ;
#40913 = FACE_BOUND ( 'NONE', #58776, .T. ) ;
#40914 = ORIENTED_EDGE ( 'NONE', *, *, #85480, .T. ) ;
#40915 = CARTESIAN_POINT ( 'NONE',  ( -0.8500000000000382805, 2.500000000000000000, -7.288010851410854585 ) ) ;
#40916 = CARTESIAN_POINT ( 'NONE',  ( 3.549999999999943867, 2.500000000000000000, -6.248780366869526759 ) ) ;
#40917 = ORIENTED_EDGE ( 'NONE', *, *, #807, .F. ) ;
#40918 = DIRECTION ( 'NONE',  ( -0.000000000000000000, 1.000000000000000000, -0.000000000000000000 ) ) ;
#40920 = DIRECTION ( 'NONE',  ( 0.000000000000000000, 1.000000000000000000, 0.000000000000000000 ) ) ;
#40919 = AXIS2_PLACEMENT_3D ( 'NONE', #111558, #21910, #63759 ) ;
#40921 = AXIS2_PLACEMENT_3D ( 'NONE', #86628, #55251, #63785 ) ;
#40922 = DIRECTION ( 'NONE',  ( -0.000000000000000000, 1.000000000000000000, -0.000000000000000000 ) ) ;
#40923 = DIRECTION ( 'NONE',  ( -0.000000000000000000, -1.000000000000000000, -0.000000000000000000 ) ) ;
#40924 = DIRECTION ( 'NONE',  ( 0.000000000000000000, 0.000000000000000000, 1.000000000000000000 ) ) ;
#40925 = CARTESIAN_POINT ( 'NONE',  ( -6.900000000000015454, 2.500000000000000000, 4.576537180435972019 ) ) ;
#40926 = ADVANCED_FACE ( 'NONE', ( #35330 ), #61177, .T. ) ;
#40927 = CARTESIAN_POINT ( 'NONE',  ( 9.199999999999919353, 2.500000000000000000, 0.09999999999999772959 ) ) ;
#40928 = ORIENTED_EDGE ( 'NONE', *, *, #83838, .F. ) ;
#40929 = ORIENTED_EDGE ( 'NONE', *, *, #29024, .T. ) ;
#40930 = EDGE_LOOP ( 'NONE', ( #70665, #120877 ) ) ;
#40931 = ORIENTED_EDGE ( 'NONE', *, *, #110876, .T. ) ;
#40932 = DIRECTION ( 'NONE',  ( 0.000000000000000000, 1.000000000000000000, 0.000000000000000000 ) ) ;
#40933 = CARTESIAN_POINT ( 'NONE',  ( 5.649999999999932854, 2.500000000000000000, 2.511473670974873507 ) ) ;
#40934 = ORIENTED_EDGE ( 'NONE', *, *, #104995, .F. ) ;
#40935 = FACE_BOUND ( 'NONE', #54357, .T. ) ;
#40936 = AXIS2_PLACEMENT_3D ( 'NONE', #71219, #120968, #41144 ) ;
#40937 = DIRECTION ( 'NONE',  ( -0.000000000000000000, 1.000000000000000000, -0.000000000000000000 ) ) ;
#40938 = CARTESIAN_POINT ( 'NONE',  ( 6.649999999999930189, 2.500000000000000000, -1.472243186433550122 ) ) ;
#40939 = AXIS2_PLACEMENT_3D ( 'NONE', #62354, #61712, #82638 ) ;
#40940 = CARTESIAN_POINT ( 'NONE',  ( 8.549999999999920774, 2.500000000000000000, 6.048780366869521252 ) ) ;
#40941 = VECTOR ( 'NONE', #901, 1000.000000000000000 ) ;
#40942 = FACE_OUTER_BOUND ( 'NONE', #107084, .T. ) ;
#40943 = CARTESIAN_POINT ( 'NONE',  ( 4.599999999999939249, 12.50000000000000000, -3.572213422710612374 ) ) ;
#40944 = DIRECTION ( 'NONE',  ( -0.000000000000000000, -1.000000000000000000, -0.000000000000000000 ) ) ;
#40945 = FACE_OUTER_BOUND ( 'NONE', #83496, .T. ) ;
#40946 = LINE ( 'NONE', #23199, #74786 ) ;
#40947 = ORIENTED_EDGE ( 'NONE', *, *, #40904, .F. ) ;
#40948 = AXIS2_PLACEMENT_3D ( 'NONE', #12465, #24233, #125007 ) ;
#40949 = EDGE_LOOP ( 'NONE', ( #117562, #60051, #86869, #42468 ) ) ;
#40950 = EDGE_CURVE ( 'NONE', #84951, #124476, #31841, .T. ) ;
#40951 = VERTEX_POINT ( 'NONE', #96802 ) ;
#40952 = VERTEX_POINT ( 'NONE', #67321 ) ;
#40953 = ORIENTED_EDGE ( 'NONE', *, *, #19572, .T. ) ;
#40954 = VERTEX_POINT ( 'NONE', #85057 ) ;
#40955 = AXIS2_PLACEMENT_3D ( 'NONE', #110236, #120701, #28466 ) ;
#40956 = CARTESIAN_POINT ( 'NONE',  ( -11.64999999999999680, 2.500000000000000000, 2.165063509461097713 ) ) ;
#40957 = EDGE_LOOP ( 'NONE', ( #108599, #24528, #25369, #92464 ) ) ;
#40958 = CIRCLE ( 'NONE', #99437, 0.1000000000000002554 ) ;
#40959 = AXIS2_PLACEMENT_3D ( 'NONE', #76662, #45923, #87115 ) ;
#40960 = CONICAL_SURFACE ( 'NONE', #84757, 0.09999999999999982514, 0.003490658503988666988 ) ;
#40961 = CARTESIAN_POINT ( 'NONE',  ( 19.52519901027826421, 0.5909487300084502737, 4.333354523369964184 ) ) ;
#40962 = CARTESIAN_POINT ( 'NONE',  ( 184.8593750003413732, 0.000000000000000000, 7.564683531250000925 ) ) ;
#40963 = DIRECTION ( 'NONE',  ( 0.000000000000000000, 1.000000000000000000, 0.000000000000000000 ) ) ;
#40965 = VECTOR ( 'NONE', #111995, 1000.000000000000000 ) ;
#40964 = CARTESIAN_POINT ( 'NONE',  ( 4.399999999999939071, 12.50000000000000000, 0.3464101615137736845 ) ) ;
#40966 = ORIENTED_EDGE ( 'NONE', *, *, #36751, .F. ) ;
#40967 = DIRECTION ( 'NONE',  ( 0.000000000000000000, -0.000000000000000000, 1.000000000000000000 ) ) ;
#40968 = EDGE_LOOP ( 'NONE', ( #97896, #7811 ) ) ;
#40969 = ORIENTED_EDGE ( 'NONE', *, *, #20634, .T. ) ;
#40970 = FACE_OUTER_BOUND ( 'NONE', #8662, .T. ) ;
#40971 = FACE_OUTER_BOUND ( 'NONE', #2919, .T. ) ;
#40972 = DIRECTION ( 'NONE',  ( 0.000000000000000000, 0.000000000000000000, 1.000000000000000000 ) ) ;
#40973 = CIRCLE ( 'NONE', #74396, 0.1000000000000000472 ) ;
#40974 = EDGE_LOOP ( 'NONE', ( #19576, #117685, #42363, #70440 ) ) ;
#40975 = ORIENTED_EDGE ( 'NONE', *, *, #50834, .T. ) ;
#40976 = CARTESIAN_POINT ( 'NONE',  ( 11.64999999999990798, 2.500000000000000000, -1.472243186433550122 ) ) ;
#40977 = DIRECTION ( 'NONE',  ( 0.000000000000000000, 0.000000000000000000, -1.000000000000000000 ) ) ;
#40978 = DIRECTION ( 'NONE',  ( 0.000000000000000000, 0.000000000000000000, -1.000000000000000000 ) ) ;
#40979 = CARTESIAN_POINT ( 'NONE',  ( 10.44999999999991047, 2.500000000000000000, -6.395190528383301931 ) ) ;
#40980 = ORIENTED_EDGE ( 'NONE', *, *, #113086, .T. ) ;
#40981 = DIRECTION ( 'NONE',  ( 0.000000000000000000, -0.9999939076577903929, 0.003490651415223739937 ) ) ;
#40982 = CIRCLE ( 'NONE', #93195, 0.09999999999999999167 ) ;
#40983 = ORIENTED_EDGE ( 'NONE', *, *, #42807, .F. ) ;
#40985 = AXIS2_PLACEMENT_3D ( 'NONE', #12701, #92573, #82773 ) ;
#40984 = DIRECTION ( 'NONE',  ( 0.000000000000000000, -0.9999939076577903929, 0.003490651415223739937 ) ) ;
#40986 = ADVANCED_FACE ( 'NONE', ( #107278 ), #42308, .T. ) ;
#40987 = VERTEX_POINT ( 'NONE', #84416 ) ;
#40988 = AXIS2_PLACEMENT_3D ( 'NONE', #106716, #27500, #125702 ) ;
#40989 = CARTESIAN_POINT ( 'NONE',  ( -3.100000000000028511, 2.500000000000000000, -3.983716857408426293 ) ) ;
#40990 = CARTESIAN_POINT ( 'NONE',  ( 6.849999999999929479, 2.500000000000000000, 6.248780366869520542 ) ) ;
#40991 = LINE ( 'NONE', #2308, #28125 ) ;
#40992 = EDGE_CURVE ( 'NONE', #90531, #41827, #77883, .T. ) ;
#40993 = CARTESIAN_POINT ( 'NONE',  ( -9.600000000000008527, 12.50000000000000000, -4.330127018922197202 ) ) ;
#40994 = EDGE_CURVE ( 'NONE', #13065, #85675, #45155, .T. ) ;
#40995 = VERTEX_POINT ( 'NONE', #75239 ) ;
#40996 = CIRCLE ( 'NONE', #43146, 0.06509327318403745899 ) ;
#40997 = CARTESIAN_POINT ( 'NONE',  ( -9.150000000000009237, 2.500000000000000000, -2.757883832488654097 ) ) ;
#40999 = AXIS2_PLACEMENT_3D ( 'NONE', #90485, #97255, #829 ) ;
#40998 = CIRCLE ( 'NONE', #45190, 0.09999999999999999167 ) ;
#41000 = EDGE_CURVE ( 'NONE', #97220, #28707, #115134, .T. ) ;
#41001 = CARTESIAN_POINT ( 'NONE',  ( -12.69999999999999218, 12.50000000000000000, -0.4115034346978115321 ) ) ;
#41002 = ORIENTED_EDGE ( 'NONE', *, *, #95906, .F. ) ;
#41003 = EDGE_CURVE ( 'NONE', #101165, #85897, #100665, .T. ) ;
#41004 = ORIENTED_EDGE ( 'NONE', *, *, #1060, .F. ) ;
#41005 = EDGE_CURVE ( 'NONE', #26724, #54326, #119040, .T. ) ;
#41006 = ORIENTED_EDGE ( 'NONE', *, *, #126863, .F. ) ;
#41007 = DIRECTION ( 'NONE',  ( 0.000000000000000000, 0.000000000000000000, -1.000000000000000000 ) ) ;
#41008 = CARTESIAN_POINT ( 'NONE',  ( 1.849999999999950129, 2.500000000000000000, -6.841600689897078702 ) ) ;
#41009 = DIRECTION ( 'NONE',  ( 0.000000000000000000, 1.000000000000000000, 0.000000000000000000 ) ) ;
#41010 = EDGE_CURVE ( 'NONE', #70210, #61697, #110501, .T. ) ;
#41011 = DIRECTION ( 'NONE',  ( 0.000000000000000000, 0.000000000000000000, 1.000000000000000000 ) ) ;
#41012 = CARTESIAN_POINT ( 'NONE',  ( 11.24999999999994493, 2.500000000000000000, -2.065063509461102065 ) ) ;
#41013 = CARTESIAN_POINT ( 'NONE',  ( 14.14999999999989377, 12.50000000000000000, -1.472243186433550122 ) ) ;
#41014 = CIRCLE ( 'NONE', #72298, 0.06509327318403745899 ) ;
#41015 = CARTESIAN_POINT ( 'NONE',  ( 13.94999999999989804, 2.500000000000000000, 1.818653347947321475 ) ) ;
#41016 = DIRECTION ( 'NONE',  ( 0.000000000000000000, 1.000000000000000000, 0.000000000000000000 ) ) ;
#41017 = CARTESIAN_POINT ( 'NONE',  ( -2.900000000000029221, 2.500000000000000000, -4.430127018922202176 ) ) ;
#41018 = ORIENTED_EDGE ( 'NONE', *, *, #108766, .T. ) ;
#41019 = CARTESIAN_POINT ( 'NONE',  ( 6.449999999999933564, 12.50000000000000000, -6.841600689897078702 ) ) ;
#41020 = DIRECTION ( 'NONE',  ( 0.000000000000000000, 0.000000000000000000, 1.000000000000000000 ) ) ;
#41021 = LINE ( 'NONE', #29890, #19272 ) ;
#41022 = DIRECTION ( 'NONE',  ( 0.000000000000000000, 1.000000000000000000, 0.000000000000000000 ) ) ;
#41023 = ORIENTED_EDGE ( 'NONE', *, *, #81030, .F. ) ;
#41024 = CARTESIAN_POINT ( 'NONE',  ( 8.349999999999923261, 2.500000000000000000, 2.165063509461097713 ) ) ;
#41025 = CONICAL_SURFACE ( 'NONE', #51478, 0.1000000000000002554, 0.003490658503988666988 ) ;
#41026 = CIRCLE ( 'NONE', #30564, 0.06509327318403745899 ) ;
#41027 = DIRECTION ( 'NONE',  ( 0.000000000000000000, 1.000000000000000000, 0.000000000000000000 ) ) ;
#41029 = ORIENTED_EDGE ( 'NONE', *, *, #480, .T. ) ;
#41028 = CARTESIAN_POINT ( 'NONE',  ( 11.24999999999990763, 2.500000000000000000, 1.572243186433545548 ) ) ;
#41030 =( BOUNDED_CURVE ( )  B_SPLINE_CURVE ( 2, ( #115397, #44774, #106258, #16564, #96419, #45416, #65018 ),
 .UNSPECIFIED., .F., .F. ) 
 B_SPLINE_CURVE_WITH_KNOTS ( ( 3, 2, 2, 3 ),
 ( 0.5714285714285719520, 0.5952380952380957879, 0.6190476190476195129, 0.6428571428571433488 ),
 .UNSPECIFIED. ) 
 CURVE ( )  GEOMETRIC_REPRESENTATION_ITEM ( )  RATIONAL_B_SPLINE_CURVE ( ( 0.9999999999999968914, 0.8660254037844418162, 1.000000000000000000, 0.8660254037844387076, 1.000000000000000000, 0.8660254037844361541, 1.000000000000002442 ) ) 
 REPRESENTATION_ITEM ( '' )  );
#41031 = EDGE_CURVE ( 'NONE', #23794, #17700, #19300, .T. ) ;
#41032 = VERTEX_POINT ( 'NONE', #67990 ) ;
#41033 = CIRCLE ( 'NONE', #34769, 0.06509327318403745899 ) ;
#41034 = DIRECTION ( 'NONE',  ( 0.000000000000000000, 0.000000000000000000, 1.000000000000000000 ) ) ;
#41035 = EDGE_LOOP ( 'NONE', ( #95054, #123961, #58791, #11333 ) ) ;
#41036 = EDGE_LOOP ( 'NONE', ( #10362, #81350, #23148, #44027 ) ) ;
#41037 = FACE_OUTER_BOUND ( 'NONE', #60945, .T. ) ;
#41038 = EDGE_CURVE ( 'NONE', #123828, #83387, #54903, .T. ) ;
#41039 = ADVANCED_FACE ( 'NONE', ( #29382 ), #89575, .T. ) ;
#41040 = CARTESIAN_POINT ( 'NONE',  ( 5.849999999999933031, 2.500000000000000000, -1.372243186433550033 ) ) ;
#41042 = EDGE_CURVE ( 'NONE', #117955, #71169, #13029, .T. ) ;
#41041 = CARTESIAN_POINT ( 'NONE',  ( -6.050000000000020250, 2.500000000000000000, -6.941600689897078347 ) ) ;
#41044 = AXIS2_PLACEMENT_3D ( 'NONE', #30912, #110734, #2064 ) ;
#41043 = CIRCLE ( 'NONE', #57757, 0.09999999999999982514 ) ;
#41045 = DIRECTION ( 'NONE',  ( 0.000000000000000000, 0.000000000000000000, -1.000000000000000000 ) ) ;
#41046 = ORIENTED_EDGE ( 'NONE', *, *, #1179, .F. ) ;
#41047 = CONICAL_SURFACE ( 'NONE', #18023, 0.1000000000000002554, 0.003490658503988666988 ) ;
#41048 = DIRECTION ( 'NONE',  ( 0.000000000000000000, 0.000000000000000000, 1.000000000000000000 ) ) ;
#41049 = ORIENTED_EDGE ( 'NONE', *, *, #41158, .F. ) ;
#41050 = ADVANCED_FACE ( 'NONE', ( #19542 ), #46594, .T. ) ;
#41051 = DIRECTION ( 'NONE',  ( 1.000000000000000000, 0.000000000000000000, -0.000000000000000000 ) ) ;
#41052 = EDGE_CURVE ( 'NONE', #120493, #112688, #27805, .T. ) ;
#41053 = CARTESIAN_POINT ( 'NONE',  ( 0.8499999999999536815, 2.500000000000000000, 5.802370205355744659 ) ) ;
#41054 = ADVANCED_FACE ( 'NONE', ( #109868 ), #40359, .T. ) ;
#41055 = ORIENTED_EDGE ( 'NONE', *, *, #75443, .T. ) ;
#41056 = EDGE_CURVE ( 'NONE', #63798, #11368, #57049, .T. ) ;
#41057 = EDGE_CURVE ( 'NONE', #24974, #68058, #50300, .T. ) ;
#41058 = EDGE_LOOP ( 'NONE', ( #46176, #17582 ) ) ;
#41059 = ORIENTED_EDGE ( 'NONE', *, *, #64408, .F. ) ;
#41060 = EDGE_LOOP ( 'NONE', ( #38844, #75658 ) ) ;
#41061 = DIRECTION ( 'NONE',  ( 0.000000000000000000, -0.000000000000000000, 1.000000000000000000 ) ) ;
#41062 = CARTESIAN_POINT ( 'NONE',  ( 9.112263991835201082, 1.500000000000000222, 9.392448311626331758 ) ) ;
#41063 = CARTESIAN_POINT ( 'NONE',  ( 4.599999999999936584, 2.500000000000000000, 4.330127018922196314 ) ) ;
#41064 = FACE_BOUND ( 'NONE', #122014, .T. ) ;
#41065 = CARTESIAN_POINT ( 'NONE',  ( -2.900000000000030109, 2.500000000000000000, -3.637306695894650055 ) ) ;
#41066 = AXIS2_PLACEMENT_3D ( 'NONE', #29348, #39818, #69239 ) ;
#41067 = CARTESIAN_POINT ( 'NONE',  ( 185.0312500006828031, 9.429780353434619030E-16, -7.700000000000000178 ) ) ;
#41068 = EDGE_CURVE ( 'NONE', #57799, #19758, #73778, .T. ) ;
#41069 = CARTESIAN_POINT ( 'NONE',  ( 6.849999999999930367, 2.500000000000000000, -6.248780366869526759 ) ) ;
#41070 = DIRECTION ( 'NONE',  ( 0.000000000000000000, 0.000000000000000000, -1.000000000000000000 ) ) ;
#41071 = PLANE ( 'NONE',  #90337 ) ;
#41072 = AXIS2_PLACEMENT_3D ( 'NONE', #17566, #67959, #56203 ) ;
#41073 = DIRECTION ( 'NONE',  ( 0.000000000000000000, 1.000000000000000000, 0.000000000000000000 ) ) ;
#41074 = DIRECTION ( 'NONE',  ( -0.000000000000000000, 1.000000000000000000, -0.000000000000000000 ) ) ;
#41075 = AXIS2_PLACEMENT_3D ( 'NONE', #100614, #81626, #12235 ) ;
#41076 = VECTOR ( 'NONE', #119290, 1000.000000000000000 ) ;
#41077 = CARTESIAN_POINT ( 'NONE',  ( 11.89999999999990798, 2.500000000000000000, -4.576537180435977348 ) ) ;
#41078 = AXIS2_PLACEMENT_3D ( 'NONE', #45735, #126872, #35906 ) ;
#41079 = ORIENTED_EDGE ( 'NONE', *, *, #119425, .F. ) ;
#41080 = ORIENTED_EDGE ( 'NONE', *, *, #89569, .T. ) ;
#41081 = VERTEX_POINT ( 'NONE', #60141 ) ;
#41082 = EDGE_LOOP ( 'NONE', ( #57184, #125171 ) ) ;
#41083 = VERTEX_POINT ( 'NONE', #28081 ) ;
#41084 = LINE ( 'NONE', #71157, #25421 ) ;
#41085 = DIRECTION ( 'NONE',  ( 0.000000000000000000, 1.000000000000000000, 0.000000000000000000 ) ) ;
#41086 = ORIENTED_EDGE ( 'NONE', *, *, #30656, .F. ) ;
#41087 = FACE_BOUND ( 'NONE', #116870, .T. ) ;
#41089 = PLANE ( 'NONE',  #66638 ) ;
#41088 = AXIS2_PLACEMENT_3D ( 'NONE', #24458, #111040, #45397 ) ;
#41091 = VECTOR ( 'NONE', #44626, 1000.000000000000000 ) ;
#41090 = VECTOR ( 'NONE', #98089, 1000.000000000000000 ) ;
#41092 = ORIENTED_EDGE ( 'NONE', *, *, #105541, .T. ) ;
#41093 = LINE ( 'NONE', #71165, #65674 ) ;
#41094 = DIRECTION ( 'NONE',  ( 0.000000000000000000, 0.000000000000000000, 1.000000000000000000 ) ) ;
#41095 = CARTESIAN_POINT ( 'NONE',  ( -13.74999999999995381, 2.500000000000000000, -2.065063509461099844 ) ) ;
#41096 = DIRECTION ( 'NONE',  ( -0.000000000000000000, 1.000000000000000000, -0.000000000000000000 ) ) ;
#41097 = EDGE_LOOP ( 'NONE', ( #55106, #110945 ) ) ;
#41098 = DIRECTION ( 'NONE',  ( 0.000000000000000000, 1.000000000000000000, 0.000000000000000000 ) ) ;
#41099 = ADVANCED_FACE ( 'NONE', ( #18250 ), #117668, .T. ) ;
#41100 = ORIENTED_EDGE ( 'NONE', *, *, #1476, .F. ) ;
#41101 = ORIENTED_EDGE ( 'NONE', *, *, #66676, .T. ) ;
#41102 = CARTESIAN_POINT ( 'NONE',  ( 1.249999999999954259, 2.500000000000000000, -7.288010851410854585 ) ) ;
#41103 = CARTESIAN_POINT ( 'NONE',  ( 3.949999999999942446, 12.50000000000000000, -6.906693963081115939 ) ) ;
#41104 = ORIENTED_EDGE ( 'NONE', *, *, #61378, .T. ) ;
#41105 = CARTESIAN_POINT ( 'NONE',  ( 11.64999999999990621, 12.50000000000000000, 6.560283801567334372 ) ) ;
#41106 = DIRECTION ( 'NONE',  ( -0.000000000000000000, -1.000000000000000000, -0.000000000000000000 ) ) ;
#41107 = PLANE ( 'NONE',  #33183 ) ;
#41108 = DIRECTION ( 'NONE',  ( 0.000000000000000000, 0.000000000000000000, 1.000000000000000000 ) ) ;
#41109 = EDGE_LOOP ( 'NONE', ( #68134, #11217, #100187, #815 ) ) ;
#41110 = ADVANCED_FACE ( 'NONE', ( #48360 ), #42407, .T. ) ;
#41111 = DIRECTION ( 'NONE',  ( 0.000000000000000000, -0.000000000000000000, 1.000000000000000000 ) ) ;
#41112 = ORIENTED_EDGE ( 'NONE', *, *, #99912, .T. ) ;
#41113 = CARTESIAN_POINT ( 'NONE',  ( 11.24999999999994316, 2.500000000000000000, 2.165063509461097713 ) ) ;
#41114 = CIRCLE ( 'NONE', #28578, 0.1000000000000002554 ) ;
#41115 = EDGE_LOOP ( 'NONE', ( #36470, #31808, #107502, #22533 ) ) ;
#41116 = VECTOR ( 'NONE', #103463, 1000.000000000000000 ) ;
#41117 = CARTESIAN_POINT ( 'NONE',  ( -1.050000000000037792, 2.500000000000000000, 1.818653347947321475 ) ) ;
#41118 = EDGE_LOOP ( 'NONE', ( #125773, #117496, #24012, #116080 ) ) ;
#41119 = FACE_OUTER_BOUND ( 'NONE', #20242, .T. ) ;
#41120 = DIRECTION ( 'NONE',  ( 0.000000000000000000, 0.000000000000000000, 1.000000000000000000 ) ) ;
#41121 = DIRECTION ( 'NONE',  ( 0.000000000000000000, 1.000000000000000000, 0.000000000000000000 ) ) ;
#41122 = CARTESIAN_POINT ( 'NONE',  ( 13.09999999999990195, 2.500000000000000000, -4.576537180435978236 ) ) ;
#41123 = CARTESIAN_POINT ( 'NONE',  ( -9.400000000000009237, 2.500000000000000000, -4.576537180435973795 ) ) ;
#41124 = EDGE_LOOP ( 'NONE', ( #75075, #112180 ) ) ;
#41126 = VERTEX_POINT ( 'NONE', #119670 ) ;
#41125 = AXIS2_PLACEMENT_3D ( 'NONE', #91073, #70157, #41354 ) ;
#41127 = ORIENTED_EDGE ( 'NONE', *, *, #113243, .F. ) ;
#41128 = DIRECTION ( 'NONE',  ( 0.000000000000000000, 0.000000000000000000, 1.000000000000000000 ) ) ;
#41129 = DIRECTION ( 'NONE',  ( 0.000000000000000000, 1.000000000000000000, 0.000000000000000000 ) ) ;
#41130 = CARTESIAN_POINT ( 'NONE',  ( -11.24999999999996270, 2.500000000000000000, 2.065063509461097624 ) ) ;
#41132 = ORIENTED_EDGE ( 'NONE', *, *, #105328, .F. ) ;
#41131 = VERTEX_POINT ( 'NONE', #8421 ) ;
#41133 = ORIENTED_EDGE ( 'NONE', *, *, #61964, .T. ) ;
#41134 = DIRECTION ( 'NONE',  ( 0.000000000000000000, 0.000000000000000000, 1.000000000000000000 ) ) ;
#41135 = AXIS2_PLACEMENT_3D ( 'NONE', #83807, #84463, #3323 ) ;
#41136 = VERTEX_POINT ( 'NONE', #88261 ) ;
#41137 = FACE_OUTER_BOUND ( 'NONE', #114269, .T. ) ;
#41138 = DIRECTION ( 'NONE',  ( -0.000000000000000000, -1.000000000000000000, -0.000000000000000000 ) ) ;
#41140 = EDGE_CURVE ( 'NONE', #6762, #39561, #30026, .T. ) ;
#41139 = VECTOR ( 'NONE', #37263, 1000.000000000000000 ) ;
#41141 = CARTESIAN_POINT ( 'NONE',  ( 3.299999999999944755, 2.500000000000000000, -4.230127018922201998 ) ) ;
#41142 = CYLINDRICAL_SURFACE ( 'NONE', #8441, 7.500000000000000000 ) ;
#41143 = DIRECTION ( 'NONE',  ( 0.000000000000000000, 0.000000000000000000, 1.000000000000000000 ) ) ;
#41144 = DIRECTION ( 'NONE',  ( 0.000000000000000000, 0.000000000000000000, 1.000000000000000000 ) ) ;
#41145 = CARTESIAN_POINT ( 'NONE',  ( 7.049999999999928768, 2.500000000000000000, -2.165063509461101710 ) ) ;
#41146 = CARTESIAN_POINT ( 'NONE',  ( 13.34999999999989662, 12.50000000000000000, -2.165063509461101710 ) ) ;
#41147 = EDGE_CURVE ( 'NONE', #14617, #125159, #63320, .T. ) ;
#41148 = ORIENTED_EDGE ( 'NONE', *, *, #60509, .T. ) ;
#41149 = DIRECTION ( 'NONE',  ( -4.274815082592931898E-19, -0.9999939076577903929, -0.003490651415223739937 ) ) ;
#41150 = CARTESIAN_POINT ( 'NONE',  ( 10.19999999999991047, 2.500000000000000000, 4.776537180435972196 ) ) ;
#41151 = EDGE_CURVE ( 'NONE', #34347, #64996, #21479, .T. ) ;
#41152 = VERTEX_POINT ( 'NONE', #2462 ) ;
#41153 = ADVANCED_FACE ( 'NONE', ( #120966 ), #113488, .T. ) ;
#41154 = VERTEX_POINT ( 'NONE', #121599 ) ;
#41155 = EDGE_CURVE ( 'NONE', #60040, #42741, #17321, .T. ) ;
#41156 = CARTESIAN_POINT ( 'NONE',  ( 187.2552083336747444, 6.551208109652275624, -3.782341765624998686 ) ) ;
#41158 = EDGE_CURVE ( 'NONE', #59648, #62565, #616, .T. ) ;
#41157 = CARTESIAN_POINT ( 'NONE',  ( 8.549999999999922551, 2.500000000000000000, 2.611473670974873151 ) ) ;
#41159 = AXIS2_PLACEMENT_3D ( 'NONE', #76989, #34510, #54128 ) ;
#41160 = EDGE_CURVE ( 'NONE', #26349, #38979, #34086, .T. ) ;
#41161 = CARTESIAN_POINT ( 'NONE',  ( 11.64999999999990621, 2.500000000000000000, -2.165063509461101710 ) ) ;
#41163 = AXIS2_PLACEMENT_3D ( 'NONE', #110151, #47366, #108207 ) ;
#41162 = CARTESIAN_POINT ( 'NONE',  ( 179.5000000000000000, -0.6250000000000000000, 7.634788798650553154 ) ) ;
#41164 = CARTESIAN_POINT ( 'NONE',  ( -9.800000000000006040, 2.500000000000000000, 4.676537180435972552 ) ) ;
#41165 = CARTESIAN_POINT ( 'NONE',  ( -0.4500000000000402012, 2.500000000000000000, 6.495190528383297135 ) ) ;
#41166 = CIRCLE ( 'NONE', #93370, 0.1000000000000002554 ) ;
#41167 = CARTESIAN_POINT ( 'NONE',  ( -3.750000000000025757, 2.500000000000000000, -2.857883832488653741 ) ) ;
#41168 = CARTESIAN_POINT ( 'NONE',  ( -6.850000000000013856, 12.50000000000000000, 6.841600689897072485 ) ) ;
#41169 = EDGE_CURVE ( 'NONE', #118431, #90873, #15265, .T. ) ;
#41170 = CIRCLE ( 'NONE', #85047, 0.1000000000000002554 ) ;
#41172 = EDGE_CURVE ( 'NONE', #54506, #106259, #71883, .T. ) ;
#41171 = DIRECTION ( 'NONE',  ( 0.000000000000000000, -0.9999939076577903929, 0.003490651415223739937 ) ) ;
#41173 = ORIENTED_EDGE ( 'NONE', *, *, #89620, .F. ) ;
#41174 = EDGE_CURVE ( 'NONE', #67575, #113131, #42423, .T. ) ;
#41175 = ORIENTED_EDGE ( 'NONE', *, *, #74509, .T. ) ;
#41176 = CIRCLE ( 'NONE', #76746, 0.1000000000000002554 ) ;
#41177 = ORIENTED_EDGE ( 'NONE', *, *, #77983, .T. ) ;
#41178 = EDGE_LOOP ( 'NONE', ( #80358, #110549 ) ) ;
#41179 = CIRCLE ( 'NONE', #62095, 0.06509327318403745899 ) ;
#41180 = EDGE_LOOP ( 'NONE', ( #14933, #55977 ) ) ;
#41181 = DIRECTION ( 'NONE',  ( -4.274815082592931898E-19, -0.9999939076577903929, -0.003490651415223739937 ) ) ;
#41182 = DIRECTION ( 'NONE',  ( -0.000000000000000000, -1.000000000000000000, -0.000000000000000000 ) ) ;
#41183 = VECTOR ( 'NONE', #4148, 1000.000000000000000 ) ;
#41184 = VERTEX_POINT ( 'NONE', #53527 ) ;
#41185 = CARTESIAN_POINT ( 'NONE',  ( -15.59999999999998010, 2.500000000000000000, -0.2464101615137759549 ) ) ;
#41186 = DIRECTION ( 'NONE',  ( -0.000000000000000000, 1.000000000000000000, -0.000000000000000000 ) ) ;
#41187 = AXIS2_PLACEMENT_3D ( 'NONE', #21301, #111628, #61243 ) ;
#41188 = CARTESIAN_POINT ( 'NONE',  ( 0.6499999999999543920, 12.50000000000000000, 6.841600689897072485 ) ) ;
#41190 = EDGE_LOOP ( 'NONE', ( #15277, #100072, #11418, #110214 ) ) ;
#41189 = FACE_OUTER_BOUND ( 'NONE', #3267, .T. ) ;
#41191 = LINE ( 'NONE', #119713, #36904 ) ;
#41192 = CARTESIAN_POINT ( 'NONE',  ( -8.150000000000012790, 2.500000000000000000, -2.511473670974877948 ) ) ;
#41193 = VERTEX_POINT ( 'NONE', #10995 ) ;
#41194 = ORIENTED_EDGE ( 'NONE', *, *, #49863, .T. ) ;
#41195 = ORIENTED_EDGE ( 'NONE', *, *, #22832, .F. ) ;
#41196 = ORIENTED_EDGE ( 'NONE', *, *, #12869, .T. ) ;
#41197 = DIRECTION ( 'NONE',  ( 0.000000000000000000, 0.000000000000000000, 1.000000000000000000 ) ) ;
#41198 = AXIS2_PLACEMENT_3D ( 'NONE', #76358, #116261, #26606 ) ;
#41199 = DIRECTION ( 'NONE',  ( -0.000000000000000000, 1.000000000000000000, -0.000000000000000000 ) ) ;
#41200 = DIRECTION ( 'NONE',  ( -0.000000000000000000, 1.000000000000000000, -0.000000000000000000 ) ) ;
#41201 = FACE_OUTER_BOUND ( 'NONE', #28795, .T. ) ;
#41202 = EDGE_LOOP ( 'NONE', ( #31483, #120074 ) ) ;
#41203 = FACE_OUTER_BOUND ( 'NONE', #45752, .T. ) ;
#41204 = CARTESIAN_POINT ( 'NONE',  ( -7.050000000000013145, 2.500000000000000000, 6.395190528383296602 ) ) ;
#41205 = DIRECTION ( 'NONE',  ( 0.000000000000000000, 1.000000000000000000, 0.000000000000000000 ) ) ;
#41206 = DIRECTION ( 'NONE',  ( 0.000000000000000000, 1.000000000000000000, 0.000000000000000000 ) ) ;
#41207 = ADVANCED_FACE ( 'NONE', ( #90862 ), #48758, .T. ) ;
#41208 = EDGE_CURVE ( 'NONE', #109623, #100170, #82352, .T. ) ;
#41209 = ORIENTED_EDGE ( 'NONE', *, *, #92992, .F. ) ;
#41210 = VECTOR ( 'NONE', #96779, 1000.000000000000000 ) ;
#41211 = AXIS2_PLACEMENT_3D ( 'NONE', #30409, #67715, #129258 ) ;
#41212 = EDGE_CURVE ( 'NONE', #54324, #66570, #107230, .T. ) ;
#41213 = EDGE_LOOP ( 'NONE', ( #54822, #119634 ) ) ;
#41214 = ORIENTED_EDGE ( 'NONE', *, *, #92085, .T. ) ;
#41215 = DIRECTION ( 'NONE',  ( 0.000000000000000000, 0.000000000000000000, 1.000000000000000000 ) ) ;
#41216 = DIRECTION ( 'NONE',  ( -0.000000000000000000, 1.000000000000000000, -0.000000000000000000 ) ) ;
#41217 = FACE_BOUND ( 'NONE', #124115, .T. ) ;
#41218 = CARTESIAN_POINT ( 'NONE',  ( 13.34999999999989662, 2.500000000000000000, -2.265063509461101798 ) ) ;
#41219 = DIRECTION ( 'NONE',  ( -0.000000000000000000, 1.000000000000000000, -0.000000000000000000 ) ) ;
#41220 = EDGE_CURVE ( 'NONE', #71397, #88786, #50813, .T. ) ;
#41222 = CIRCLE ( 'NONE', #16126, 0.1000000000000002554 ) ;
#41221 = VECTOR ( 'NONE', #49087, 1000.000000000000000 ) ;
#41223 = CARTESIAN_POINT ( 'NONE',  ( -4.350000000000027178, 2.500000000000000000, -6.248780366869526759 ) ) ;
#41224 = CARTESIAN_POINT ( 'NONE',  ( -12.09999999999999609, 2.500000000000000000, -5.122947341949751987 ) ) ;
#41225 = FACE_OUTER_BOUND ( 'NONE', #19175, .T. ) ;
#41226 = DIRECTION ( 'NONE',  ( 0.000000000000000000, 0.000000000000000000, 1.000000000000000000 ) ) ;
#41227 = EDGE_LOOP ( 'NONE', ( #56560, #110413 ) ) ;
#41228 = AXIS2_PLACEMENT_3D ( 'NONE', #99925, #102496, #69816 ) ;
#41229 = DIRECTION ( 'NONE',  ( 0.000000000000000000, 0.000000000000000000, 1.000000000000000000 ) ) ;
#41230 = CARTESIAN_POINT ( 'NONE',  ( 9.999999999999912959, 2.500000000000000000, 3.637306695894644726 ) ) ;
#41231 = ORIENTED_EDGE ( 'NONE', *, *, #113389, .T. ) ;
#41232 = VERTEX_POINT ( 'NONE', #43084 ) ;
#41233 = FACE_OUTER_BOUND ( 'NONE', #59110, .T. ) ;
#41234 = CARTESIAN_POINT ( 'NONE',  ( 9.149999999999920419, 12.50000000000000000, -7.122917578226816815 ) ) ;
#41235 = EDGE_CURVE ( 'NONE', #20148, #13812, #62065, .T. ) ;
#41236 = FACE_BOUND ( 'NONE', #27574, .T. ) ;
#41237 = CARTESIAN_POINT ( 'NONE',  ( 2.099999999999948574, 12.50000000000000000, 4.265033745738159077 ) ) ;
#41238 = FACE_OUTER_BOUND ( 'NONE', #49521, .T. ) ;
#41239 = VERTEX_POINT ( 'NONE', #22791 ) ;
#41240 = DIRECTION ( 'NONE',  ( -0.000000000000000000, -1.000000000000000000, -0.000000000000000000 ) ) ;
#41241 = CARTESIAN_POINT ( 'NONE',  ( 184.4166666666666856, 6.668395609140176816, 3.850000000000000977 ) ) ;
#41242 = AXIS2_PLACEMENT_3D ( 'NONE', #29502, #10487, #70708 ) ;
#41243 = ORIENTED_EDGE ( 'NONE', *, *, #63912, .F. ) ;
#41244 = DIRECTION ( 'NONE',  ( 0.000000000000000000, 0.000000000000000000, 1.000000000000000000 ) ) ;
#41245 = CONICAL_SURFACE ( 'NONE', #101867, 0.1000000000000002554, 0.003490658503988666988 ) ;
#41246 = DIRECTION ( 'NONE',  ( -1.000000000000000000, -0.000000000000000000, -0.000000000000000000 ) ) ;
#41247 = AXIS2_PLACEMENT_3D ( 'NONE', #84003, #93840, #84662 ) ;
#41248 = EDGE_CURVE ( 'NONE', #57762, #114896, #92565, .T. ) ;
#41249 = CARTESIAN_POINT ( 'NONE',  ( -2.100000000000033840, 2.500000000000000000, 3.637306695894644726 ) ) ;
#41250 = LINE ( 'NONE', #121716, #86573 ) ;
#41251 = VECTOR ( 'NONE', #95812, 1000.000000000000000 ) ;
#41252 = ORIENTED_EDGE ( 'NONE', *, *, #2983, .F. ) ;
#41253 = AXIS2_PLACEMENT_3D ( 'NONE', #36684, #107335, #66118 ) ;
#41254 = CARTESIAN_POINT ( 'NONE',  ( 11.24999999999990585, 2.500000000000000000, -5.702370205355749455 ) ) ;
#41255 = CARTESIAN_POINT ( 'NONE',  ( -12.49999999999999467, 2.500000000000000000, 0.6928203230275535862 ) ) ;
#41256 = CARTESIAN_POINT ( 'NONE',  ( 4.399999999999937295, 2.500000000000000000, 4.776537180435972196 ) ) ;
#41257 = ORIENTED_EDGE ( 'NONE', *, *, #38427, .T. ) ;
#41258 = ORIENTED_EDGE ( 'NONE', *, *, #32348, .T. ) ;
#41259 = CIRCLE ( 'NONE', #85146, 0.06509327318403745899 ) ;
#41260 = ADVANCED_FACE ( 'NONE', ( #113072 ), #32045, .T. ) ;
#41261 =( BOUNDED_CURVE ( )  B_SPLINE_CURVE ( 2, ( #36698, #107347, #97525, #7852, #5905, #45868, #116520 ),
 .UNSPECIFIED., .F., .F. ) 
 B_SPLINE_CURVE_WITH_KNOTS ( ( 3, 2, 2, 3 ),
 ( 0.2857142857142859760, 0.3095238095238098119, 0.3333333333333335924, 0.3571428571428574283 ),
 .UNSPECIFIED. ) 
 CURVE ( )  GEOMETRIC_REPRESENTATION_ITEM ( )  RATIONAL_B_SPLINE_CURVE ( ( 0.9999999999999984457, 0.8660254037844402619, 1.000000000000000000, 0.8660254037844387076, 1.000000000000000000, 0.8660254037844371533, 1.000000000000001554 ) ) 
 REPRESENTATION_ITEM ( '' )  );
#41262 = LINE ( 'NONE', #51716, #7495 ) ;
#41263 = ORIENTED_EDGE ( 'NONE', *, *, #38307, .F. ) ;
#41264 = DIRECTION ( 'NONE',  ( 0.000000000000000000, 0.000000000000000000, 1.000000000000000000 ) ) ;
#41265 = DIRECTION ( 'NONE',  ( 0.000000000000000000, 0.000000000000000000, 1.000000000000000000 ) ) ;
#41267 = CIRCLE ( 'NONE', #124878, 0.1000000000000002554 ) ;
#41266 = AXIS2_PLACEMENT_3D ( 'NONE', #108877, #67668, #97142 ) ;
#41268 = DIRECTION ( 'NONE',  ( -4.274815082592931898E-19, -0.9999939076577903929, -0.003490651415223739937 ) ) ;
#41269 = ORIENTED_EDGE ( 'NONE', *, *, #112257, .F. ) ;
#41270 = PLANE ( 'NONE',  #5703 ) ;
#41271 = FACE_OUTER_BOUND ( 'NONE', #14682, .T. ) ;
#41272 = LINE ( 'NONE', #117863, #105013 ) ;
#41273 = CARTESIAN_POINT ( 'NONE',  ( -1.050000000000038236, 2.500000000000000000, -1.918653347947326004 ) ) ;
#41274 = DIRECTION ( 'NONE',  ( 0.000000000000000000, 1.000000000000000000, 0.000000000000000000 ) ) ;
#41275 = CARTESIAN_POINT ( 'NONE',  ( -11.89999999999999680, 12.50000000000000000, -4.676537180435976104 ) ) ;
#41276 = EDGE_LOOP ( 'NONE', ( #40181, #120314, #28938, #1123 ) ) ;
#41277 = ORIENTED_EDGE ( 'NONE', *, *, #66099, .F. ) ;
#41278 = DIRECTION ( 'NONE',  ( 0.000000000000000000, 1.000000000000000000, 0.000000000000000000 ) ) ;
#41279 = ORIENTED_EDGE ( 'NONE', *, *, #107933, .F. ) ;
#41280 = DIRECTION ( 'NONE',  ( -4.274815082592931898E-19, -0.9999939076577903929, -0.003490651415223739937 ) ) ;
#41282 = ORIENTED_EDGE ( 'NONE', *, *, #1550, .F. ) ;
#41281 = EDGE_LOOP ( 'NONE', ( #19832, #14094, #70699, #47544 ) ) ;
#41283 = ORIENTED_EDGE ( 'NONE', *, *, #56687, .T. ) ;
#41284 = AXIS2_PLACEMENT_3D ( 'NONE', #16882, #14326, #15618 ) ;
#41285 = LINE ( 'NONE', #53661, #85556 ) ;
#41286 = DIRECTION ( 'NONE',  ( -0.000000000000000000, -1.000000000000000000, -0.000000000000000000 ) ) ;
#41287 = DIRECTION ( 'NONE',  ( -0.000000000000000000, -1.000000000000000000, -0.000000000000000000 ) ) ;
#41288 = EDGE_CURVE ( 'NONE', #3112, #111831, #61279, .T. ) ;
#41289 = DIRECTION ( 'NONE',  ( 0.000000000000000000, -0.9999939076577903929, 0.003490651415223739937 ) ) ;
#41290 = CARTESIAN_POINT ( 'NONE',  ( -5.400000000000019895, 12.50000000000000000, -0.6928203230275541413 ) ) ;
#41291 = DIRECTION ( 'NONE',  ( 1.000000000000000000, 0.000000000000000000, 0.000000000000000000 ) ) ;
#41292 = FACE_OUTER_BOUND ( 'NONE', #78652, .T. ) ;
#41293 = CARTESIAN_POINT ( 'NONE',  ( 5.449999999999937117, 2.500000000000000000, -6.495190528383302464 ) ) ;
#41294 = DIRECTION ( 'NONE',  ( 0.000000000000000000, 1.000000000000000000, 0.000000000000000000 ) ) ;
#41295 = EDGE_CURVE ( 'NONE', #85147, #31487, #126000, .T. ) ;
#41297 = VERTEX_POINT ( 'NONE', #18671 ) ;
#41296 = AXIS2_PLACEMENT_3D ( 'NONE', #21809, #22460, #51910 ) ;
#41298 = CIRCLE ( 'NONE', #126965, 0.06509327318403745899 ) ;
#41299 = CARTESIAN_POINT ( 'NONE',  ( -0.6500000000000394351, 12.50000000000000000, 2.511473670974873507 ) ) ;
#41300 = ADVANCED_FACE ( 'NONE', ( #58611 ), #99824, .T. ) ;
#41301 = VERTEX_POINT ( 'NONE', #38996 ) ;
#41302 = EDGE_CURVE ( 'NONE', #66032, #112123, #96752, .T. ) ;
#41303 = ORIENTED_EDGE ( 'NONE', *, *, #23535, .F. ) ;
#41304 = EDGE_CURVE ( 'NONE', #22551, #82878, #77992, .T. ) ;
#41305 = DIRECTION ( 'NONE',  ( 0.000000000000000000, 0.000000000000000000, -1.000000000000000000 ) ) ;
#41306 = ADVANCED_FACE ( 'NONE', ( #119436 ), #59915, .T. ) ;
#41307 = FACE_OUTER_BOUND ( 'NONE', #118539, .T. ) ;
#41309 = VECTOR ( 'NONE', #126811, 1000.000000000000000 ) ;
#41308 = CIRCLE ( 'NONE', #76796, 0.06509327318403745899 ) ;
#41310 = CARTESIAN_POINT ( 'NONE',  ( -12.89999999999999147, 2.500000000000000000, -5.022947341949751454 ) ) ;
#41311 = CARTESIAN_POINT ( 'NONE',  ( 1.649999999999949729, 12.50000000000000000, 5.802370205355744659 ) ) ;
#41312 = DIRECTION ( 'NONE',  ( 0.000000000000000000, 1.000000000000000000, 0.000000000000000000 ) ) ;
#41313 = EDGE_CURVE ( 'NONE', #74338, #31381, #109287, .T. ) ;
#41314 = CARTESIAN_POINT ( 'NONE',  ( -11.44999999999999751, 2.500000000000000000, -2.511473670974873951 ) ) ;
#41315 = ORIENTED_EDGE ( 'NONE', *, *, #101275, .T. ) ;
#41316 = ADVANCED_FACE ( 'NONE', ( #69709 ), #119849, .T. ) ;
#41317 = EDGE_CURVE ( 'NONE', #114882, #80384, #29879, .T. ) ;
#41318 = AXIS2_PLACEMENT_3D ( 'NONE', #117432, #106357, #38273 ) ;
#41319 = EDGE_CURVE ( 'NONE', #92599, #45421, #107326, .T. ) ;
#41320 = ORIENTED_EDGE ( 'NONE', *, *, #63860, .T. ) ;
#41321 = VECTOR ( 'NONE', #120595, 1000.000000000000000 ) ;
#41322 = EDGE_CURVE ( 'NONE', #59852, #109430, #78257, .T. ) ;
#41323 = ORIENTED_EDGE ( 'NONE', *, *, #2352, .F. ) ;
#41324 = DIRECTION ( 'NONE',  ( 0.000000000000000000, 1.000000000000000000, 0.000000000000000000 ) ) ;
#41325 = VERTEX_POINT ( 'NONE', #50095 ) ;
#41326 = ORIENTED_EDGE ( 'NONE', *, *, #32501, .F. ) ;
#41327 = EDGE_CURVE ( 'NONE', #107807, #17323, #71004, .T. ) ;
#41328 = DIRECTION ( 'NONE',  ( -4.274815082592931898E-19, -0.9999939076577903929, -0.003490651415223739937 ) ) ;
#41329 = DIRECTION ( 'NONE',  ( 0.000000000000000000, 0.000000000000000000, 1.000000000000000000 ) ) ;
#41330 = AXIS2_PLACEMENT_3D ( 'NONE', #74893, #6753, #96441 ) ;
#41331 = DIRECTION ( 'NONE',  ( -0.000000000000000000, -1.000000000000000000, -0.000000000000000000 ) ) ;
#41332 = LINE ( 'NONE', #51780, #79973 ) ;
#41333 = CARTESIAN_POINT ( 'NONE',  ( 17.50000000000000000, -2.500000000000000000, 4.000000000000001776 ) ) ;
#41334 = ORIENTED_EDGE ( 'NONE', *, *, #75222, .F. ) ;
#41335 = CARTESIAN_POINT ( 'NONE',  ( 6.849999999999929479, 2.500000000000000000, -2.511473670974877948 ) ) ;
#41336 = DIRECTION ( 'NONE',  ( 0.000000000000000000, 0.000000000000000000, -1.000000000000000000 ) ) ;
#41337 = CARTESIAN_POINT ( 'NONE',  ( -4.550000000000026468, 12.50000000000000000, -6.495190528383302464 ) ) ;
#41338 = CARTESIAN_POINT ( 'NONE',  ( 4.149999999999941735, 2.500000000000000000, -5.802370205355749988 ) ) ;
#41339 = AXIS2_PLACEMENT_3D ( 'NONE', #58806, #40469, #79102 ) ;
#41340 = AXIS2_PLACEMENT_3D ( 'NONE', #97369, #108471, #18799 ) ;
#41341 = DIRECTION ( 'NONE',  ( 0.000000000000000000, 0.000000000000000000, -1.000000000000000000 ) ) ;
#41342 = ORIENTED_EDGE ( 'NONE', *, *, #46752, .T. ) ;
#41343 = CIRCLE ( 'NONE', #45446, 0.06509327318403745899 ) ;
#41344 = VERTEX_POINT ( 'NONE', #40258 ) ;
#41345 = ORIENTED_EDGE ( 'NONE', *, *, #20910, .F. ) ;
#41346 = DIRECTION ( 'NONE',  ( 0.000000000000000000, -1.000000000000000000, 0.000000000000000000 ) ) ;
#41347 = AXIS2_PLACEMENT_3D ( 'NONE', #43997, #111416, #13217 ) ;
#41348 = VERTEX_POINT ( 'NONE', #98502 ) ;
#41349 = AXIS2_PLACEMENT_3D ( 'NONE', #22594, #33055, #992 ) ;
#41350 = CARTESIAN_POINT ( 'NONE',  ( 16.89731025888664462, -0.9183091266721399304, 5.698390440797583167 ) ) ;
#41351 = LINE ( 'NONE', #91716, #29332 ) ;
#41352 = AXIS2_PLACEMENT_3D ( 'NONE', #120391, #21541, #10426 ) ;
#41353 = VERTEX_POINT ( 'NONE', #8837 ) ;
#41354 = DIRECTION ( 'NONE',  ( 0.000000000000000000, 0.000000000000000000, -1.000000000000000000 ) ) ;
#41356 = CIRCLE ( 'NONE', #114484, 0.06509327318403745899 ) ;
#41355 = CARTESIAN_POINT ( 'NONE',  ( 6.249999999999928946, 12.50000000000000000, 2.857883832488649301 ) ) ;
#41357 = DIRECTION ( 'NONE',  ( -0.000000000000000000, 1.000000000000000000, -0.000000000000000000 ) ) ;
#41358 = DIRECTION ( 'NONE',  ( 0.000000000000000000, 1.000000000000000000, 0.000000000000000000 ) ) ;
#41359 = ADVANCED_FACE ( 'NONE', ( #48792 ), #80177, .T. ) ;
#41361 = AXIS2_PLACEMENT_3D ( 'NONE', #119904, #99627, #40724 ) ;
#41360 = PRESENTATION_LAYER_ASSIGNMENT (  '', '', ( #70589 ) ) ;
#41362 = FACE_OUTER_BOUND ( 'NONE', #84385, .T. ) ;
#41363 = EDGE_CURVE ( 'NONE', #30275, #29752, #122003, .T. ) ;
#41364 = ORIENTED_EDGE ( 'NONE', *, *, #58774, .T. ) ;
#41365 = ORIENTED_EDGE ( 'NONE', *, *, #31586, .F. ) ;
#41366 = DIRECTION ( 'NONE',  ( 0.000000000000000000, 1.000000000000000000, 0.000000000000000000 ) ) ;
#41367 = CARTESIAN_POINT ( 'NONE',  ( 3.549999999999942979, 2.500000000000000000, 1.818653347947321475 ) ) ;
#41368 = CARTESIAN_POINT ( 'NONE',  ( 1.449999999999951328, 2.500000000000000000, 2.411473670974873862 ) ) ;
#41369 = ADVANCED_FACE ( 'NONE', ( #50711 ), #84344, .T. ) ;
#41370 = DIRECTION ( 'NONE',  ( 0.000000000000000000, -0.000000000000000000, 1.000000000000000000 ) ) ;
#41371 = ORIENTED_EDGE ( 'NONE', *, *, #5384, .F. ) ;
#41372 = VERTEX_POINT ( 'NONE', #110905 ) ;
#41373 = DIRECTION ( 'NONE',  ( 0.000000000000000000, 0.000000000000000000, -1.000000000000000000 ) ) ;
#41374 = CARTESIAN_POINT ( 'NONE',  ( -13.09999999999999254, 12.50000000000000000, -4.611443907251937091 ) ) ;
#41375 = CARTESIAN_POINT ( 'NONE',  ( 0.5999999999999547917, 2.500000000000000000, 3.983716857408420076 ) ) ;
#41376 = FACE_OUTER_BOUND ( 'NONE', #110535, .T. ) ;
#41377 = ORIENTED_EDGE ( 'NONE', *, *, #9682, .F. ) ;
#41378 = CARTESIAN_POINT ( 'NONE',  ( 0.4499999999999573785, 12.50000000000000000, -6.495190528383302464 ) ) ;
#41379 = DIRECTION ( 'NONE',  ( -0.000000000000000000, -1.000000000000000000, -0.000000000000000000 ) ) ;
#41380 = EDGE_LOOP ( 'NONE', ( #112868, #25580, #3949, #30135 ) ) ;
#41381 = CARTESIAN_POINT ( 'NONE',  ( 17.50000000000000000, 2.500000000000000000, 2.922290670087886344 ) ) ;
#41382 = ORIENTED_EDGE ( 'NONE', *, *, #101984, .F. ) ;
#41383 = DIRECTION ( 'NONE',  ( -4.274815082592931898E-19, -0.9999939076577903929, -0.003490651415223739937 ) ) ;
#41384 = AXIS2_PLACEMENT_3D ( 'NONE', #63005, #90523, #102921 ) ;
#41385 = ORIENTED_EDGE ( 'NONE', *, *, #127999, .T. ) ;
#41386 = AXIS2_PLACEMENT_3D ( 'NONE', #30253, #47944, #108775 ) ;
#41387 = ORIENTED_EDGE ( 'NONE', *, *, #4228, .T. ) ;
#41388 = LINE ( 'NONE', #79373, #113302 ) ;
#41389 = DIRECTION ( 'NONE',  ( -0.000000000000000000, 1.000000000000000000, -0.000000000000000000 ) ) ;
#41390 = ORIENTED_EDGE ( 'NONE', *, *, #4668, .F. ) ;
#41391 = EDGE_LOOP ( 'NONE', ( #79356, #25237 ) ) ;
#41392 = CARTESIAN_POINT ( 'NONE',  ( -9.550000000000007816, 12.50000000000000000, -6.495190528383297135 ) ) ;
#41393 = CARTESIAN_POINT ( 'NONE',  ( -1.850000000000033396, 12.50000000000000000, -1.883746621131363375 ) ) ;
#41394 = ORIENTED_EDGE ( 'NONE', *, *, #101029, .F. ) ;
#41395 = AXIS2_PLACEMENT_3D ( 'NONE', #122434, #22316, #83159 ) ;
#41397 = ADVANCED_FACE ( 'NONE', ( #21243 ), #61181, .T. ) ;
#41396 = DIRECTION ( 'NONE',  ( 0.000000000000000000, -0.9999939076577903929, 0.003490651415223739937 ) ) ;
#41398 = CARTESIAN_POINT ( 'NONE',  ( 185.1093750003413732, 9.264065473108010111E-16, -7.564683531250000925 ) ) ;
#41399 = CIRCLE ( 'NONE', #51854, 0.06509327318403745899 ) ;
#41400 = CARTESIAN_POINT ( 'NONE',  ( -5.400000000000023448, 2.500000000000000000, -4.230127018922201998 ) ) ;
#41401 = CARTESIAN_POINT ( 'NONE',  ( 13.14999999999990088, 2.500000000000000000, 1.718653347947321386 ) ) ;
#41402 = CARTESIAN_POINT ( 'NONE',  ( -9.600000000000008527, 2.500000000000000000, -4.330127018922197202 ) ) ;
#41403 = CARTESIAN_POINT ( 'NONE',  ( 14.14999999999989733, 2.500000000000000000, 2.857883832488649301 ) ) ;
#41404 = DIRECTION ( 'NONE',  ( -4.274815082592931898E-19, -0.9999939076577903929, -0.003490651415223739937 ) ) ;
#41405 = CONICAL_SURFACE ( 'NONE', #51860, 0.1000000000000002554, 0.003490658503988666988 ) ;
#41406 = ORIENTED_EDGE ( 'NONE', *, *, #37621, .F. ) ;
#41407 = ORIENTED_EDGE ( 'NONE', *, *, #35118, .F. ) ;
#41408 = CARTESIAN_POINT ( 'NONE',  ( -14.59999999999998366, 2.500000000000000000, 0.5928203230275517210 ) ) ;
#41409 = ORIENTED_EDGE ( 'NONE', *, *, #29196, .T. ) ;
#41410 = DIRECTION ( 'NONE',  ( -0.000000000000000000, 1.000000000000000000, -0.000000000000000000 ) ) ;
#41411 = LINE ( 'NONE', #81325, #38741 ) ;
#41412 = ADVANCED_FACE ( 'NONE', ( #90604 ), #9128, .T. ) ;
#41413 = AXIS2_PLACEMENT_3D ( 'NONE', #25192, #65109, #73645 ) ;
#41414 = DIRECTION ( 'NONE',  ( -0.000000000000000000, 1.000000000000000000, -0.000000000000000000 ) ) ;
#41416 = ORIENTED_EDGE ( 'NONE', *, *, #71906, .T. ) ;
#41415 = VERTEX_POINT ( 'NONE', #40899 ) ;
#41417 = FACE_BOUND ( 'NONE', #123490, .T. ) ;
#41418 = EDGE_LOOP ( 'NONE', ( #55848, #78269, #78586, #5914 ) ) ;
#41419 = EDGE_CURVE ( 'NONE', #36193, #94775, #50902, .T. ) ;
#41420 = LINE ( 'NONE', #31584, #34625 ) ;
#41421 = LINE ( 'NONE', #89846, #24972 ) ;
#41422 = CARTESIAN_POINT ( 'NONE',  ( 0.8499999999999545697, 12.50000000000000000, -1.472243186433550122 ) ) ;
#41423 = CIRCLE ( 'NONE', #18416, 0.06509327318403745899 ) ;
#41424 = FACE_OUTER_BOUND ( 'NONE', #116679, .T. ) ;
#41425 = PLANE ( 'NONE',  #112005 ) ;
#41426 = DIRECTION ( 'NONE',  ( -0.000000000000000000, -1.000000000000000000, -0.000000000000000000 ) ) ;
#41427 = CIRCLE ( 'NONE', #14194, 0.06509327318403745899 ) ;
#41428 = DIRECTION ( 'NONE',  ( 0.000000000000000000, 0.000000000000000000, -1.000000000000000000 ) ) ;
#41429 = CARTESIAN_POINT ( 'NONE',  ( 9.149999999999920419, 2.500000000000000000, -5.902370205355750521 ) ) ;
#41430 = ADVANCED_FACE ( 'NONE', ( #67747 ), #79513, .T. ) ;
#41431 = CARTESIAN_POINT ( 'NONE',  ( 1.699999999999951994, 2.500000000000000000, -4.430127018922202176 ) ) ;
#41432 = DIRECTION ( 'NONE',  ( 0.000000000000000000, -0.000000000000000000, 1.000000000000000000 ) ) ;
#41433 = CIRCLE ( 'NONE', #91583, 0.09999999999999999167 ) ;
#41434 = CIRCLE ( 'NONE', #58149, 0.1000000000000000472 ) ;
#41435 = DIRECTION ( 'NONE',  ( 0.000000000000000000, 1.000000000000000000, 0.000000000000000000 ) ) ;
#41436 = ORIENTED_EDGE ( 'NONE', *, *, #127668, .F. ) ;
#41438 = ORIENTED_EDGE ( 'NONE', *, *, #70368, .F. ) ;
#41437 = CIRCLE ( 'NONE', #95709, 0.06509327318403745899 ) ;
#41439 = VERTEX_POINT ( 'NONE', #70331 ) ;
#41440 = ORIENTED_EDGE ( 'NONE', *, *, #119334, .F. ) ;
#41441 = LINE ( 'NONE', #51895, #110336 ) ;
#41442 = DIRECTION ( 'NONE',  ( -0.000000000000000000, 1.000000000000000000, -0.000000000000000000 ) ) ;
#41444 = VERTEX_POINT ( 'NONE', #27816 ) ;
#41443 = EDGE_LOOP ( 'NONE', ( #108555, #46555 ) ) ;
#41446 = ORIENTED_EDGE ( 'NONE', *, *, #123574, .F. ) ;
#41445 = CIRCLE ( 'NONE', #114562, 0.09999999999999999167 ) ;
#41447 = PLANE ( 'NONE',  #25042 ) ;
#41448 = CARTESIAN_POINT ( 'NONE',  ( 3.349999999999944578, 12.50000000000000000, -5.802370205355749988 ) ) ;
#41449 = FILL_AREA_STYLE ('',( #21134 ) ) ;
#41450 = CARTESIAN_POINT ( 'NONE',  ( -8.749999999999976907, 2.500000000000000000, -6.495190528383297135 ) ) ;
#41451 = DIRECTION ( 'NONE',  ( 0.000000000000000000, 0.000000000000000000, 1.000000000000000000 ) ) ;
#41452 = DIRECTION ( 'NONE',  ( -0.000000000000000000, -1.000000000000000000, -0.000000000000000000 ) ) ;
#41453 = DIRECTION ( 'NONE',  ( -0.000000000000000000, 1.000000000000000000, -0.000000000000000000 ) ) ;
#41454 = VECTOR ( 'NONE', #6409, 1000.000000000000000 ) ;
#41455 = VERTEX_POINT ( 'NONE', #107679 ) ;
#41456 = DIRECTION ( 'NONE',  ( -0.000000000000000000, -1.000000000000000000, -0.000000000000000000 ) ) ;
#41457 = ORIENTED_EDGE ( 'NONE', *, *, #29071, .F. ) ;
#41458 = ADVANCED_FACE ( 'NONE', ( #17995 ), #48119, .T. ) ;
#41460 = AXIS2_PLACEMENT_3D ( 'NONE', #72744, #23001, #72105 ) ;
#41459 = CIRCLE ( 'NONE', #123003, 0.06509327318403745899 ) ;
#41461 = VERTEX_POINT ( 'NONE', #59241 ) ;
#41462 = ORIENTED_EDGE ( 'NONE', *, *, #21227, .F. ) ;
#41463 = CARTESIAN_POINT ( 'NONE',  ( 7.899999999999923084, 2.500000000000000000, -0.7928203230275543412 ) ) ;
#41464 = ORIENTED_EDGE ( 'NONE', *, *, #78073, .T. ) ;
#41465 = EDGE_CURVE ( 'NONE', #89903, #129360, #127956, .T. ) ;
#41466 = ORIENTED_EDGE ( 'NONE', *, *, #81890, .T. ) ;
#41467 = VERTEX_POINT ( 'NONE', #118134 ) ;
#41468 = EDGE_CURVE ( 'NONE', #118944, #81926, #9021, .T. ) ;
#41469 = DIRECTION ( 'NONE',  ( -0.000000000000000000, 1.000000000000000000, -0.000000000000000000 ) ) ;
#41470 = FILL_AREA_STYLE ('',( #62387 ) ) ;
#41471 = DIRECTION ( 'NONE',  ( 0.000000000000000000, 0.000000000000000000, 1.000000000000000000 ) ) ;
#41472 = PLANE ( 'NONE',  #31606 ) ;
#41473 = DIRECTION ( 'NONE',  ( 0.000000000000000000, 0.000000000000000000, 1.000000000000000000 ) ) ;
#41474 = EDGE_CURVE ( 'NONE', #86459, #119361, #38300, .T. ) ;
#41475 = DIRECTION ( 'NONE',  ( 0.000000000000000000, 0.000000000000000000, -1.000000000000000000 ) ) ;
#41476 = EDGE_CURVE ( 'NONE', #76693, #93836, #105274, .T. ) ;
#41477 = EDGE_CURVE ( 'NONE', #113011, #110791, #279, .T. ) ;
#41478 = CARTESIAN_POINT ( 'NONE',  ( 187.5000000000000000, 1.500000000000000000, 6.000000000000000000 ) ) ;
#41479 = EDGE_LOOP ( 'NONE', ( #29574, #35182 ) ) ;
#41481 = DIRECTION ( 'NONE',  ( -0.000000000000000000, -1.000000000000000000, -0.000000000000000000 ) ) ;
#41480 = CIRCLE ( 'NONE', #74908, 0.06509327318403745899 ) ;
#41482 = ADVANCED_FACE ( 'NONE', ( #20588 ), #101067, .T. ) ;
#41483 = VERTEX_POINT ( 'NONE', #129276 ) ;
#41484 = CARTESIAN_POINT ( 'NONE',  ( -7.900000000000014566, 2.500000000000000000, -3.637306695894650055 ) ) ;
#41485 = PLANE ( 'NONE',  #12699 ) ;
#41486 = CONICAL_SURFACE ( 'NONE', #3800, 0.09999999999999982514, 0.003490658503988666988 ) ;
#41487 = AXIS2_PLACEMENT_3D ( 'NONE', #528, #29375, #119034 ) ;
#41488 = VERTEX_POINT ( 'NONE', #128635 ) ;
#41489 = DIRECTION ( 'NONE',  ( 0.000000000000000000, 1.000000000000000000, 0.000000000000000000 ) ) ;
#41490 = ADVANCED_FACE ( 'NONE', ( #60534 ), #44641, .T. ) ;
#41491 = VERTEX_POINT ( 'NONE', #29132 ) ;
#41492 = ADVANCED_FACE ( 'NONE', ( #69027 ), #108941, .T. ) ;
#41493 = CARTESIAN_POINT ( 'NONE',  ( 6.849999999999927702, 12.50000000000000000, 1.818653347947321475 ) ) ;
#41494 = CONICAL_SURFACE ( 'NONE', #45677, 0.09999999999999982514, 0.003490658503988666988 ) ;
#41495 = AXIS2_PLACEMENT_3D ( 'NONE', #63979, #32618, #81053 ) ;
#41496 = PLANE ( 'NONE',  #88581 ) ;
#41497 = ORIENTED_EDGE ( 'NONE', *, *, #46912, .T. ) ;
#41498 = ORIENTED_EDGE ( 'NONE', *, *, #108825, .F. ) ;
#41499 = CARTESIAN_POINT ( 'NONE',  ( -11.25000000000000000, 12.50000000000000000, -2.922977105672687426 ) ) ;
#41500 = DIRECTION ( 'NONE',  ( 0.000000000000000000, 0.000000000000000000, 1.000000000000000000 ) ) ;
#41501 = CARTESIAN_POINT ( 'NONE',  ( 184.5468750003414300, -8.734944146203032389, -1.604583208406768146E-15 ) ) ;
#41502 = FACE_OUTER_BOUND ( 'NONE', #67553, .T. ) ;
#41503 = CONICAL_SURFACE ( 'NONE', #24748, 0.09999999999999982514, 0.003490658503988666988 ) ;
#41504 = CARTESIAN_POINT ( 'NONE',  ( -4.350000000000023626, 2.500000000000000000, 1.918653347947321564 ) ) ;
#41505 = AXIS2_PLACEMENT_3D ( 'NONE', #30102, #88329, #60208 ) ;
#41506 = VERTEX_POINT ( 'NONE', #50069 ) ;
#41507 = LINE ( 'NONE', #81417, #27852 ) ;
#41508 = VERTEX_POINT ( 'NONE', #49416 ) ;
#41509 = FACE_OUTER_BOUND ( 'NONE', #29163, .T. ) ;
#41511 = AXIS2_PLACEMENT_3D ( 'NONE', #102092, #113851, #12408 ) ;
#41510 = DIRECTION ( 'NONE',  ( -0.000000000000000000, 1.000000000000000000, -0.000000000000000000 ) ) ;
#41512 = VECTOR ( 'NONE', #76088, 1000.000000000000000 ) ;
#41513 = DIRECTION ( 'NONE',  ( 0.000000000000000000, 0.000000000000000000, 1.000000000000000000 ) ) ;
#41514 = DIRECTION ( 'NONE',  ( 0.000000000000000000, 1.000000000000000000, 0.000000000000000000 ) ) ;
#41515 = DIRECTION ( 'NONE',  ( -0.000000000000000000, 1.000000000000000000, -0.000000000000000000 ) ) ;
#41516 = DIRECTION ( 'NONE',  ( 0.000000000000000000, 0.000000000000000000, 1.000000000000000000 ) ) ;
#41517 = DIRECTION ( 'NONE',  ( -0.000000000000000000, 1.000000000000000000, -0.000000000000000000 ) ) ;
#41518 = VERTEX_POINT ( 'NONE', #89328 ) ;
#41519 = CONICAL_SURFACE ( 'NONE', #70741, 0.1000000000000002554, 0.003490658503988666988 ) ;
#41521 = EDGE_CURVE ( 'NONE', #17072, #121453, #39609, .T. ) ;
#41520 = DIRECTION ( 'NONE',  ( 0.000000000000000000, -0.9999939076577903929, 0.003490651415223739937 ) ) ;
#41522 = FACE_OUTER_BOUND ( 'NONE', #6760, .T. ) ;
#41523 = CARTESIAN_POINT ( 'NONE',  ( 1.049999999999954081, 2.500000000000000000, -6.048780366869526581 ) ) ;
#41524 = COLOUR_RGB ( '', 0.09019608, 0.27058824, 0.51372549) ;
#41525 = ADVANCED_FACE ( 'NONE', ( #19948 ), #59891, .T. ) ;
#41526 = EDGE_LOOP ( 'NONE', ( #64552, #92627 ) ) ;
#41527 = AXIS2_PLACEMENT_3D ( 'NONE', #109705, #20034, #61900 ) ;
#41528 = CARTESIAN_POINT ( 'NONE',  ( -3.750000000000025757, 12.50000000000000000, 1.472243186433545459 ) ) ;
#41529 = VECTOR ( 'NONE', #125050, 1000.000000000000000 ) ;
#41530 = ORIENTED_EDGE ( 'NONE', *, *, #60670, .T. ) ;
#41531 = ORIENTED_EDGE ( 'NONE', *, *, #128347, .F. ) ;
#41532 = CARTESIAN_POINT ( 'NONE',  ( -7.700000000000010836, 2.500000000000000000, 3.983716857408420964 ) ) ;
#41533 = EDGE_LOOP ( 'NONE', ( #2603, #120466, #4076, #89880 ) ) ;
#41535 = AXIS2_PLACEMENT_3D ( 'NONE', #42718, #123192, #2102 ) ;
#41534 = CARTESIAN_POINT ( 'NONE',  ( 8.099999999999923261, 12.50000000000000000, -4.741630453620016006 ) ) ;
#41536 = CARTESIAN_POINT ( 'NONE',  ( 3.149999999999942624, 12.50000000000000000, 6.148780366869520897 ) ) ;
#41537 = VERTEX_POINT ( 'NONE', #73535 ) ;
#41538 = DIRECTION ( 'NONE',  ( -0.000000000000000000, 1.000000000000000000, -0.000000000000000000 ) ) ;
#41539 = DIRECTION ( 'NONE',  ( 0.000000000000000000, 1.000000000000000000, 0.000000000000000000 ) ) ;
#41540 = CONICAL_SURFACE ( 'NONE', #70762, 0.1000000000000002554, 0.003490658503988666988 ) ;
#41541 = EDGE_LOOP ( 'NONE', ( #122341, #39 ) ) ;
#41542 = AXIS2_PLACEMENT_3D ( 'NONE', #112500, #22846, #102662 ) ;
#41543 = ORIENTED_EDGE ( 'NONE', *, *, #109089, .T. ) ;
#41544 = ORIENTED_EDGE ( 'NONE', *, *, #103804, .T. ) ;
#41545 = PLANE ( 'NONE',  #75553 ) ;
#41546 = DIRECTION ( 'NONE',  ( 0.000000000000000000, 0.000000000000000000, 1.000000000000000000 ) ) ;
#41547 = CARTESIAN_POINT ( 'NONE',  ( 8.149999999999923972, 2.500000000000000000, -6.841600689897077814 ) ) ;
#41548 = FACE_BOUND ( 'NONE', #48550, .T. ) ;
#41549 = ORIENTED_EDGE ( 'NONE', *, *, #81773, .F. ) ;
#41550 = DIRECTION ( 'NONE',  ( 0.000000000000000000, 0.000000000000000000, -1.000000000000000000 ) ) ;
#41551 = FACE_OUTER_BOUND ( 'NONE', #37449, .T. ) ;
#41552 = EDGE_LOOP ( 'NONE', ( #95032, #35077 ) ) ;
#41554 = EDGE_CURVE ( 'NONE', #42734, #14735, #65458, .T. ) ;
#41553 = DIRECTION ( 'NONE',  ( 0.000000000000000000, 1.000000000000000000, 0.000000000000000000 ) ) ;
#41555 = CARTESIAN_POINT ( 'NONE',  ( -4.600000000000025402, 12.50000000000000000, 4.330127018922196314 ) ) ;
#41556 = CARTESIAN_POINT ( 'NONE',  ( -10.45000000000000462, 12.50000000000000000, -2.165063509461097713 ) ) ;
#41557 = CARTESIAN_POINT ( 'NONE',  ( 4.149999999999939959, 12.50000000000000000, -2.165063509461101710 ) ) ;
#41558 = CIRCLE ( 'NONE', #66566, 0.09999999999999982514 ) ;
#41559 = DIRECTION ( 'NONE',  ( 0.000000000000000000, 0.000000000000000000, 1.000000000000000000 ) ) ;
#41560 = DIRECTION ( 'NONE',  ( 0.000000000000000000, 0.000000000000000000, 1.000000000000000000 ) ) ;
#41561 = CARTESIAN_POINT ( 'NONE',  ( 1.049999999999952083, 2.500000000000000000, 6.941600689897073018 ) ) ;
#41562 = EDGE_CURVE ( 'NONE', #42779, #31532, #15366, .T. ) ;
#41563 = AXIS2_PLACEMENT_3D ( 'NONE', #34744, #104726, #106038 ) ;
#41564 = CIRCLE ( 'NONE', #114694, 0.09999999999999982514 ) ;
#41565 = EDGE_LOOP ( 'NONE', ( #101866, #29712 ) ) ;
#41566 = ORIENTED_EDGE ( 'NONE', *, *, #57148, .F. ) ;
#41567 = CONICAL_SURFACE ( 'NONE', #58282, 0.1000000000000002554, 0.003490658503988666988 ) ;
#41568 = ORIENTED_EDGE ( 'NONE', *, *, #11190, .F. ) ;
#41569 = ORIENTED_EDGE ( 'NONE', *, *, #116970, .T. ) ;
#41570 = DIRECTION ( 'NONE',  ( 0.000000000000000000, -0.000000000000000000, 1.000000000000000000 ) ) ;
#41571 = ADVANCED_FACE ( 'NONE', ( #22541 ), #31700, .T. ) ;
#41572 = LINE ( 'NONE', #81480, #92769 ) ;
#41573 = EDGE_LOOP ( 'NONE', ( #114302, #12106 ) ) ;
#41574 = FACE_BOUND ( 'NONE', #24451, .T. ) ;
#41575 = EDGE_CURVE ( 'NONE', #126915, #65424, #98920, .T. ) ;
#41576 = PLANE ( 'NONE',  #58460 ) ;
#41577 = DIRECTION ( 'NONE',  ( -0.000000000000000000, -1.000000000000000000, -0.000000000000000000 ) ) ;
#41578 = AXIS2_PLACEMENT_3D ( 'NONE', #45941, #17069, #126428 ) ;
#41579 = VECTOR ( 'NONE', #45647, 1000.000000000000000 ) ;
#41580 = CARTESIAN_POINT ( 'NONE',  ( -13.34999999999999076, 12.50000000000000000, -1.407149913249510442 ) ) ;
#41581 = CIRCLE ( 'NONE', #18572, 0.1000000000000000056 ) ;
#41582 = EDGE_CURVE ( 'NONE', #97417, #73329, #78085, .T. ) ;
#41583 = DIRECTION ( 'NONE',  ( 0.000000000000000000, 0.000000000000000000, -1.000000000000000000 ) ) ;
#41584 = FACE_OUTER_BOUND ( 'NONE', #93337, .T. ) ;
#41585 = CARTESIAN_POINT ( 'NONE',  ( -1.250000000000001554, 12.50000000000000000, 6.430097255199259010 ) ) ;
#41586 = DIRECTION ( 'NONE',  ( -0.000000000000000000, 1.000000000000000000, -0.000000000000000000 ) ) ;
#41587 = FACE_OUTER_BOUND ( 'NONE', #16317, .T. ) ;
#41588 = EDGE_CURVE ( 'NONE', #102089, #5504, #112837, .T. ) ;
#41589 = DIRECTION ( 'NONE',  ( -4.274815082592931898E-19, -0.9999939076577903929, -0.003490651415223739937 ) ) ;
#41590 = VERTEX_POINT ( 'NONE', #63084 ) ;
#41591 = AXIS2_PLACEMENT_3D ( 'NONE', #126022, #24623, #23980 ) ;
#41592 = VERTEX_POINT ( 'NONE', #51358 ) ;
#41593 = CONICAL_SURFACE ( 'NONE', #10178, 0.1000000000000000472, 0.003490658503988666988 ) ;
#41594 = VERTEX_POINT ( 'NONE', #82080 ) ;
#41595 = VERTEX_POINT ( 'NONE', #91258 ) ;
#41596 = ORIENTED_EDGE ( 'NONE', *, *, #88687, .T. ) ;
#41597 = ORIENTED_EDGE ( 'NONE', *, *, #14376, .F. ) ;
#41598 = CARTESIAN_POINT ( 'NONE',  ( -0.2000000000000399791, 2.500000000000000000, -4.576537180435977348 ) ) ;
#41599 = VERTEX_POINT ( 'NONE', #61814 ) ;
#41600 = DIRECTION ( 'NONE',  ( -0.000000000000000000, -1.000000000000000000, -0.000000000000000000 ) ) ;
#41601 = CARTESIAN_POINT ( 'NONE',  ( 1.849999999999950573, 12.50000000000000000, -1.818653347947326138 ) ) ;
#41602 = FACE_OUTER_BOUND ( 'NONE', #99840, .T. ) ;
#41603 = DIRECTION ( 'NONE',  ( 0.000000000000000000, 0.000000000000000000, -1.000000000000000000 ) ) ;
#41604 = CIRCLE ( 'NONE', #22725, 0.09999999999999999167 ) ;
#41605 = ORIENTED_EDGE ( 'NONE', *, *, #91198, .T. ) ;
#41606 = CARTESIAN_POINT ( 'NONE',  ( 3.749999999999976907, 2.500000000000000000, 2.165063509461097713 ) ) ;
#41607 = ORIENTED_EDGE ( 'NONE', *, *, #3846, .T. ) ;
#41608 = EDGE_CURVE ( 'NONE', #43343, #24753, #55105, .T. ) ;
#41609 = EDGE_LOOP ( 'NONE', ( #37173, #4746 ) ) ;
#41610 = VECTOR ( 'NONE', #109724, 1000.000000000000000 ) ;
#41611 = DIRECTION ( 'NONE',  ( 0.000000000000000000, 0.000000000000000000, 1.000000000000000000 ) ) ;
#41612 = DIRECTION ( 'NONE',  ( 0.000000000000000000, 1.000000000000000000, 0.000000000000000000 ) ) ;
#41613 = DIRECTION ( 'NONE',  ( 0.000000000000000000, 0.000000000000000000, -1.000000000000000000 ) ) ;
#41614 = EDGE_CURVE ( 'NONE', #74146, #13780, #75927, .T. ) ;
#41615 = VERTEX_POINT ( 'NONE', #12678 ) ;
#41616 = CONICAL_SURFACE ( 'NONE', #37402, 0.09999999999999982514, 0.003490658503988666988 ) ;
#41618 = EDGE_CURVE ( 'NONE', #110642, #46368, #36236, .T. ) ;
#41617 = ORIENTED_EDGE ( 'NONE', *, *, #124628, .F. ) ;
#41619 = DIRECTION ( 'NONE',  ( 0.000000000000000000, 0.000000000000000000, 1.000000000000000000 ) ) ;
#41620 = VECTOR ( 'NONE', #128947, 1000.000000000000000 ) ;
#41621 = DIRECTION ( 'NONE',  ( 0.000000000000000000, -0.000000000000000000, 1.000000000000000000 ) ) ;
#41622 = LINE ( 'NONE', #120163, #95785 ) ;
#41623 = DIRECTION ( 'NONE',  ( 0.000000000000000000, -0.9999939076577903929, 0.003490651415223739937 ) ) ;
#41624 = EDGE_LOOP ( 'NONE', ( #32368, #91331, #127727, #9638 ) ) ;
#41625 = ADVANCED_FACE ( 'NONE', ( #103001 ), #32139, .T. ) ;
#41626 = ADVANCED_FACE ( 'NONE', ( #13326 ), #86388, .T. ) ;
#41627 = DIRECTION ( 'NONE',  ( -0.000000000000000000, -1.000000000000000000, -0.000000000000000000 ) ) ;
#41628 = AXIS2_PLACEMENT_3D ( 'NONE', #61881, #50129, #100492 ) ;
#41629 = ADVANCED_FACE ( 'NONE', ( #91904 ), #96850, .T. ) ;
#41630 = EDGE_CURVE ( 'NONE', #8036, #52810, #6948, .T. ) ;
#41631 = ORIENTED_EDGE ( 'NONE', *, *, #41875, .T. ) ;
#41632 = CARTESIAN_POINT ( 'NONE',  ( 14.69113575804714422, -2.499999999999999556, 6.337000356225073183 ) ) ;
#41633 = ORIENTED_EDGE ( 'NONE', *, *, #63862, .T. ) ;
#41634 = DIRECTION ( 'NONE',  ( 0.000000000000000000, 0.000000000000000000, 1.000000000000000000 ) ) ;
#41637 = EDGE_CURVE ( 'NONE', #54383, #91134, #9222, .T. ) ;
#41636 = CONICAL_SURFACE ( 'NONE', #75059, 0.1000000000000000056, 0.003490658503988666988 ) ;
#41635 = CIRCLE ( 'NONE', #22849, 0.09999999999999999167 ) ;
#41638 = DIRECTION ( 'NONE',  ( -0.000000000000000000, 1.000000000000000000, -0.000000000000000000 ) ) ;
#41639 = CARTESIAN_POINT ( 'NONE',  ( -2.500000000000032419, 12.50000000000000000, 0.6277270498435120194 ) ) ;
#41640 = CONICAL_SURFACE ( 'NONE', #129471, 0.1000000000000000056, 0.003490658503988666988 ) ;
#41641 = LINE ( 'NONE', #103106, #94711 ) ;
#41642 = FACE_OUTER_BOUND ( 'NONE', #122117, .T. ) ;
#41643 = ORIENTED_EDGE ( 'NONE', *, *, #45021, .T. ) ;
#41644 = ADVANCED_FACE ( 'NONE', ( #3523 ), #2869, .T. ) ;
#41645 = DIRECTION ( 'NONE',  ( 0.000000000000000000, 0.000000000000000000, -1.000000000000000000 ) ) ;
#41648 = EDGE_CURVE ( 'NONE', #91650, #110814, #33633, .T. ) ;
#41647 = AXIS2_PLACEMENT_3D ( 'NONE', #88825, #89475, #30577 ) ;
#41646 = CONICAL_SURFACE ( 'NONE', #106454, 0.1000000000000002554, 0.003490658503988666988 ) ;
#41649 = CARTESIAN_POINT ( 'NONE',  ( 2.299999999999949640, 12.50000000000000000, -4.611443907251939756 ) ) ;
#41650 = ORIENTED_EDGE ( 'NONE', *, *, #10836, .T. ) ;
#41651 = ORIENTED_EDGE ( 'NONE', *, *, #44869, .F. ) ;
#41652 = ORIENTED_EDGE ( 'NONE', *, *, #81640, .F. ) ;
#41653 = CARTESIAN_POINT ( 'NONE',  ( 17.50000000000000000, -2.750000000000000000, 10.00000000000000178 ) ) ;
#41654 = CARTESIAN_POINT ( 'NONE',  ( 14.14999999999989377, 12.50000000000000000, -1.472243186433550122 ) ) ;
#41655 = DIRECTION ( 'NONE',  ( -4.274815082592931898E-19, -0.9999939076577903929, -0.003490651415223739937 ) ) ;
#41656 = LINE ( 'NONE', #2322, #92520 ) ;
#41657 = DIRECTION ( 'NONE',  ( 0.000000000000000000, 0.000000000000000000, -1.000000000000000000 ) ) ;
#41658 = CARTESIAN_POINT ( 'NONE',  ( 7.499999999999927169, 12.50000000000000000, 3.572213422710607489 ) ) ;
#41659 = CARTESIAN_POINT ( 'NONE',  ( -3.100000000000028511, 12.50000000000000000, 0.4115034346978110880 ) ) ;
#41660 = VECTOR ( 'NONE', #22885, 1000.000000000000000 ) ;
#41661 = AXIS2_PLACEMENT_3D ( 'NONE', #125514, #65951, #56750 ) ;
#41662 = CONICAL_SURFACE ( 'NONE', #6111, 0.09999999999999999167, 0.003490658503988666988 ) ;
#41663 = VERTEX_POINT ( 'NONE', #63739 ) ;
#41664 = CARTESIAN_POINT ( 'NONE',  ( 5.799999999999933209, 2.500000000000000000, -0.1000000000000023925 ) ) ;
#41665 = CARTESIAN_POINT ( 'NONE',  ( 2.049999999999948308, 12.50000000000000000, 6.495190528383297135 ) ) ;
#41666 = CARTESIAN_POINT ( 'NONE',  ( -7.700000000000014388, 2.500000000000000000, -4.576537180435977348 ) ) ;
#41667 = CARTESIAN_POINT ( 'NONE',  ( 0.8499999999999536815, 12.50000000000000000, 5.802370205355744659 ) ) ;
#41668 = CIRCLE ( 'NONE', #106385, 0.1000000000000002554 ) ;
#41669 = VERTEX_POINT ( 'NONE', #104920 ) ;
#41670 = AXIS2_PLACEMENT_3D ( 'NONE', #28574, #58682, #126778 ) ;
#41671 = CARTESIAN_POINT ( 'NONE',  ( 5.849999999999931255, 2.500000000000000000, 2.857883832488649301 ) ) ;
#41672 = CONICAL_SURFACE ( 'NONE', #100234, 0.09999999999999982514, 0.003490658503988666988 ) ;
#41673 = EDGE_CURVE ( 'NONE', #52514, #22700, #94902, .T. ) ;
#41674 = DIRECTION ( 'NONE',  ( 0.000000000000000000, -0.000000000000000000, 1.000000000000000000 ) ) ;
#41676 = EDGE_LOOP ( 'NONE', ( #5514, #55283, #57668, #63483 ) ) ;
#41675 = CARTESIAN_POINT ( 'NONE',  ( 0.3999999999999568345, 2.500000000000000000, -3.737306695894649700 ) ) ;
#41677 = VECTOR ( 'NONE', #34299, 1000.000000000000000 ) ;
#41678 = ORIENTED_EDGE ( 'NONE', *, *, #28941, .T. ) ;
#41679 = CARTESIAN_POINT ( 'NONE',  ( 9.799999999999915445, 2.500000000000000000, -4.576537180435977348 ) ) ;
#41680 = EDGE_CURVE ( 'NONE', #21282, #105322, #117872, .T. ) ;
#41681 = CONICAL_SURFACE ( 'NONE', #8195, 0.1000000000000000472, 0.003490658503988666988 ) ;
#41682 = ORIENTED_EDGE ( 'NONE', *, *, #95815, .T. ) ;
#41683 = ORIENTED_EDGE ( 'NONE', *, *, #33932, .T. ) ;
#41684 = DIRECTION ( 'NONE',  ( -0.000000000000000000, -1.000000000000000000, -0.000000000000000000 ) ) ;
#41685 = DIRECTION ( 'NONE',  ( -0.000000000000000000, -1.000000000000000000, -0.000000000000000000 ) ) ;
#41686 = DIRECTION ( 'NONE',  ( 0.000000000000000000, 0.000000000000000000, -1.000000000000000000 ) ) ;
#41687 = CARTESIAN_POINT ( 'NONE',  ( -14.34999999999998543, 2.500000000000000000, 2.611473670974877148 ) ) ;
#41688 = EDGE_LOOP ( 'NONE', ( #60749, #115168, #14230, #16436 ) ) ;
#41689 = CARTESIAN_POINT ( 'NONE',  ( -8.950000000000004619, 2.500000000000000000, 6.148780366869520897 ) ) ;
#41690 = ORIENTED_EDGE ( 'NONE', *, *, #18403, .T. ) ;
#41691 = CARTESIAN_POINT ( 'NONE',  ( -9.150000000000009237, 12.50000000000000000, 2.099970236277060032 ) ) ;
#41692 = CARTESIAN_POINT ( 'NONE',  ( 186.3229166673494319, -4.445597072760092416, 7.700000000000049916 ) ) ;
#41693 = ORIENTED_EDGE ( 'NONE', *, *, #80341, .T. ) ;
#41694 = ORIENTED_EDGE ( 'NONE', *, *, #77731, .F. ) ;
#41695 = ORIENTED_EDGE ( 'NONE', *, *, #40635, .F. ) ;
#41696 = ORIENTED_EDGE ( 'NONE', *, *, #16355, .T. ) ;
#41697 = PLANE ( 'NONE',  #69199 ) ;
#41698 = CARTESIAN_POINT ( 'NONE',  ( 6.714630671504235870, 2.500000000000252687, 9.763603585389109440 ) ) ;
#41699 = CARTESIAN_POINT ( 'NONE',  ( 13.94999999999989626, 2.500000000000000000, 2.511473670974873507 ) ) ;
#41700 = FACE_BOUND ( 'NONE', #51622, .T. ) ;
#41701 = VERTEX_POINT ( 'NONE', #125858 ) ;
#41702 = CARTESIAN_POINT ( 'NONE',  ( 11.89999999999990798, 2.500000000000000000, 4.676537180435972552 ) ) ;
#41703 = CARTESIAN_POINT ( 'NONE',  ( 187.1093750003414016, 9.264065473108010111E-16, -7.564683531250000925 ) ) ;
#41704 = AXIS2_PLACEMENT_3D ( 'NONE', #107450, #96985, #104857 ) ;
#41705 = DIRECTION ( 'NONE',  ( -0.000000000000000000, -1.000000000000000000, -0.000000000000000000 ) ) ;
#41706 = DIRECTION ( 'NONE',  ( -4.274815082592931898E-19, -0.9999939076577903929, -0.003490651415223739937 ) ) ;
#41707 = PLANE ( 'NONE',  #86125 ) ;
#41708 = CARTESIAN_POINT ( 'NONE',  ( 13.74999999999989342, 2.500000000000000000, -1.472243186433550122 ) ) ;
#41709 = CIRCLE ( 'NONE', #47962, 0.06509327318403745899 ) ;
#41710 = CARTESIAN_POINT ( 'NONE',  ( 4.799999999999934097, 2.500000000000000000, 4.676537180435972552 ) ) ;
#41711 = ADVANCED_FACE ( 'NONE', ( #116687 ), #115374, .T. ) ;
#41712 = LINE ( 'NONE', #12220, #3453 ) ;
#41714 = CONICAL_SURFACE ( 'NONE', #114842, 0.1000000000000000056, 0.003490658503988666988 ) ;
#41713 = CIRCLE ( 'NONE', #24967, 0.06509327318403741736 ) ;
#41715 = VERTEX_POINT ( 'NONE', #25091 ) ;
#41716 = VERTEX_POINT ( 'NONE', #84000 ) ;
#41717 = ORIENTED_EDGE ( 'NONE', *, *, #105110, .T. ) ;
#41718 = ORIENTED_EDGE ( 'NONE', *, *, #17921, .T. ) ;
#41719 = EDGE_LOOP ( 'NONE', ( #43520, #36097, #29287, #65461 ) ) ;
#41720 = CARTESIAN_POINT ( 'NONE',  ( -6.250000000000017764, 12.50000000000000000, 7.188010851410848723 ) ) ;
#41722 = EDGE_CURVE ( 'NONE', #14537, #93110, #95132, .T. ) ;
#41721 = CIRCLE ( 'NONE', #68877, 0.1000000000000002554 ) ;
#41723 = ADVANCED_FACE ( 'NONE', ( #56471 ), #42602, .T. ) ;
#41724 = CARTESIAN_POINT ( 'NONE',  ( 10.39999999999991154, 2.500000000000000000, 5.122947341949749323 ) ) ;
#41725 = VERTEX_POINT ( 'NONE', #104301 ) ;
#41726 = FACE_BOUND ( 'NONE', #87126, .T. ) ;
#41727 = ADVANCED_FACE ( 'NONE', ( #74845 ), #99011, .T. ) ;
#41728 = CARTESIAN_POINT ( 'NONE',  ( -13.34999999999999076, 12.50000000000000000, -1.472243186433547901 ) ) ;
#41730 = VECTOR ( 'NONE', #30902, 1000.000000000000000 ) ;
#41729 = AXIS2_PLACEMENT_3D ( 'NONE', #77669, #8284, #106498 ) ;
#41731 = ADVANCED_FACE ( 'NONE', ( #85927 ), #109476, .T. ) ;
#41732 = ORIENTED_EDGE ( 'NONE', *, *, #10129, .T. ) ;
#41733 = DIRECTION ( 'NONE',  ( -0.000000000000000000, -1.000000000000000000, -0.000000000000000000 ) ) ;
#41734 = CARTESIAN_POINT ( 'NONE',  ( -2.499999999999996447, 2.500000000000000000, 4.330127018922196314 ) ) ;
#41735 = PLANE ( 'NONE',  #9290 ) ;
#41736 = ADVANCED_FACE ( 'NONE', ( #17169 ), #78190, .T. ) ;
#41737 = CARTESIAN_POINT ( 'NONE',  ( -6.850000000000013856, 2.500000000000000000, 6.841600689897072485 ) ) ;
#41738 = ORIENTED_EDGE ( 'NONE', *, *, #84332, .T. ) ;
#41739 = CARTESIAN_POINT ( 'NONE',  ( -3.749999999999994671, 12.50000000000000000, -6.495190528383302464 ) ) ;
#41740 = ORIENTED_EDGE ( 'NONE', *, *, #120648, .T. ) ;
#41741 = ORIENTED_EDGE ( 'NONE', *, *, #53824, .T. ) ;
#41742 = ORIENTED_EDGE ( 'NONE', *, *, #90947, .F. ) ;
#41743 = CONICAL_SURFACE ( 'NONE', #70965, 0.09999999999999999167, 0.003490658503988666988 ) ;
#41744 = DIRECTION ( 'NONE',  ( 0.000000000000000000, 0.000000000000000000, 1.000000000000000000 ) ) ;
#41745 = DIRECTION ( 'NONE',  ( 0.000000000000000000, 1.000000000000000000, 0.000000000000000000 ) ) ;
#41746 = EDGE_LOOP ( 'NONE', ( #106018, #20745 ) ) ;
#41747 = DIRECTION ( 'NONE',  ( -0.000000000000000000, 1.000000000000000000, -0.000000000000000000 ) ) ;
#41748 = AXIS2_PLACEMENT_3D ( 'NONE', #42142, #34272, #2858 ) ;
#41749 = DIRECTION ( 'NONE',  ( 0.000000000000000000, 0.000000000000000000, 1.000000000000000000 ) ) ;
#41750 = DIRECTION ( 'NONE',  ( -0.000000000000000000, 1.000000000000000000, -0.000000000000000000 ) ) ;
#41751 = DIRECTION ( 'NONE',  ( -0.000000000000000000, 1.000000000000000000, -0.000000000000000000 ) ) ;
#41752 = CARTESIAN_POINT ( 'NONE',  ( 185.9895833340161460, -4.445597072760115509, -7.700000000000001954 ) ) ;
#41753 = ORIENTED_EDGE ( 'NONE', *, *, #99502, .F. ) ;
#41754 = CARTESIAN_POINT ( 'NONE',  ( 2.899999999999946620, 2.500000000000000000, 0.5928203230275495006 ) ) ;
#41756 = EDGE_LOOP ( 'NONE', ( #89868, #13320, #117603, #40161 ) ) ;
#41755 = AXIS2_PLACEMENT_3D ( 'NONE', #15867, #55805, #26999 ) ;
#41757 = DIRECTION ( 'NONE',  ( -0.000000000000000000, -1.000000000000000000, -0.000000000000000000 ) ) ;
#41758 = AXIS2_PLACEMENT_3D ( 'NONE', #58354, #9240, #28237 ) ;
#41759 = AXIS2_PLACEMENT_3D ( 'NONE', #36623, #66695, #85692 ) ;
#41760 = VERTEX_POINT ( 'NONE', #27032 ) ;
#41761 = DIRECTION ( 'NONE',  ( 0.000000000000000000, -0.9999939076577903929, 0.003490651415223739937 ) ) ;
#41762 = ORIENTED_EDGE ( 'NONE', *, *, #46585, .T. ) ;
#41763 = DIRECTION ( 'NONE',  ( -0.000000000000000000, 1.000000000000000000, -0.000000000000000000 ) ) ;
#41764 = DIRECTION ( 'NONE',  ( -1.000000000000000000, -0.000000000000000000, -0.000000000000000000 ) ) ;
#41765 = CARTESIAN_POINT ( 'NONE',  ( 0.6499999999999566125, 2.500000000000000000, -6.048780366869526581 ) ) ;
#41766 = DIRECTION ( 'NONE',  ( -0.000000000000000000, -1.000000000000000000, -0.000000000000000000 ) ) ;
#41767 = CARTESIAN_POINT ( 'NONE',  ( 97.50000000000000000, 0.000000000000000000, 7.500000000000000000 ) ) ;
#41768 = AXIS2_PLACEMENT_3D ( 'NONE', #83861, #15095, #53765 ) ;
#41769 = ORIENTED_EDGE ( 'NONE', *, *, #37633, .F. ) ;
#41770 = ORIENTED_EDGE ( 'NONE', *, *, #125528, .T. ) ;
#41772 = ORIENTED_EDGE ( 'NONE', *, *, #76925, .F. ) ;
#41771 = CONICAL_SURFACE ( 'NONE', #45871, 0.1000000000000000472, 0.003490658503988666988 ) ;
#41773 = CARTESIAN_POINT ( 'NONE',  ( -8.550000000000011369, 12.50000000000000000, -2.511473670974877948 ) ) ;
#41774 = AXIS2_PLACEMENT_3D ( 'NONE', #95125, #16532, #114746 ) ;
#41775 = DIRECTION ( 'NONE',  ( -0.000000000000000000, -1.000000000000000000, -0.000000000000000000 ) ) ;
#41777 = EDGE_CURVE ( 'NONE', #121648, #34168, #115727, .T. ) ;
#41776 = CARTESIAN_POINT ( 'NONE',  ( -13.54999999999999005, 2.500000000000000000, -1.818653347947323917 ) ) ;
#41779 = VERTEX_POINT ( 'NONE', #36218 ) ;
#41778 = ORIENTED_EDGE ( 'NONE', *, *, #94823, .T. ) ;
#41780 = EDGE_LOOP ( 'NONE', ( #45071, #112328, #53891, #53759 ) ) ;
#41781 = EDGE_CURVE ( 'NONE', #115124, #65093, #103216, .T. ) ;
#41782 = DIRECTION ( 'NONE',  ( 0.000000000000000000, 1.000000000000000000, 0.000000000000000000 ) ) ;
#41783 = EDGE_CURVE ( 'NONE', #35444, #90867, #111629, .T. ) ;
#41784 = ORIENTED_EDGE ( 'NONE', *, *, #7789, .T. ) ;
#41785 = CARTESIAN_POINT ( 'NONE',  ( -0.4500000000000397571, 12.50000000000000000, -6.495190528383302464 ) ) ;
#41786 = CARTESIAN_POINT ( 'NONE',  ( -0.2000000000000408673, 12.50000000000000000, -3.983716857408426293 ) ) ;
#41787 = CARTESIAN_POINT ( 'NONE',  ( 1.849999999999951017, 2.500000000000000000, -6.048780366869526581 ) ) ;
#41788 = DIRECTION ( 'NONE',  ( -4.274815082592931898E-19, -0.9999939076577903929, -0.003490651415223739937 ) ) ;
#41790 = EDGE_CURVE ( 'NONE', #77714, #113705, #17522, .T. ) ;
#41789 = DIRECTION ( 'NONE',  ( -4.274815082592931898E-19, -0.9999939076577903929, -0.003490651415223739937 ) ) ;
#41791 = CARTESIAN_POINT ( 'NONE',  ( 14.59999999999989484, 2.500000000000000000, -0.1000000000000022815 ) ) ;
#41792 = DIRECTION ( 'NONE',  ( 0.000000000000000000, 0.000000000000000000, 1.000000000000000000 ) ) ;
#41793 = DIRECTION ( 'NONE',  ( 0.000000000000000000, 1.000000000000000000, 0.000000000000000000 ) ) ;
#41794 = ORIENTED_EDGE ( 'NONE', *, *, #99872, .T. ) ;
#41795 = EDGE_CURVE ( 'NONE', #3331, #12469, #6704, .T. ) ;
#41796 = DIRECTION ( 'NONE',  ( -0.000000000000000000, 1.000000000000000000, -0.000000000000000000 ) ) ;
#41797 = EDGE_CURVE ( 'NONE', #106728, #27665, #90697, .T. ) ;
#41798 = CARTESIAN_POINT ( 'NONE',  ( 35.03103265464613969, -3.271231620382011762, 3.345711933271832361 ) ) ;
#41799 = ORIENTED_EDGE ( 'NONE', *, *, #71010, .F. ) ;
#41800 =( BOUNDED_CURVE ( )  B_SPLINE_CURVE ( 2, ( #34908, #104270, #103632 ),
 .UNSPECIFIED., .F., .F. ) 
 B_SPLINE_CURVE_WITH_KNOTS ( ( 3, 3 ),
 ( 0.000000000000000000, 8.005299705393619772E-05 ),
 .UNSPECIFIED. ) 
 CURVE ( )  GEOMETRIC_REPRESENTATION_ITEM ( )  RATIONAL_B_SPLINE_CURVE ( ( 1.000000000000000000, 0.9972072019273716670, 0.9944676636816938142 ) ) 
 REPRESENTATION_ITEM ( '' )  );
#41801 = ORIENTED_EDGE ( 'NONE', *, *, #17164, .T. ) ;
#41802 = CARTESIAN_POINT ( 'NONE',  ( 184.5260416670080588, -6.551208109652273848, -3.782341765625003571 ) ) ;
#41803 = DIRECTION ( 'NONE',  ( 0.000000000000000000, 0.000000000000000000, -1.000000000000000000 ) ) ;
#41804 = CARTESIAN_POINT ( 'NONE',  ( -10.85000000000000142, 12.50000000000000000, -5.867463478539783672 ) ) ;
#41805 = EDGE_CURVE ( 'NONE', #91613, #36380, #127038, .T. ) ;
#41806 = DIRECTION ( 'NONE',  ( 0.000000000000000000, 1.000000000000000000, 0.000000000000000000 ) ) ;
#41807 = CARTESIAN_POINT ( 'NONE',  ( 0.7999999999999612976, 2.500000000000000000, -1.084202172485504434E-16 ) ) ;
#41808 = DIRECTION ( 'NONE',  ( 0.000000000000000000, 1.000000000000000000, 0.000000000000000000 ) ) ;
#41809 = DIRECTION ( 'NONE',  ( -0.000000000000000000, -1.000000000000000000, -0.000000000000000000 ) ) ;
#41810 = DIRECTION ( 'NONE',  ( 0.000000000000000000, 1.000000000000000000, 0.000000000000000000 ) ) ;
#41811 = AXIS2_PLACEMENT_3D ( 'NONE', #107266, #4524, #26776 ) ;
#41812 = DIRECTION ( 'NONE',  ( 0.000000000000000000, 1.000000000000000000, 0.000000000000000000 ) ) ;
#41813 = ORIENTED_EDGE ( 'NONE', *, *, #77801, .T. ) ;
#41814 = ORIENTED_EDGE ( 'NONE', *, *, #35834, .T. ) ;
#41815 = AXIS2_PLACEMENT_3D ( 'NONE', #112959, #105723, #23945 ) ;
#41816 = ORIENTED_EDGE ( 'NONE', *, *, #48690, .F. ) ;
#41817 = EDGE_LOOP ( 'NONE', ( #90099, #51532 ) ) ;
#41818 = LINE ( 'NONE', #81709, #63026 ) ;
#41819 = DIRECTION ( 'NONE',  ( 0.000000000000000000, 1.000000000000000000, 0.000000000000000000 ) ) ;
#41822 = VERTEX_POINT ( 'NONE', #35569 ) ;
#41821 = AXIS2_PLACEMENT_3D ( 'NONE', #86412, #17676, #78562 ) ;
#41820 = VECTOR ( 'NONE', #110843, 1000.000000000000000 ) ;
#41823 = DIRECTION ( 'NONE',  ( 0.000000000000000000, 1.000000000000000000, 0.000000000000000000 ) ) ;
#41824 = LINE ( 'NONE', #90236, #11197 ) ;
#41825 = DIRECTION ( 'NONE',  ( 0.000000000000000000, 1.000000000000000000, 0.000000000000000000 ) ) ;
#41827 = VERTEX_POINT ( 'NONE', #49264 ) ;
#41826 = DIRECTION ( 'NONE',  ( 0.000000000000000000, 0.000000000000000000, 1.000000000000000000 ) ) ;
#41828 = DIRECTION ( 'NONE',  ( -4.274815082592931898E-19, -0.9999939076577903929, -0.003490651415223739937 ) ) ;
#41829 = CARTESIAN_POINT ( 'NONE',  ( -7.500000000000015099, 12.50000000000000000, -5.022947341949754119 ) ) ;
#41830 = VERTEX_POINT ( 'NONE', #89807 ) ;
#41831 = ADVANCED_FACE ( 'NONE', ( #98330 ), #60379, .T. ) ;
#41832 = ORIENTED_EDGE ( 'NONE', *, *, #44549, .F. ) ;
#41833 = ORIENTED_EDGE ( 'NONE', *, *, #72633, .T. ) ;
#41834 = EDGE_LOOP ( 'NONE', ( #36303, #128132, #48189, #18026 ) ) ;
#41835 = DIRECTION ( 'NONE',  ( 0.000000000000000000, 0.000000000000000000, -1.000000000000000000 ) ) ;
#41836 = DIRECTION ( 'NONE',  ( 0.000000000000000000, 1.000000000000000000, 0.000000000000000000 ) ) ;
#41837 = DIRECTION ( 'NONE',  ( 0.000000000000000000, 1.000000000000000000, 0.000000000000000000 ) ) ;
#41838 = CONICAL_SURFACE ( 'NONE', #35568, 0.09999999999999999167, 0.003490658503988666988 ) ;
#41839 = EDGE_LOOP ( 'NONE', ( #61134, #5996, #107416, #118987 ) ) ;
#41840 = CONICAL_SURFACE ( 'NONE', #112922, 0.1000000000000002554, 0.003490658503988666988 ) ;
#41841 = CARTESIAN_POINT ( 'NONE',  ( 13.34999999999990017, 12.50000000000000000, 2.922977105672686982 ) ) ;
#41842 = ORIENTED_EDGE ( 'NONE', *, *, #103478, .F. ) ;
#41843 = DIRECTION ( 'NONE',  ( -0.000000000000000000, -1.000000000000000000, -0.000000000000000000 ) ) ;
#41844 = DIRECTION ( 'NONE',  ( 0.000000000000000000, 0.000000000000000000, 1.000000000000000000 ) ) ;
#41845 = CARTESIAN_POINT ( 'NONE',  ( 1.249999999999988454, 2.500000000000000000, 2.165063509461097713 ) ) ;
#41846 = CARTESIAN_POINT ( 'NONE',  ( -1.850000000000033840, 12.50000000000000000, 1.818653347947321475 ) ) ;
#41847 = VECTOR ( 'NONE', #45698, 1000.000000000000000 ) ;
#41848 = ORIENTED_EDGE ( 'NONE', *, *, #41003, .F. ) ;
#41849 = ORIENTED_EDGE ( 'NONE', *, *, #101906, .T. ) ;
#41850 = ORIENTED_EDGE ( 'NONE', *, *, #74734, .F. ) ;
#41851 = CARTESIAN_POINT ( 'NONE',  ( -1.900000000000034994, 2.500000000000000000, -0.2464101615137783419 ) ) ;
#41852 = LINE ( 'NONE', #102677, #25115 ) ;
#41853 = FACE_BOUND ( 'NONE', #73738, .T. ) ;
#41854 = AXIS2_PLACEMENT_3D ( 'NONE', #2396, #82281, #10920 ) ;
#41855 = CARTESIAN_POINT ( 'NONE',  ( 154.1524742528378056, 2.500000000000000000, 1.703575533167231537 ) ) ;
#41856 = DIRECTION ( 'NONE',  ( -0.000000000000000000, -1.000000000000000000, -0.000000000000000000 ) ) ;
#41857 = DIRECTION ( 'NONE',  ( -0.000000000000000000, 1.000000000000000000, -0.000000000000000000 ) ) ;
#41858 = VECTOR ( 'NONE', #89781, 1000.000000000000000 ) ;
#41859 = AXIS2_PLACEMENT_3D ( 'NONE', #76615, #17001, #16372 ) ;
#41860 = DIRECTION ( 'NONE',  ( -0.000000000000000000, 1.000000000000000000, -0.000000000000000000 ) ) ;
#41861 = DIRECTION ( 'NONE',  ( 0.000000000000000000, 0.000000000000000000, -1.000000000000000000 ) ) ;
#41862 = CARTESIAN_POINT ( 'NONE',  ( -10.85000000000000142, 12.50000000000000000, -2.165063509461097713 ) ) ;
#41863 = ORIENTED_EDGE ( 'NONE', *, *, #108968, .F. ) ;
#41864 = CIRCLE ( 'NONE', #125467, 0.1000000000000000472 ) ;
#41865 = DIRECTION ( 'NONE',  ( 0.000000000000000000, 0.000000000000000000, -1.000000000000000000 ) ) ;
#41866 = EDGE_CURVE ( 'NONE', #119726, #10174, #124138, .T. ) ;
#41867 = DIRECTION ( 'NONE',  ( -0.000000000000000000, 1.000000000000000000, -0.000000000000000000 ) ) ;
#41868 = AXIS2_PLACEMENT_3D ( 'NONE', #105445, #95621, #125699 ) ;
#41869 = VERTEX_POINT ( 'NONE', #38817 ) ;
#41870 = ORIENTED_EDGE ( 'NONE', *, *, #95301, .F. ) ;
#41871 = FACE_OUTER_BOUND ( 'NONE', #57297, .T. ) ;
#41872 = EDGE_CURVE ( 'NONE', #81006, #30789, #67701, .T. ) ;
#41873 = LINE ( 'NONE', #92233, #65370 ) ;
#41874 = FACE_BOUND ( 'NONE', #42761, .T. ) ;
#41875 = EDGE_CURVE ( 'NONE', #35997, #120269, #34281, .T. ) ;
#41876 = CARTESIAN_POINT ( 'NONE',  ( 4.199999999999941558, 12.50000000000000000, -4.265033745738164406 ) ) ;
#41877 = EDGE_CURVE ( 'NONE', #42325, #62716, #92761, .T. ) ;
#41878 = EDGE_CURVE ( 'NONE', #106136, #112609, #79989, .T. ) ;
#41879 = ORIENTED_EDGE ( 'NONE', *, *, #78096, .F. ) ;
#41880 = DIRECTION ( 'NONE',  ( -4.274815082592931898E-19, -0.9999939076577903929, -0.003490651415223739937 ) ) ;
#41881 = EDGE_CURVE ( 'NONE', #17735, #117196, #30076, .T. ) ;
#41882 = ADVANCED_FACE ( 'NONE', ( #37506 ), #71931, .T. ) ;
#41883 = CARTESIAN_POINT ( 'NONE',  ( 184.7083333333333144, -4.445597072760115509, -7.700000000000001954 ) ) ;
#41884 = EDGE_CURVE ( 'NONE', #123363, #20166, #47319, .T. ) ;
#41885 = ORIENTED_EDGE ( 'NONE', *, *, #47624, .T. ) ;
#41886 = DIRECTION ( 'NONE',  ( 0.000000000000000000, -0.000000000000000000, 1.000000000000000000 ) ) ;
#41887 = FACE_OUTER_BOUND ( 'NONE', #4616, .T. ) ;
#41888 = CIRCLE ( 'NONE', #10552, 0.06509327318403741736 ) ;
#41889 = ORIENTED_EDGE ( 'NONE', *, *, #7306, .F. ) ;
#41890 = CARTESIAN_POINT ( 'NONE',  ( 1.649999999999951505, 12.50000000000000000, 2.792790559304612064 ) ) ;
#41891 = AXIS2_PLACEMENT_3D ( 'NONE', #124830, #35174, #75708 ) ;
#41893 = EDGE_CURVE ( 'NONE', #12959, #65883, #32227, .T. ) ;
#41892 = DIRECTION ( 'NONE',  ( 0.000000000000000000, 0.000000000000000000, -1.000000000000000000 ) ) ;
#41894 = ORIENTED_EDGE ( 'NONE', *, *, #77977, .F. ) ;
#41895 = DIRECTION ( 'NONE',  ( 0.000000000000000000, 0.000000000000000000, 1.000000000000000000 ) ) ;
#41897 = AXIS2_PLACEMENT_3D ( 'NONE', #9496, #100449, #19295 ) ;
#41896 = AXIS2_PLACEMENT_3D ( 'NONE', #99773, #49398, #129257 ) ;
#41898 = DIRECTION ( 'NONE',  ( 0.000000000000000000, 0.000000000000000000, 1.000000000000000000 ) ) ;
#41899 = CYLINDRICAL_SURFACE ( 'NONE', #101589, 10.00000000000000000 ) ;
#41900 = ORIENTED_EDGE ( 'NONE', *, *, #29087, .F. ) ;
#41901 = VERTEX_POINT ( 'NONE', #17845 ) ;
#41902 = CARTESIAN_POINT ( 'NONE',  ( -11.64999999999999680, 2.500000000000000000, 7.288010851410849256 ) ) ;
#41903 = VERTEX_POINT ( 'NONE', #9317 ) ;
#41904 = CARTESIAN_POINT ( 'NONE',  ( -4.600000000000024514, 2.500000000000000000, 3.637306695894644726 ) ) ;
#41905 = CARTESIAN_POINT ( 'NONE',  ( 10.64999999999990976, 2.500000000000000000, 1.818653347947321475 ) ) ;
#41906 = CARTESIAN_POINT ( 'NONE',  ( 6.849999999999929479, 2.500000000000000000, -2.511473670974877948 ) ) ;
#41907 = ORIENTED_EDGE ( 'NONE', *, *, #26180, .T. ) ;
#41908 = DIRECTION ( 'NONE',  ( 0.000000000000000000, 0.000000000000000000, 1.000000000000000000 ) ) ;
#41909 = CARTESIAN_POINT ( 'NONE',  ( -6.050000000000018474, 2.500000000000000000, 2.511473670974873507 ) ) ;
#41910 = CARTESIAN_POINT ( 'NONE',  ( 187.5000000000000000, 9.429780353434619030E-16, -7.700000000000000178 ) ) ;
#41911 = CARTESIAN_POINT ( 'NONE',  ( 3.349999999999944578, 2.500000000000000000, -5.902370205355750521 ) ) ;
#41912 = DIRECTION ( 'NONE',  ( 0.000000000000000000, -0.000000000000000000, 1.000000000000000000 ) ) ;
#41913 = FACE_OUTER_BOUND ( 'NONE', #96057, .T. ) ;
#41914 = EDGE_LOOP ( 'NONE', ( #78806, #47984 ) ) ;
#41915 = ORIENTED_EDGE ( 'NONE', *, *, #73107, .T. ) ;
#41916 = CARTESIAN_POINT ( 'NONE',  ( 15.39999999999989200, 2.500000000000000000, -0.7928203230275543412 ) ) ;
#41917 = ORIENTED_EDGE ( 'NONE', *, *, #12546, .T. ) ;
#41918 = CARTESIAN_POINT ( 'NONE',  ( 105.7538778652931626, 6.265388825864785183, -4.478799985686444884 ) ) ;
#41920 = ORIENTED_EDGE ( 'NONE', *, *, #110180, .F. ) ;
#41919 = ORIENTED_EDGE ( 'NONE', *, *, #53114, .T. ) ;
#41921 = VERTEX_POINT ( 'NONE', #69516 ) ;
#41922 = EDGE_CURVE ( 'NONE', #5094, #47068, #68875, .T. ) ;
#41923 = DIRECTION ( 'NONE',  ( 0.000000000000000000, 0.000000000000000000, 1.000000000000000000 ) ) ;
#41924 = EDGE_CURVE ( 'NONE', #47526, #78573, #7051, .T. ) ;
#41925 = DIRECTION ( 'NONE',  ( -0.000000000000000000, 1.000000000000000000, -0.000000000000000000 ) ) ;
#41926 = AXIS2_PLACEMENT_3D ( 'NONE', #121598, #31956, #39856 ) ;
#41927 = DIRECTION ( 'NONE',  ( 0.000000000000000000, 0.000000000000000000, -1.000000000000000000 ) ) ;
#41928 = EDGE_CURVE ( 'NONE', #123848, #101406, #96948, .T. ) ;
#41929 = SURFACE_SIDE_STYLE ('',( #120477 ) ) ;
#41930 = DIRECTION ( 'NONE',  ( 0.000000000000000000, 1.000000000000000000, 0.000000000000000000 ) ) ;
#41931 = DIRECTION ( 'NONE',  ( 0.000000000000000000, -0.000000000000000000, 1.000000000000000000 ) ) ;
#41932 = LINE ( 'NONE', #51745, #111321 ) ;
#41933 = DIRECTION ( 'NONE',  ( -0.000000000000000000, -1.000000000000000000, -0.000000000000000000 ) ) ;
#41934 = CARTESIAN_POINT ( 'NONE',  ( 10.44999999999991047, 2.500000000000000000, 2.165063509461097713 ) ) ;
#41935 = EDGE_CURVE ( 'NONE', #112874, #115594, #38137, .T. ) ;
#41936 = CARTESIAN_POINT ( 'NONE',  ( 5.449999999999936229, 12.50000000000000000, 6.430097255199259010 ) ) ;
#41937 = ADVANCED_FACE ( 'NONE', ( #68232 ), #108155, .T. ) ;
#41939 = VERTEX_POINT ( 'NONE', #48606 ) ;
#41938 = EDGE_CURVE ( 'NONE', #10213, #117937, #23804, .T. ) ;
#41940 = EDGE_CURVE ( 'NONE', #23223, #72558, #802, .T. ) ;
#41941 = DIRECTION ( 'NONE',  ( -0.000000000000000000, -1.000000000000000000, -0.000000000000000000 ) ) ;
#41942 = EDGE_LOOP ( 'NONE', ( #64877, #123521, #52859, #53405 ) ) ;
#41943 = EDGE_LOOP ( 'NONE', ( #84388, #14715, #5326, #83135 ) ) ;
#41944 = FACE_OUTER_BOUND ( 'NONE', #87620, .T. ) ;
#41945 = DIRECTION ( 'NONE',  ( 0.000000000000000000, -0.9999939076577903929, 0.003490651415223739937 ) ) ;
#41946 = LINE ( 'NONE', #20996, #36079 ) ;
#41947 = EDGE_CURVE ( 'NONE', #27524, #128176, #11369, .T. ) ;
#41948 = AXIS2_PLACEMENT_3D ( 'NONE', #2037, #33459, #53724 ) ;
#41949 = DIRECTION ( 'NONE',  ( 0.000000000000000000, 0.000000000000000000, -1.000000000000000000 ) ) ;
#41950 = CIRCLE ( 'NONE', #106675, 0.09999999999999982514 ) ;
#41951 = CARTESIAN_POINT ( 'NONE',  ( -9.400000000000007461, 2.500000000000000000, -0.3464101615137783474 ) ) ;
#41952 = DIRECTION ( 'NONE',  ( 0.000000000000000000, 0.000000000000000000, 1.000000000000000000 ) ) ;
#41953 = LINE ( 'NONE', #120502, #59281 ) ;
#41954 = ORIENTED_EDGE ( 'NONE', *, *, #65848, .T. ) ;
#41955 = ORIENTED_EDGE ( 'NONE', *, *, #86029, .T. ) ;
#41956 = EDGE_LOOP ( 'NONE', ( #16442, #85205 ) ) ;
#41957 = ORIENTED_EDGE ( 'NONE', *, *, #51336, .F. ) ;
#41958 = EDGE_CURVE ( 'NONE', #39483, #108866, #113780, .T. ) ;
#41959 = VERTEX_POINT ( 'NONE', #72754 ) ;
#41960 = DIRECTION ( 'NONE',  ( -1.000000000000000000, -0.000000000000000000, -0.000000000000000000 ) ) ;
#41961 = CARTESIAN_POINT ( 'NONE',  ( -11.64999999999999680, 2.500000000000000000, 1.472243186433545459 ) ) ;
#41962 = DIRECTION ( 'NONE',  ( 0.000000000000000000, 1.000000000000000000, 0.000000000000000000 ) ) ;
#41963 = CARTESIAN_POINT ( 'NONE',  ( -3.950000000000024603, 2.500000000000000000, -2.511473670974877948 ) ) ;
#41964 = FACE_OUTER_BOUND ( 'NONE', #80078, .T. ) ;
#41965 = ORIENTED_EDGE ( 'NONE', *, *, #96694, .F. ) ;
#41966 = DIRECTION ( 'NONE',  ( 0.000000000000000000, 1.000000000000000000, 0.000000000000000000 ) ) ;
#41967 = DIRECTION ( 'NONE',  ( 0.000000000000000000, 0.000000000000000000, 1.000000000000000000 ) ) ;
#41968 = LINE ( 'NONE', #63539, #54127 ) ;
#41969 = DIRECTION ( 'NONE',  ( -4.274815082592931898E-19, -0.9999939076577903929, -0.003490651415223739937 ) ) ;
#41970 = CARTESIAN_POINT ( 'NONE',  ( -8.750000000000010658, 2.500000000000000000, 2.757883832488649656 ) ) ;
#41971 = EDGE_LOOP ( 'NONE', ( #81433, #65441 ) ) ;
#41972 = EDGE_CURVE ( 'NONE', #37042, #72947, #76119, .T. ) ;
#41973 = ORIENTED_EDGE ( 'NONE', *, *, #68995, .T. ) ;
#41974 = ORIENTED_EDGE ( 'NONE', *, *, #27261, .F. ) ;
#41975 = VECTOR ( 'NONE', #59671, 1000.000000000000000 ) ;
#41976 = DIRECTION ( 'NONE',  ( 0.000000000000000000, 1.000000000000000000, 0.000000000000000000 ) ) ;
#41977 = AXIS2_PLACEMENT_3D ( 'NONE', #53362, #2299, #362 ) ;
#41978 = VERTEX_POINT ( 'NONE', #50522 ) ;
#41979 = CARTESIAN_POINT ( 'NONE',  ( 11.64999999999990266, 2.500000000000000000, -6.495190528383302464 ) ) ;
#41980 = CARTESIAN_POINT ( 'NONE',  ( -7.900000000000014566, 12.50000000000000000, -3.637306695894650055 ) ) ;
#41981 = AXIS2_PLACEMENT_3D ( 'NONE', #117948, #27626, #67551 ) ;
#41983 = ORIENTED_EDGE ( 'NONE', *, *, #23518, .T. ) ;
#41982 = CIRCLE ( 'NONE', #2249, 0.06509327318403745899 ) ;
#41984 = CARTESIAN_POINT ( 'NONE',  ( 184.1666666666666856, -6.668395609140176816, -3.850000000000003642 ) ) ;
#41985 = LINE ( 'NONE', #51811, #120565 ) ;
#41986 = ADVANCED_FACE ( 'NONE', ( #10584 ), #99207, .T. ) ;
#41987 = DIRECTION ( 'NONE',  ( 0.000000000000000000, 0.000000000000000000, 1.000000000000000000 ) ) ;
#41988 = DIRECTION ( 'NONE',  ( 0.000000000000000000, -0.000000000000000000, 1.000000000000000000 ) ) ;
#41989 = CARTESIAN_POINT ( 'NONE',  ( -0.6000000000000388356, 12.50000000000000000, 3.983716857408420964 ) ) ;
#41990 = ORIENTED_EDGE ( 'NONE', *, *, #36103, .T. ) ;
#41991 = EDGE_LOOP ( 'NONE', ( #89938, #1568, #121852, #26616 ) ) ;
#41992 = DIRECTION ( 'NONE',  ( -0.000000000000000000, -1.000000000000000000, -0.000000000000000000 ) ) ;
#41993 = LINE ( 'NONE', #51822, #64413 ) ;
#41994 = CARTESIAN_POINT ( 'NONE',  ( 0.8499999999999557909, 2.500000000000000000, -6.495190528383302464 ) ) ;
#41995 = LINE ( 'NONE', #21051, #77302 ) ;
#41996 = VERTEX_POINT ( 'NONE', #81916 ) ;
#41997 = ORIENTED_EDGE ( 'NONE', *, *, #73950, .F. ) ;
#41998 = DIRECTION ( 'NONE',  ( -0.000000000000000000, -1.000000000000000000, -0.000000000000000000 ) ) ;
#41999 = CARTESIAN_POINT ( 'NONE',  ( 10.84999999999991260, 12.50000000000000000, 6.560283801567334372 ) ) ;
#42000 = DIRECTION ( 'NONE',  ( 0.000000000000000000, 0.000000000000000000, 1.000000000000000000 ) ) ;
#42001 = DIRECTION ( 'NONE',  ( 0.000000000000000000, -0.9999939076577903929, 0.003490651415223739937 ) ) ;
#42002 = ORIENTED_EDGE ( 'NONE', *, *, #56440, .T. ) ;
#42003 = AXIS2_PLACEMENT_3D ( 'NONE', #62097, #89609, #61455 ) ;
#42004 = DIRECTION ( 'NONE',  ( -0.000000000000000000, -1.000000000000000000, -0.000000000000000000 ) ) ;
#42005 = EDGE_CURVE ( 'NONE', #82577, #93997, #81288, .T. ) ;
#42006 = LINE ( 'NONE', #50523, #7648 ) ;
#42007 = VERTEX_POINT ( 'NONE', #82586 ) ;
#42008 = CARTESIAN_POINT ( 'NONE',  ( 3.949999999999941558, 12.50000000000000000, -1.883746621131363597 ) ) ;
#42009 = ORIENTED_EDGE ( 'NONE', *, *, #28739, .F. ) ;
#42010 = CONICAL_SURFACE ( 'NONE', #33698, 0.09999999999999982514, 0.003490658503988666988 ) ;
#42011 = DIRECTION ( 'NONE',  ( 0.000000000000000000, 1.000000000000000000, 0.000000000000000000 ) ) ;
#42012 = AXIS2_PLACEMENT_3D ( 'NONE', #24229, #122438, #33422 ) ;
#42013 = VERTEX_POINT ( 'NONE', #90434 ) ;
#42014 = DIRECTION ( 'NONE',  ( 0.000000000000000000, 0.000000000000000000, 1.000000000000000000 ) ) ;
#42015 = CARTESIAN_POINT ( 'NONE',  ( -12.29999999999999538, 12.50000000000000000, -4.741630453620013341 ) ) ;
#42016 = EDGE_CURVE ( 'NONE', #62754, #62269, #103314, .T. ) ;
#42017 = ORIENTED_EDGE ( 'NONE', *, *, #10867, .T. ) ;
#42018 = EDGE_CURVE ( 'NONE', #16041, #110257, #51193, .T. ) ;
#42019 = VERTEX_POINT ( 'NONE', #22382 ) ;
#42020 = EDGE_CURVE ( 'NONE', #59954, #63275, #57338, .T. ) ;
#42021 = ADVANCED_FACE ( 'NONE', ( #43310 ), #60991, .T. ) ;
#42022 = FACE_OUTER_BOUND ( 'NONE', #80407, .T. ) ;
#42023 = CARTESIAN_POINT ( 'NONE',  ( -6.250000000000021316, 12.50000000000000000, -1.472243186433550122 ) ) ;
#42025 = CARTESIAN_POINT ( 'NONE',  ( -12.94999999999999218, 2.500000000000000000, 2.265063509461101354 ) ) ;
#42024 = VECTOR ( 'NONE', #11050, 1000.000000000000000 ) ;
#42026 = CARTESIAN_POINT ( 'NONE',  ( 184.3593750003413732, 0.000000000000000000, 7.564683531250000925 ) ) ;
#42027 = CIRCLE ( 'NONE', #35768, 0.06509327318403745899 ) ;
#42028 = EDGE_CURVE ( 'NONE', #129259, #46131, #49046, .T. ) ;
#42029 = DIRECTION ( 'NONE',  ( -0.000000000000000000, -1.000000000000000000, -0.000000000000000000 ) ) ;
#42030 = DIRECTION ( 'NONE',  ( -4.274815082592931898E-19, -0.9999939076577903929, -0.003490651415223739937 ) ) ;
#42031 = DIRECTION ( 'NONE',  ( 0.000000000000000000, 0.000000000000000000, 1.000000000000000000 ) ) ;
#42032 = DIRECTION ( 'NONE',  ( 0.000000000000000000, 1.000000000000000000, 0.000000000000000000 ) ) ;
#42033 = DIRECTION ( 'NONE',  ( 0.000000000000000000, 0.000000000000000000, -1.000000000000000000 ) ) ;
#42034 = EDGE_CURVE ( 'NONE', #112256, #64883, #115825, .T. ) ;
#42035 = CIRCLE ( 'NONE', #19030, 0.09999999999999982514 ) ;
#42036 = EDGE_CURVE ( 'NONE', #61413, #50205, #124243, .T. ) ;
#42037 = EDGE_CURVE ( 'NONE', #88884, #42322, #113316, .T. ) ;
#42038 = ORIENTED_EDGE ( 'NONE', *, *, #19965, .T. ) ;
#42039 = ORIENTED_EDGE ( 'NONE', *, *, #47858, .F. ) ;
#42040 = DIRECTION ( 'NONE',  ( 0.000000000000000000, 1.000000000000000000, 0.000000000000000000 ) ) ;
#42041 = ORIENTED_EDGE ( 'NONE', *, *, #38369, .T. ) ;
#42042 = AXIS2_PLACEMENT_3D ( 'NONE', #118163, #120109, #50098 ) ;
#42043 = FACE_OUTER_BOUND ( 'NONE', #17564, .T. ) ;
#42044 = CARTESIAN_POINT ( 'NONE',  ( 9.599999999999914380, 2.500000000000000000, -4.430127018922202176 ) ) ;
#42045 = CARTESIAN_POINT ( 'NONE',  ( 15.59999999999988951, 2.500000000000000000, 0.3464101615137735735 ) ) ;
#42047 = VERTEX_POINT ( 'NONE', #92380 ) ;
#42046 = ORIENTED_EDGE ( 'NONE', *, *, #102074, .T. ) ;
#42048 = PRODUCT_RELATED_PRODUCT_CATEGORY ( 'part', '', ( #57498 ) ) ;
#42049 = FACE_BOUND ( 'NONE', #23711, .T. ) ;
#42050 = ORIENTED_EDGE ( 'NONE', *, *, #36315, .F. ) ;
#42051 = CARTESIAN_POINT ( 'NONE',  ( -5.400000000000019895, 2.500000000000000000, -2.276824562219559311E-15 ) ) ;
#42052 = DIRECTION ( 'NONE',  ( -0.000000000000000000, 1.000000000000000000, -0.000000000000000000 ) ) ;
#42053 = LINE ( 'NONE', #91147, #51327 ) ;
#42054 = LINE ( 'NONE', #113358, #32687 ) ;
#42055 = CARTESIAN_POINT ( 'NONE',  ( 4.549999999999939426, 2.500000000000000000, -6.595190528383302109 ) ) ;
#42056 = FACE_OUTER_BOUND ( 'NONE', #70848, .T. ) ;
#42057 = DIRECTION ( 'NONE',  ( 0.000000000000000000, 1.000000000000000000, 0.000000000000000000 ) ) ;
#42058 = DIRECTION ( 'NONE',  ( 0.000000000000000000, 0.000000000000000000, -1.000000000000000000 ) ) ;
#42059 = CARTESIAN_POINT ( 'NONE',  ( -12.69999999999999218, 2.500000000000000000, 4.776537180435972196 ) ) ;
#42060 = DIRECTION ( 'NONE',  ( -0.000000000000000000, 1.000000000000000000, -0.000000000000000000 ) ) ;
#42061 = CARTESIAN_POINT ( 'NONE',  ( -10.45000000000000107, 2.500000000000000000, 2.065063509461097624 ) ) ;
#42062 = ORIENTED_EDGE ( 'NONE', *, *, #71744, .F. ) ;
#42063 = ORIENTED_EDGE ( 'NONE', *, *, #100635, .F. ) ;
#42064 = ORIENTED_EDGE ( 'NONE', *, *, #45093, .F. ) ;
#42065 = DIRECTION ( 'NONE',  ( 0.000000000000000000, 0.000000000000000000, -1.000000000000000000 ) ) ;
#42066 = ORIENTED_EDGE ( 'NONE', *, *, #20766, .F. ) ;
#42067 = DIRECTION ( 'NONE',  ( -0.000000000000000000, -1.000000000000000000, -0.000000000000000000 ) ) ;
#42068 = CONICAL_SURFACE ( 'NONE', #16969, 0.1000000000000002554, 0.003490658503988666988 ) ;
#42069 = LINE ( 'NONE', #121914, #128028 ) ;
#42070 = VECTOR ( 'NONE', #126470, 1000.000000000000000 ) ;
#42072 = ADVANCED_FACE ( 'NONE', ( #21725 ), #84523, .T. ) ;
#42071 = CIRCLE ( 'NONE', #2329, 0.09999999999999999167 ) ;
#42074 = VERTEX_POINT ( 'NONE', #121843 ) ;
#42073 = ORIENTED_EDGE ( 'NONE', *, *, #64807, .F. ) ;
#42075 = ORIENTED_EDGE ( 'NONE', *, *, #11686, .T. ) ;
#42076 = DIRECTION ( 'NONE',  ( -0.000000000000000000, 1.000000000000000000, -0.000000000000000000 ) ) ;
#42077 = AXIS2_PLACEMENT_3D ( 'NONE', #36685, #25536, #55010 ) ;
#42078 = DIRECTION ( 'NONE',  ( 0.000000000000000000, 0.000000000000000000, -1.000000000000000000 ) ) ;
#42079 = AXIS2_PLACEMENT_3D ( 'NONE', #83604, #74423, #93416 ) ;
#42080 = CARTESIAN_POINT ( 'NONE',  ( -4.150000000000024336, 2.500000000000000000, 1.472243186433545459 ) ) ;
#42081 = CARTESIAN_POINT ( 'NONE',  ( -11.89999999999999680, 2.500000000000000000, -0.3464101615137741841 ) ) ;
#42082 = CARTESIAN_POINT ( 'NONE',  ( -4.600000000000028066, 2.500000000000000000, -3.537306695894649966 ) ) ;
#42083 = CONICAL_SURFACE ( 'NONE', #6516, 0.1000000000000002554, 0.003490658503988666988 ) ;
#42084 = DIRECTION ( 'NONE',  ( 0.000000000000000000, 1.000000000000000000, 0.000000000000000000 ) ) ;
#42085 = ORIENTED_EDGE ( 'NONE', *, *, #115060, .T. ) ;
#42086 = CARTESIAN_POINT ( 'NONE',  ( -8.550000000000011369, 12.50000000000000000, -2.511473670974877948 ) ) ;
#42087 = ORIENTED_EDGE ( 'NONE', *, *, #35843, .T. ) ;
#42088 = EDGE_CURVE ( 'NONE', #39107, #86369, #21855, .T. ) ;
#42089 = ORIENTED_EDGE ( 'NONE', *, *, #8309, .F. ) ;
#42090 = ORIENTED_EDGE ( 'NONE', *, *, #45298, .T. ) ;
#42091 = ADVANCED_FACE ( 'NONE', ( #62929 ), #59423, .T. ) ;
#42092 = CARTESIAN_POINT ( 'NONE',  ( 8.349999999999923261, 2.500000000000000000, 1.472243186433545459 ) ) ;
#42093 = ORIENTED_EDGE ( 'NONE', *, *, #5947, .T. ) ;
#42094 = ORIENTED_EDGE ( 'NONE', *, *, #113262, .F. ) ;
#42095 = ORIENTED_EDGE ( 'NONE', *, *, #101557, .F. ) ;
#42096 = ADVANCED_FACE ( 'NONE', ( #83226 ), #33489, .T. ) ;
#42097 = FACE_OUTER_BOUND ( 'NONE', #56079, .T. ) ;
#42098 = DIRECTION ( 'NONE',  ( 0.000000000000000000, -0.000000000000000000, 1.000000000000000000 ) ) ;
#42099 = PLANE ( 'NONE',  #27553 ) ;
#42100 = CARTESIAN_POINT ( 'NONE',  ( 9.399999999999915090, 12.50000000000000000, 4.048810130592458201 ) ) ;
#42101 = CARTESIAN_POINT ( 'NONE',  ( 1.049999999999952083, 2.500000000000000000, 6.941600689897073018 ) ) ;
#42102 = DIRECTION ( 'NONE',  ( -0.000000000000000000, 1.000000000000000000, -0.000000000000000000 ) ) ;
#42103 = AXIS2_PLACEMENT_3D ( 'NONE', #90894, #71918, #49703 ) ;
#42104 = VECTOR ( 'NONE', #42775, 1000.000000000000000 ) ;
#42105 = EDGE_LOOP ( 'NONE', ( #118833, #87313 ) ) ;
#42106 = CARTESIAN_POINT ( 'NONE',  ( -3.150000000000032330, 2.500000000000000000, -6.148780366869526226 ) ) ;
#42107 = ORIENTED_EDGE ( 'NONE', *, *, #94180, .T. ) ;
#42108 = LINE ( 'NONE', #889, #77549 ) ;
#42109 = VERTEX_POINT ( 'NONE', #65498 ) ;
#42110 = FACE_OUTER_BOUND ( 'NONE', #101418, .T. ) ;
#42111 = VERTEX_POINT ( 'NONE', #125696 ) ;
#42112 = AXIS2_PLACEMENT_3D ( 'NONE', #49733, #59569, #89642 ) ;
#42113 = CARTESIAN_POINT ( 'NONE',  ( 6.449999999999930012, 2.500000000000000000, 6.841600689897072485 ) ) ;
#42114 = CIRCLE ( 'NONE', #115224, 5.000000000000000000 ) ;
#42115 = CARTESIAN_POINT ( 'NONE',  ( -3.749999999999991118, 2.500000000000000000, -2.065063509461102065 ) ) ;
#42116 = EDGE_LOOP ( 'NONE', ( #38336, #78895, #70256, #99610 ) ) ;
#42117 = ORIENTED_EDGE ( 'NONE', *, *, #111522, .F. ) ;
#42118 = DIRECTION ( 'NONE',  ( 0.000000000000000000, 0.000000000000000000, 1.000000000000000000 ) ) ;
#42119 = CARTESIAN_POINT ( 'NONE',  ( -2.300000000000033573, 2.500000000000000000, 4.676537180435972552 ) ) ;
#42120 = DIRECTION ( 'NONE',  ( 0.000000000000000000, 0.000000000000000000, 1.000000000000000000 ) ) ;
#42121 = DIRECTION ( 'NONE',  ( 0.000000000000000000, 1.000000000000000000, 0.000000000000000000 ) ) ;
#42122 = AXIS2_PLACEMENT_3D ( 'NONE', #107691, #106391, #67081 ) ;
#42123 = CARTESIAN_POINT ( 'NONE',  ( 6.049999999999930544, 2.500000000000000000, 2.511473670974873507 ) ) ;
#42124 = VERTEX_POINT ( 'NONE', #75966 ) ;
#42125 = EDGE_CURVE ( 'NONE', #69422, #7039, #85139, .T. ) ;
#42126 = DIRECTION ( 'NONE',  ( 0.000000000000000000, 1.000000000000000000, 0.000000000000000000 ) ) ;
#42127 = CONICAL_SURFACE ( 'NONE', #21279, 0.09999999999999982514, 0.003490658503988666988 ) ;
#42128 = CONICAL_SURFACE ( 'NONE', #115241, 0.09999999999999982514, 0.003490658503988666988 ) ;
#42129 = ORIENTED_EDGE ( 'NONE', *, *, #57775, .T. ) ;
#42130 = CARTESIAN_POINT ( 'NONE',  ( -7.500000000000016875, 2.500000000000000000, -3.637306695894650055 ) ) ;
#42131 = DIRECTION ( 'NONE',  ( -0.000000000000000000, -1.000000000000000000, -0.000000000000000000 ) ) ;
#42132 = VECTOR ( 'NONE', #51859, 1000.000000000000000 ) ;
#42133 = CONICAL_SURFACE ( 'NONE', #115247, 0.1000000000000002554, 0.003490658503988666988 ) ;
#42134 = ADVANCED_FACE ( 'NONE', ( #115216 ), #113966, .T. ) ;
#42135 = DIRECTION ( 'NONE',  ( -0.000000000000000000, -1.000000000000000000, -0.000000000000000000 ) ) ;
#42136 = CARTESIAN_POINT ( 'NONE',  ( 2.699999999999947331, 12.50000000000000000, -0.3464101615137783474 ) ) ;
#42137 = CARTESIAN_POINT ( 'NONE',  ( 14.99999999999992895, 2.500000000000000000, -0.1000000000000022815 ) ) ;
#42138 = EDGE_CURVE ( 'NONE', #84736, #4055, #34126, .T. ) ;
#42139 = DIRECTION ( 'NONE',  ( 0.000000000000000000, 0.000000000000000000, 1.000000000000000000 ) ) ;
#42140 = DIRECTION ( 'NONE',  ( 0.000000000000000000, 0.000000000000000000, -1.000000000000000000 ) ) ;
#42141 = VERTEX_POINT ( 'NONE', #93680 ) ;
#42142 = CARTESIAN_POINT ( 'NONE',  ( 1.249999999999952038, 2.500000000000000000, -1.472243186433550122 ) ) ;
#42143 = DIRECTION ( 'NONE',  ( 0.000000000000000000, 0.000000000000000000, 1.000000000000000000 ) ) ;
#42144 = PLANE ( 'NONE',  #49658 ) ;
#42145 = ORIENTED_EDGE ( 'NONE', *, *, #92465, .T. ) ;
#42146 = EDGE_CURVE ( 'NONE', #64315, #50389, #32330, .T. ) ;
#42147 = ORIENTED_EDGE ( 'NONE', *, *, #55823, .T. ) ;
#42148 = FACE_OUTER_BOUND ( 'NONE', #15340, .T. ) ;
#42149 = ORIENTED_EDGE ( 'NONE', *, *, #25008, .T. ) ;
#42150 = EDGE_LOOP ( 'NONE', ( #58384, #8612, #107871, #582 ) ) ;
#42151 = DIRECTION ( 'NONE',  ( -0.000000000000000000, -1.000000000000000000, -0.000000000000000000 ) ) ;
#42152 = CIRCLE ( 'NONE', #29621, 0.1000000000000000472 ) ;
#42153 = CONICAL_SURFACE ( 'NONE', #106975, 0.1000000000000000056, 0.003490658503988666988 ) ;
#42154 = CONICAL_SURFACE ( 'NONE', #63078, 0.09999999999999982514, 0.003490658503988666988 ) ;
#42155 = EDGE_LOOP ( 'NONE', ( #62028, #14361, #44143, #32727 ) ) ;
#42156 = CARTESIAN_POINT ( 'NONE',  ( 1.049999999999952971, 12.50000000000000000, 6.213873640053559022 ) ) ;
#42157 = CARTESIAN_POINT ( 'NONE',  ( -8.150000000000012790, 2.500000000000000000, -2.611473670974877592 ) ) ;
#42158 = CARTESIAN_POINT ( 'NONE',  ( 18.27284318114731931, 0.4998542452748436227, 4.791717918552973465 ) ) ;
#42159 = ORIENTED_EDGE ( 'NONE', *, *, #63493, .F. ) ;
#42161 = DIRECTION ( 'NONE',  ( 0.000000000000000000, 0.000000000000000000, 1.000000000000000000 ) ) ;
#42160 = AXIS2_PLACEMENT_3D ( 'NONE', #39282, #119098, #81118 ) ;
#42162 = EDGE_CURVE ( 'NONE', #38593, #120493, #126367, .T. ) ;
#42163 = DIRECTION ( 'NONE',  ( 0.000000000000000000, 0.000000000000000000, 1.000000000000000000 ) ) ;
#42164 = AXIS2_PLACEMENT_3D ( 'NONE', #94680, #35772, #123493 ) ;
#42165 = VERTEX_POINT ( 'NONE', #55685 ) ;
#42166 = CIRCLE ( 'NONE', #115293, 0.06509327318403745899 ) ;
#42167 = EDGE_CURVE ( 'NONE', #47326, #114265, #95616, .T. ) ;
#42168 = ORIENTED_EDGE ( 'NONE', *, *, #40736, .T. ) ;
#42169 = ORIENTED_EDGE ( 'NONE', *, *, #109961, .F. ) ;
#42170 = DIRECTION ( 'NONE',  ( 0.000000000000000000, -0.9999939076577903929, 0.003490651415223739937 ) ) ;
#42171 = DIRECTION ( 'NONE',  ( 0.000000000000000000, -0.000000000000000000, 1.000000000000000000 ) ) ;
#42172 = DIRECTION ( 'NONE',  ( 0.000000000000000000, -0.000000000000000000, 1.000000000000000000 ) ) ;
#42173 = EDGE_CURVE ( 'NONE', #17483, #60337, #111718, .T. ) ;
#42174 = EDGE_CURVE ( 'NONE', #50142, #51049, #109578, .T. ) ;
#42175 = FACE_BOUND ( 'NONE', #76795, .T. ) ;
#42176 = ORIENTED_EDGE ( 'NONE', *, *, #75127, .T. ) ;
#42177 = EDGE_CURVE ( 'NONE', #85507, #4707, #55287, .T. ) ;
#42178 = EDGE_CURVE ( 'NONE', #39225, #70505, #126300, .T. ) ;
#42179 = CARTESIAN_POINT ( 'NONE',  ( -2.700000000000029932, 2.500000000000000000, -4.776537180435977525 ) ) ;
#42180 = CARTESIAN_POINT ( 'NONE',  ( 1.449999999999951328, 2.500000000000000000, -1.818653347947326138 ) ) ;
#42181 = ORIENTED_EDGE ( 'NONE', *, *, #73994, .F. ) ;
#42182 = LINE ( 'NONE', #64389, #122046 ) ;
#42183 = CARTESIAN_POINT ( 'NONE',  ( 1.899999999999951283, 2.500000000000000000, -0.3464101615137782364 ) ) ;
#42184 = EDGE_CURVE ( 'NONE', #2990, #102929, #117964, .T. ) ;
#42185 = DIRECTION ( 'NONE',  ( 0.000000000000000000, 0.000000000000000000, 1.000000000000000000 ) ) ;
#42186 = DIRECTION ( 'NONE',  ( 0.000000000000000000, 0.000000000000000000, 1.000000000000000000 ) ) ;
#42187 = DIRECTION ( 'NONE',  ( -0.000000000000000000, 1.000000000000000000, -0.000000000000000000 ) ) ;
#42188 = ADVANCED_FACE ( 'NONE', ( #4624 ), #13411, .T. ) ;
#42189 = DIRECTION ( 'NONE',  ( 0.000000000000000000, 1.000000000000000000, 0.000000000000000000 ) ) ;
#42190 = FACE_OUTER_BOUND ( 'NONE', #123540, .T. ) ;
#42191 = AXIS2_PLACEMENT_3D ( 'NONE', #37144, #28610, #56739 ) ;
#42193 = EDGE_CURVE ( 'NONE', #75709, #4289, #72021, .T. ) ;
#42192 = CIRCLE ( 'NONE', #115314, 0.09999999999999982514 ) ;
#42194 = EDGE_CURVE ( 'NONE', #58747, #63242, #35414, .T. ) ;
#42195 = ORIENTED_EDGE ( 'NONE', *, *, #46304, .T. ) ;
#42196 = ORIENTED_EDGE ( 'NONE', *, *, #104762, .F. ) ;
#42197 = EDGE_LOOP ( 'NONE', ( #96529, #45458 ) ) ;
#42198 = ORIENTED_EDGE ( 'NONE', *, *, #121474, .T. ) ;
#42199 = DIRECTION ( 'NONE',  ( -0.000000000000000000, 1.000000000000000000, -0.000000000000000000 ) ) ;
#42200 = FACE_OUTER_BOUND ( 'NONE', #110832, .T. ) ;
#42201 = CARTESIAN_POINT ( 'NONE',  ( -1.050000000000037792, 2.500000000000000000, 6.148780366869520009 ) ) ;
#42202 = VERTEX_POINT ( 'NONE', #55042 ) ;
#42203 = FACE_BOUND ( 'NONE', #5951, .T. ) ;
#42204 = EDGE_CURVE ( 'NONE', #74055, #6638, #86572, .T. ) ;
#42205 = CARTESIAN_POINT ( 'NONE',  ( -4.999999999999990230, 2.500000000000000000, -4.330127018922201643 ) ) ;
#42206 = DIRECTION ( 'NONE',  ( -0.000000000000000000, -1.000000000000000000, -0.000000000000000000 ) ) ;
#42207 = CIRCLE ( 'NONE', #107015, 0.1000000000000002554 ) ;
#42209 = CARTESIAN_POINT ( 'NONE',  ( -2.700000000000030820, 12.50000000000000000, -3.983716857408426293 ) ) ;
#42208 = AXIS2_PLACEMENT_3D ( 'NONE', #83335, #103615, #64320 ) ;
#42210 = VECTOR ( 'NONE', #58068, 1000.000000000000000 ) ;
#42211 = AXIS2_PLACEMENT_3D ( 'NONE', #45284, #15140, #45932 ) ;
#42212 = CARTESIAN_POINT ( 'NONE',  ( -1.850000000000033396, 2.500000000000000000, -1.918653347947325782 ) ) ;
#42213 = DIRECTION ( 'NONE',  ( 0.000000000000000000, 1.000000000000000000, 0.000000000000000000 ) ) ;
#42214 = CARTESIAN_POINT ( 'NONE',  ( 185.2916666666666572, 4.445597072760072876, -7.700000000000080114 ) ) ;
#42215 = CARTESIAN_POINT ( 'NONE',  ( -8.100000000000013856, 12.50000000000000000, -0.3464101615137782364 ) ) ;
#42216 = DIRECTION ( 'NONE',  ( 0.000000000000000000, 1.000000000000000000, 0.000000000000000000 ) ) ;
#42217 = PLANE ( 'NONE',  #14117 ) ;
#42218 = VECTOR ( 'NONE', #56613, 1000.000000000000000 ) ;
#42219 = EDGE_LOOP ( 'NONE', ( #89363, #76426 ) ) ;
#42220 = DIRECTION ( 'NONE',  ( -4.274815082592931898E-19, -0.9999939076577903929, -0.003490651415223739937 ) ) ;
#42221 = ORIENTED_EDGE ( 'NONE', *, *, #45900, .T. ) ;
#42222 = ORIENTED_EDGE ( 'NONE', *, *, #18809, .T. ) ;
#42223 = ORIENTED_EDGE ( 'NONE', *, *, #97147, .F. ) ;
#42225 = EDGE_LOOP ( 'NONE', ( #57535, #111335 ) ) ;
#42224 = AXIS2_PLACEMENT_3D ( 'NONE', #100303, #79378, #38156 ) ;
#42226 = AXIS2_PLACEMENT_3D ( 'NONE', #14535, #25655, #64927 ) ;
#42227 = AXIS2_PLACEMENT_3D ( 'NONE', #57997, #118835, #78290 ) ;
#42228 = EDGE_LOOP ( 'NONE', ( #127274, #26823, #98448, #63687 ) ) ;
#42229 = FACE_OUTER_BOUND ( 'NONE', #118154, .T. ) ;
#42230 = ORIENTED_EDGE ( 'NONE', *, *, #104756, .F. ) ;
#42231 = VERTEX_POINT ( 'NONE', #124433 ) ;
#42232 = AXIS2_PLACEMENT_3D ( 'NONE', #68398, #108325, #8823 ) ;
#42233 = DIRECTION ( 'NONE',  ( 0.000000000000000000, -0.9999939076577903929, 0.003490651415223739937 ) ) ;
#42234 = CIRCLE ( 'NONE', #123767, 0.1000000000000002554 ) ;
#42235 = CARTESIAN_POINT ( 'NONE',  ( 12.49999999999993960, 12.50000000000000000, -4.395220292106239768 ) ) ;
#42236 = CARTESIAN_POINT ( 'NONE',  ( 11.44999999999990870, 2.500000000000000000, 6.741600689897071952 ) ) ;
#42237 = CARTESIAN_POINT ( 'NONE',  ( 12.49999999999990052, 2.500000000000000000, 0.7928203230275495672 ) ) ;
#42238 = ORIENTED_EDGE ( 'NONE', *, *, #124578, .T. ) ;
#42239 = DIRECTION ( 'NONE',  ( -0.000000000000000000, 1.000000000000000000, -0.000000000000000000 ) ) ;
#42240 = ORIENTED_EDGE ( 'NONE', *, *, #65784, .F. ) ;
#42241 = EDGE_CURVE ( 'NONE', #88360, #109444, #34779, .T. ) ;
#42242 = ORIENTED_EDGE ( 'NONE', *, *, #18769, .T. ) ;
#42243 = DIRECTION ( 'NONE',  ( 0.000000000000000000, 1.000000000000000000, 0.000000000000000000 ) ) ;
#42244 = EDGE_CURVE ( 'NONE', #72184, #116662, #65737, .T. ) ;
#42245 = FACE_OUTER_BOUND ( 'NONE', #13200, .T. ) ;
#42246 = ORIENTED_EDGE ( 'NONE', *, *, #51244, .F. ) ;
#42247 = EDGE_LOOP ( 'NONE', ( #15995, #104085, #91691, #89047 ) ) ;
#42248 = FACE_OUTER_BOUND ( 'NONE', #65052, .T. ) ;
#42249 = CARTESIAN_POINT ( 'NONE',  ( -0.8500000000000390576, 2.500000000000000000, -2.165063509461101710 ) ) ;
#42250 = FACE_OUTER_BOUND ( 'NONE', #84658, .T. ) ;
#42252 = DIRECTION ( 'NONE',  ( 0.000000000000000000, -0.000000000000000000, 1.000000000000000000 ) ) ;
#42251 = CONICAL_SURFACE ( 'NONE', #40196, 0.1000000000000002554, 0.003490658503988666988 ) ;
#42253 = CIRCLE ( 'NONE', #12972, 0.09999999999999982514 ) ;
#42254 = AXIS2_PLACEMENT_3D ( 'NONE', #57721, #28251, #26328 ) ;
#42255 = CARTESIAN_POINT ( 'NONE',  ( -0.6000000000000383915, 12.50000000000000000, -4.676537180435977881 ) ) ;
#42256 = ORIENTED_EDGE ( 'NONE', *, *, #101862, .T. ) ;
#42257 = CARTESIAN_POINT ( 'NONE',  ( 2.099999999999949463, 2.500000000000000000, 0.7928203230275495672 ) ) ;
#42258 = CIRCLE ( 'NONE', #115373, 0.09999999999999982514 ) ;
#42260 = ORIENTED_EDGE ( 'NONE', *, *, #107649, .F. ) ;
#42259 = CIRCLE ( 'NONE', #127929, 0.1000000000000002554 ) ;
#42261 = CARTESIAN_POINT ( 'NONE',  ( 17.50000000000000000, 2.499999999999999556, -0.3333333333333299286 ) ) ;
#42262 = CONICAL_SURFACE ( 'NONE', #115376, 0.09999999999999999167, 0.003490658503988666988 ) ;
#42263 = DIRECTION ( 'NONE',  ( -0.000000000000000000, -1.000000000000000000, -0.000000000000000000 ) ) ;
#42264 = DIRECTION ( 'NONE',  ( -0.000000000000000000, 1.000000000000000000, -0.000000000000000000 ) ) ;
#42265 = CIRCLE ( 'NONE', #115378, 1.000000000000000888 ) ;
#42266 = AXIS2_PLACEMENT_3D ( 'NONE', #76112, #95111, #16521 ) ;
#42267 = CARTESIAN_POINT ( 'NONE',  ( 11.04999999999990656, 12.50000000000000000, -6.148780366869526226 ) ) ;
#42268 = CARTESIAN_POINT ( 'NONE',  ( -4.076600168545496672E-14, 2.500000000000000000, -5.022947341949754119 ) ) ;
#42269 = ORIENTED_EDGE ( 'NONE', *, *, #124658, .F. ) ;
#42270 = AXIS2_PLACEMENT_3D ( 'NONE', #125491, #105858, #37129 ) ;
#42271 = DIRECTION ( 'NONE',  ( -0.000000000000000000, -1.000000000000000000, -0.000000000000000000 ) ) ;
#42272 = CARTESIAN_POINT ( 'NONE',  ( 10.84999999999990905, 12.50000000000000000, -6.495190528383302464 ) ) ;
#42273 = ORIENTED_EDGE ( 'NONE', *, *, #44030, .F. ) ;
#42274 = VERTEX_POINT ( 'NONE', #75320 ) ;
#42275 = ORIENTED_EDGE ( 'NONE', *, *, #28022, .T. ) ;
#42276 = CARTESIAN_POINT ( 'NONE',  ( -15.39999999999997904, 2.500000000000000000, -0.5928203230275518321 ) ) ;
#42277 = PLANE ( 'NONE',  #53368 ) ;
#42278 = CARTESIAN_POINT ( 'NONE',  ( 14.14999999999989733, 12.50000000000000000, 1.472243186433545459 ) ) ;
#42279 = DIRECTION ( 'NONE',  ( -0.000000000000000000, 1.000000000000000000, -0.000000000000000000 ) ) ;
#42280 = EDGE_CURVE ( 'NONE', #53828, #36380, #16377, .T. ) ;
#42281 = DIRECTION ( 'NONE',  ( 0.000000000000000000, 1.000000000000000000, 0.000000000000000000 ) ) ;
#42282 = DIRECTION ( 'NONE',  ( 0.000000000000000000, 0.000000000000000000, 1.000000000000000000 ) ) ;
#42283 = FACE_OUTER_BOUND ( 'NONE', #100640, .T. ) ;
#42284 = AXIS2_PLACEMENT_3D ( 'NONE', #25205, #92027, #72403 ) ;
#42285 = DIRECTION ( 'NONE',  ( 0.000000000000000000, -0.9999939076577903929, 0.003490651415223739937 ) ) ;
#42286 = EDGE_LOOP ( 'NONE', ( #120249, #111869 ) ) ;
#42287 = CARTESIAN_POINT ( 'NONE',  ( -11.44999999999999751, 12.50000000000000000, 2.511473670974873507 ) ) ;
#42288 = ADVANCED_FACE ( 'NONE', ( #119124 ), #9167, .T. ) ;
#42290 = ADVANCED_FACE ( 'NONE', ( #28167 ), #18334, .F. ) ;
#42289 = CARTESIAN_POINT ( 'NONE',  ( 10.39999999999991154, 2.500000000000000000, -3.737306695894649700 ) ) ;
#42291 = CARTESIAN_POINT ( 'NONE',  ( -1.250000000000037970, 12.50000000000000000, 2.922977105672686982 ) ) ;
#42292 = CARTESIAN_POINT ( 'NONE',  ( -9.999999999999969802, 2.500000000000000000, 4.330127018922196314 ) ) ;
#42293 = AXIS2_PLACEMENT_3D ( 'NONE', #86743, #126678, #47473 ) ;
#42294 = CONICAL_SURFACE ( 'NONE', #31826, 0.09999999999999982514, 0.003490658503988666988 ) ;
#42295 = ORIENTED_EDGE ( 'NONE', *, *, #100137, .T. ) ;
#42296 = DIRECTION ( 'NONE',  ( -4.274815082592931898E-19, -0.9999939076577903929, -0.003490651415223739937 ) ) ;
#42297 = AXIS2_PLACEMENT_3D ( 'NONE', #98283, #39403, #38087 ) ;
#42298 = AXIS2_PLACEMENT_3D ( 'NONE', #52739, #56441, #106824 ) ;
#42299 = CARTESIAN_POINT ( 'NONE',  ( -8.350000000000008527, 2.500000000000000000, 7.288010851410849256 ) ) ;
#42301 = ORIENTED_EDGE ( 'NONE', *, *, #93303, .F. ) ;
#42300 = CARTESIAN_POINT ( 'NONE',  ( -5.850000000000018296, 2.500000000000000000, 1.372243186433545370 ) ) ;
#42302 = EDGE_CURVE ( 'NONE', #48001, #90845, #120043, .T. ) ;
#42303 = CIRCLE ( 'NONE', #2560, 0.06509327318403745899 ) ;
#42304 = ORIENTED_EDGE ( 'NONE', *, *, #2313, .T. ) ;
#42306 = AXIS2_PLACEMENT_3D ( 'NONE', #103516, #83860, #104156 ) ;
#42305 = DIRECTION ( 'NONE',  ( -4.274815082592931898E-19, -0.9999939076577903929, -0.003490651415223739937 ) ) ;
#42307 = ORIENTED_EDGE ( 'NONE', *, *, #96025, .T. ) ;
#42308 = CONICAL_SURFACE ( 'NONE', #69480, 0.09999999999999982514, 0.003490658503988666988 ) ;
#42310 = ORIENTED_EDGE ( 'NONE', *, *, #39816, .F. ) ;
#42309 = VECTOR ( 'NONE', #44498, 1000.000000000000000 ) ;
#42311 = CARTESIAN_POINT ( 'NONE',  ( 11.84999999999990372, 12.50000000000000000, -6.148780366869526226 ) ) ;
#42312 = AXIS2_PLACEMENT_3D ( 'NONE', #11088, #100754, #39315 ) ;
#42313 = CARTESIAN_POINT ( 'NONE',  ( 19.51231976789321720, 0.5900868802296501681, -4.348342248682749656 ) ) ;
#42314 = DIRECTION ( 'NONE',  ( 0.000000000000000000, -0.9999939076577903929, 0.003490651415223739937 ) ) ;
#42315 = CARTESIAN_POINT ( 'NONE',  ( -3.150000000000030109, 12.50000000000000000, -2.576566944158915184 ) ) ;
#42316 = ORIENTED_EDGE ( 'NONE', *, *, #38479, .F. ) ;
#42317 = CONICAL_SURFACE ( 'NONE', #90410, 0.1000000000000002554, 0.003490658503988666988 ) ;
#42318 = DIRECTION ( 'NONE',  ( 0.000000000000000000, -0.000000000000000000, 1.000000000000000000 ) ) ;
#42319 = ORIENTED_EDGE ( 'NONE', *, *, #69634, .T. ) ;
#42320 = DIRECTION ( 'NONE',  ( 0.000000000000000000, 0.000000000000000000, -1.000000000000000000 ) ) ;
#42321 = CARTESIAN_POINT ( 'NONE',  ( 186.3645833340161175, -6.668395609140180369, 3.849999999999994760 ) ) ;
#42322 = VERTEX_POINT ( 'NONE', #106707 ) ;
#42323 = EDGE_CURVE ( 'NONE', #17427, #51388, #99295, .T. ) ;
#42324 = ORIENTED_EDGE ( 'NONE', *, *, #71727, .F. ) ;
#42325 = VERTEX_POINT ( 'NONE', #96894 ) ;
#42326 = ORIENTED_EDGE ( 'NONE', *, *, #113486, .T. ) ;
#42327 = DIRECTION ( 'NONE',  ( 0.000000000000000000, 1.000000000000000000, 0.000000000000000000 ) ) ;
#42328 = CARTESIAN_POINT ( 'NONE',  ( 16.31212831497987281, 1.500000000000323297, 6.358242018216644809 ) ) ;
#42329 = DIRECTION ( 'NONE',  ( 0.000000000000000000, 0.000000000000000000, -1.000000000000000000 ) ) ;
#42330 = EDGE_CURVE ( 'NONE', #53498, #93285, #48444, .T. ) ;
#42331 = FACE_BOUND ( 'NONE', #111651, .T. ) ;
#42332 = ORIENTED_EDGE ( 'NONE', *, *, #83726, .F. ) ;
#42333 = CARTESIAN_POINT ( 'NONE',  ( 184.1979166673494603, 6.668395609140176816, 3.850000000000000977 ) ) ;
#42334 = ADVANCED_FACE ( 'NONE', ( #88348 ), #47165, .T. ) ;
#42335 = DIRECTION ( 'NONE',  ( 0.000000000000000000, 1.000000000000000000, 0.000000000000000000 ) ) ;
#42336 = CARTESIAN_POINT ( 'NONE',  ( 3.149999999999944400, 2.500000000000000000, 2.511473670974873507 ) ) ;
#42337 = VECTOR ( 'NONE', #109639, 1000.000000000000000 ) ;
#42338 = AXIS2_PLACEMENT_3D ( 'NONE', #97432, #36610, #86971 ) ;
#42339 = EDGE_CURVE ( 'NONE', #39960, #54236, #79834, .T. ) ;
#42341 = AXIS2_PLACEMENT_3D ( 'NONE', #22948, #23578, #42601 ) ;
#42340 = CARTESIAN_POINT ( 'NONE',  ( 6.449999999999933564, 2.500000000000000000, -6.941600689897078347 ) ) ;
#42342 = EDGE_CURVE ( 'NONE', #54324, #85725, #39308, .T. ) ;
#42343 = DIRECTION ( 'NONE',  ( 0.000000000000000000, 0.000000000000000000, 1.000000000000000000 ) ) ;
#42344 = ADVANCED_FACE ( 'NONE', ( #58278 ), #68723, .T. ) ;
#42345 = DIRECTION ( 'NONE',  ( 0.000000000000000000, 0.000000000000000000, -1.000000000000000000 ) ) ;
#42346 = AXIS2_PLACEMENT_3D ( 'NONE', #95549, #16312, #56255 ) ;
#42348 = CARTESIAN_POINT ( 'NONE',  ( -1.650000000000035660, 12.50000000000000000, 7.188010851410848723 ) ) ;
#42347 = AXIS2_PLACEMENT_3D ( 'NONE', #25361, #77062, #116322 ) ;
#42349 = EDGE_CURVE ( 'NONE', #123082, #117024, #59520, .T. ) ;
#42350 = ORIENTED_EDGE ( 'NONE', *, *, #80467, .F. ) ;
#42351 = ORIENTED_EDGE ( 'NONE', *, *, #91059, .T. ) ;
#42352 = ORIENTED_EDGE ( 'NONE', *, *, #8881, .T. ) ;
#42353 = VERTEX_POINT ( 'NONE', #108005 ) ;
#42354 = ORIENTED_EDGE ( 'NONE', *, *, #73892, .T. ) ;
#42355 = DIRECTION ( 'NONE',  ( 0.000000000000000000, -1.000000000000000000, 0.000000000000000000 ) ) ;
#42356 = CIRCLE ( 'NONE', #117532, 1.000000000000000444 ) ;
#42357 = LINE ( 'NONE', #33813, #73785 ) ;
#42358 = VERTEX_POINT ( 'NONE', #17008 ) ;
#42359 = FACE_BOUND ( 'NONE', #11392, .T. ) ;
#42360 = EDGE_CURVE ( 'NONE', #41081, #20554, #42885, .T. ) ;
#42361 = AXIS2_PLACEMENT_3D ( 'NONE', #77671, #117576, #27936 ) ;
#42362 = CARTESIAN_POINT ( 'NONE',  ( 4.599999999999936584, 12.50000000000000000, 3.637306695894644726 ) ) ;
#42363 = ORIENTED_EDGE ( 'NONE', *, *, #28012, .T. ) ;
#42364 = CARTESIAN_POINT ( 'NONE',  ( -4.150000000000025224, 2.500000000000000000, 5.702370205355745014 ) ) ;
#42365 = DIRECTION ( 'NONE',  ( -4.274815082592931898E-19, -0.9999939076577903929, -0.003490651415223739937 ) ) ;
#42366 = CARTESIAN_POINT ( 'NONE',  ( 5.849999999999933920, 2.500000000000000000, 5.902370205355745192 ) ) ;
#42367 = EDGE_LOOP ( 'NONE', ( #22922, #22195, #4388, #9250 ) ) ;
#42368 = DIRECTION ( 'NONE',  ( 0.000000000000000000, 1.000000000000000000, 0.000000000000000000 ) ) ;
#42369 = CONICAL_SURFACE ( 'NONE', #115501, 0.09999999999999999167, 0.003490658503988666988 ) ;
#42370 = ORIENTED_EDGE ( 'NONE', *, *, #93610, .T. ) ;
#42371 = EDGE_LOOP ( 'NONE', ( #29815, #118430 ) ) ;
#42372 = ORIENTED_EDGE ( 'NONE', *, *, #53539, .F. ) ;
#42373 = CARTESIAN_POINT ( 'NONE',  ( -3.350000000000028511, 2.500000000000000000, 1.472243186433545459 ) ) ;
#42374 = CARTESIAN_POINT ( 'NONE',  ( -7.900000000000014566, 2.500000000000000000, -4.922947341949753586 ) ) ;
#42375 = CARTESIAN_POINT ( 'NONE',  ( 13.94999999999989626, 2.500000000000000000, 2.411473670974873862 ) ) ;
#42376 = ORIENTED_EDGE ( 'NONE', *, *, #86841, .F. ) ;
#42377 = CARTESIAN_POINT ( 'NONE',  ( 3.349999999999941913, 12.50000000000000000, 6.430097255199259010 ) ) ;
#42378 = AXIS2_PLACEMENT_3D ( 'NONE', #66428, #51334, #20565 ) ;
#42379 = AXIS2_PLACEMENT_3D ( 'NONE', #69710, #7550, #78906 ) ;
#42380 = CARTESIAN_POINT ( 'NONE',  ( -4.350000000000027178, 12.50000000000000000, -6.083687093685488989 ) ) ;
#42381 = DIRECTION ( 'NONE',  ( 0.000000000000000000, 0.000000000000000000, -1.000000000000000000 ) ) ;
#42382 = CARTESIAN_POINT ( 'NONE',  ( 6.849999999999930367, 12.50000000000000000, -6.906693963081115939 ) ) ;
#42383 = CARTESIAN_POINT ( 'NONE',  ( 185.8229166673494319, -4.445597072760122614, 7.699999999999998401 ) ) ;
#42384 = ORIENTED_EDGE ( 'NONE', *, *, #63595, .F. ) ;
#42385 = FACE_OUTER_BOUND ( 'NONE', #49353, .T. ) ;
#42386 = CONICAL_SURFACE ( 'NONE', #6743, 0.09999999999999982514, 0.003490658503988666988 ) ;
#42387 = EDGE_LOOP ( 'NONE', ( #66407, #98271 ) ) ;
#42388 = DIRECTION ( 'NONE',  ( -0.000000000000000000, -1.000000000000000000, -0.000000000000000000 ) ) ;
#42389 = CONICAL_SURFACE ( 'NONE', #11059, 0.1000000000000002554, 0.003490658503988666988 ) ;
#42390 = AXIS2_PLACEMENT_3D ( 'NONE', #4670, #4046, #113360 ) ;
#42391 = ORIENTED_EDGE ( 'NONE', *, *, #86940, .T. ) ;
#42392 = AXIS2_PLACEMENT_3D ( 'NONE', #31045, #121323, #81419 ) ;
#42393 = EDGE_CURVE ( 'NONE', #88884, #46382, #88817, .T. ) ;
#42394 = ORIENTED_EDGE ( 'NONE', *, *, #102696, .T. ) ;
#42395 = DIRECTION ( 'NONE',  ( 0.000000000000000000, 1.000000000000000000, 0.000000000000000000 ) ) ;
#42396 = FACE_OUTER_BOUND ( 'NONE', #9386, .T. ) ;
#42397 = CARTESIAN_POINT ( 'NONE',  ( -14.14999999999998614, 12.50000000000000000, -2.857883832488651521 ) ) ;
#42398 = DIRECTION ( 'NONE',  ( -4.274815082592931898E-19, -0.9999939076577903929, -0.003490651415223739937 ) ) ;
#42399 = DIRECTION ( 'NONE',  ( -4.274815082592931898E-19, -0.9999939076577903929, -0.003490651415223739937 ) ) ;
#42400 = CIRCLE ( 'NONE', #111319, 0.09999999999999982514 ) ;
#42401 = ORIENTED_EDGE ( 'NONE', *, *, #5693, .T. ) ;
#42402 = EDGE_LOOP ( 'NONE', ( #92130, #19254 ) ) ;
#42403 = CIRCLE ( 'NONE', #109285, 0.1000000000000002554 ) ;
#42404 = EDGE_CURVE ( 'NONE', #56648, #102123, #46977, .T. ) ;
#42405 = CARTESIAN_POINT ( 'NONE',  ( 179.5000000000000000, -1.375000000000000000, 7.634788798650553154 ) ) ;
#42407 = CONICAL_SURFACE ( 'NONE', #100974, 0.1000000000000002554, 0.003490658503988666988 ) ;
#42406 = DIRECTION ( 'NONE',  ( 0.000000000000000000, -0.9999939076577903929, 0.003490651415223739937 ) ) ;
#42408 = CIRCLE ( 'NONE', #23612, 0.06509327318403745899 ) ;
#42409 = CIRCLE ( 'NONE', #36146, 0.06509327318403745899 ) ;
#42410 = DIRECTION ( 'NONE',  ( 0.000000000000000000, 0.000000000000000000, 1.000000000000000000 ) ) ;
#42412 = ORIENTED_EDGE ( 'NONE', *, *, #35053, .T. ) ;
#42411 = ORIENTED_EDGE ( 'NONE', *, *, #98927, .T. ) ;
#42413 = ORIENTED_EDGE ( 'NONE', *, *, #67624, .F. ) ;
#42414 = DIRECTION ( 'NONE',  ( 0.000000000000000000, 0.000000000000000000, 1.000000000000000000 ) ) ;
#42415 = AXIS2_PLACEMENT_3D ( 'NONE', #61517, #11749, #82449 ) ;
#42416 = ORIENTED_EDGE ( 'NONE', *, *, #72050, .F. ) ;
#42417 = FACE_OUTER_BOUND ( 'NONE', #81666, .T. ) ;
#42418 = FACE_OUTER_BOUND ( 'NONE', #112007, .T. ) ;
#42419 = DIRECTION ( 'NONE',  ( 0.000000000000000000, -0.9999939076577903929, 0.003490651415223739937 ) ) ;
#42420 = ORIENTED_EDGE ( 'NONE', *, *, #8631, .F. ) ;
#42421 = CONICAL_SURFACE ( 'NONE', #69590, 0.09999999999999982514, 0.003490658503988666988 ) ;
#42422 = DIRECTION ( 'NONE',  ( 0.000000000000000000, 1.000000000000000000, 0.000000000000000000 ) ) ;
#42423 = LINE ( 'NONE', #101338, #2662 ) ;
#42424 = CARTESIAN_POINT ( 'NONE',  ( 7.299999999999926104, 12.50000000000000000, -3.983716857408426293 ) ) ;
#42425 = CARTESIAN_POINT ( 'NONE',  ( -0.6000000000000323963, 2.500000000000000000, 0.3464101615137759604 ) ) ;
#42426 = DIRECTION ( 'NONE',  ( 0.000000000000000000, 0.000000000000000000, 1.000000000000000000 ) ) ;
#42427 = ORIENTED_EDGE ( 'NONE', *, *, #40470, .F. ) ;
#42428 = DIRECTION ( 'NONE',  ( -1.000000000000000000, -0.000000000000000000, -0.000000000000000000 ) ) ;
#42429 = DIRECTION ( 'NONE',  ( 0.000000000000000000, 0.000000000000000000, 1.000000000000000000 ) ) ;
#42430 = EDGE_LOOP ( 'NONE', ( #79271, #63940 ) ) ;
#42431 = VERTEX_POINT ( 'NONE', #67408 ) ;
#42432 = AXIS2_PLACEMENT_3D ( 'NONE', #108073, #33701, #73612 ) ;
#42433 = CONICAL_SURFACE ( 'NONE', #25688, 0.09999999999999982514, 0.003490658503988666988 ) ;
#42434 = CARTESIAN_POINT ( 'NONE',  ( 187.1302083336747444, -4.367472073101514418, -7.564683531250002702 ) ) ;
#42435 = LINE ( 'NONE', #51611, #69902 ) ;
#42436 = DIRECTION ( 'NONE',  ( 0.000000000000000000, 1.000000000000000000, 0.000000000000000000 ) ) ;
#42437 = CARTESIAN_POINT ( 'NONE',  ( -6.900000000000015454, 2.500000000000000000, 3.983716857408420076 ) ) ;
#42438 = DIRECTION ( 'NONE',  ( 0.000000000000000000, 0.000000000000000000, 1.000000000000000000 ) ) ;
#42439 = ADVANCED_FACE ( 'NONE', ( #107363 ), #89024, .T. ) ;
#42440 = CIRCLE ( 'NONE', #13449, 0.06509327318403745899 ) ;
#42441 = DIRECTION ( 'NONE',  ( 0.000000000000000000, 0.000000000000000000, 1.000000000000000000 ) ) ;
#42442 = AXIS2_PLACEMENT_3D ( 'NONE', #62802, #32714, #121069 ) ;
#42443 = DIRECTION ( 'NONE',  ( 0.000000000000000000, 0.000000000000000000, -1.000000000000000000 ) ) ;
#42444 = CARTESIAN_POINT ( 'NONE',  ( -2.050000000000033129, 2.500000000000000000, 2.065063509461097624 ) ) ;
#42445 = CONICAL_SURFACE ( 'NONE', #69612, 0.1000000000000000472, 0.003490658503988666988 ) ;
#42446 = AXIS2_PLACEMENT_3D ( 'NONE', #25188, #55943, #76243 ) ;
#42447 = ADVANCED_FACE ( 'NONE', ( #109296 ), #61645, .T. ) ;
#42448 = CARTESIAN_POINT ( 'NONE',  ( 2.899999999999944844, 12.50000000000000000, 3.637306695894644726 ) ) ;
#42449 = EDGE_CURVE ( 'NONE', #95328, #125928, #118062, .T. ) ;
#42450 = ORIENTED_EDGE ( 'NONE', *, *, #105442, .F. ) ;
#42451 = CIRCLE ( 'NONE', #15216, 0.06509327318403745899 ) ;
#42452 = ORIENTED_EDGE ( 'NONE', *, *, #92160, .T. ) ;
#42453 = CIRCLE ( 'NONE', #61218, 0.1000000000000002554 ) ;
#42454 = AXIS2_PLACEMENT_3D ( 'NONE', #97175, #95249, #35056 ) ;
#42455 = ORIENTED_EDGE ( 'NONE', *, *, #12762, .F. ) ;
#42456 = CONICAL_SURFACE ( 'NONE', #123999, 0.1000000000000002554, 0.003490658503988666988 ) ;
#42457 = ADVANCED_FACE ( 'NONE', ( #60227 ), #116009, .T. ) ;
#42458 = VERTEX_POINT ( 'NONE', #61509 ) ;
#42459 = ADVANCED_FACE ( 'NONE', ( #94638 ), #90879, .T. ) ;
#42460 = DIRECTION ( 'NONE',  ( 0.000000000000000000, 0.000000000000000000, 1.000000000000000000 ) ) ;
#42461 = DIRECTION ( 'NONE',  ( 0.000000000000000000, 0.000000000000000000, -1.000000000000000000 ) ) ;
#42462 = CONICAL_SURFACE ( 'NONE', #63377, 0.1000000000000002554, 0.003490658503988666988 ) ;
#42463 = ORIENTED_EDGE ( 'NONE', *, *, #83554, .T. ) ;
#42464 = CARTESIAN_POINT ( 'NONE',  ( 12.49999999999990408, 12.50000000000000000, 4.957854068765711553 ) ) ;
#42465 = EDGE_CURVE ( 'NONE', #97094, #37017, #80429, .T. ) ;
#42466 = DIRECTION ( 'NONE',  ( 0.000000000000000000, 0.000000000000000000, 1.000000000000000000 ) ) ;
#42468 = ORIENTED_EDGE ( 'NONE', *, *, #27082, .T. ) ;
#42467 = DIRECTION ( 'NONE',  ( 0.000000000000000000, -0.9999939076577903929, 0.003490651415223739937 ) ) ;
#42469 = ADVANCED_FACE ( 'NONE', ( #4967 ), #65825, .T. ) ;
#42470 = CARTESIAN_POINT ( 'NONE',  ( -4.150000000000024336, 2.500000000000000000, 1.472243186433545459 ) ) ;
#42471 = CARTESIAN_POINT ( 'NONE',  ( -13.74999999999998757, 2.500000000000000000, -2.857883832488651521 ) ) ;
#42472 = EDGE_LOOP ( 'NONE', ( #45860, #29040, #107385, #59336 ) ) ;
#42473 = ORIENTED_EDGE ( 'NONE', *, *, #18874, .F. ) ;
#42474 = ORIENTED_EDGE ( 'NONE', *, *, #10823, .T. ) ;
#42475 = ORIENTED_EDGE ( 'NONE', *, *, #32308, .T. ) ;
#42476 = DIRECTION ( 'NONE',  ( 0.000000000000000000, 0.000000000000000000, -1.000000000000000000 ) ) ;
#42478 = CONICAL_SURFACE ( 'NONE', #96729, 0.1000000000000002554, 0.003490658503988666988 ) ;
#42477 = DIRECTION ( 'NONE',  ( 0.000000000000000000, 0.000000000000000000, -1.000000000000000000 ) ) ;
#42479 = DIRECTION ( 'NONE',  ( 0.000000000000000000, 0.000000000000000000, 1.000000000000000000 ) ) ;
#42480 = AXIS2_PLACEMENT_3D ( 'NONE', #34959, #85949, #65014 ) ;
#42481 = DIRECTION ( 'NONE',  ( 1.000000000000000000, -0.000000000000000000, -0.000000000000000000 ) ) ;
#42482 = PRESENTATION_LAYER_ASSIGNMENT (  '', '', ( #124026 ) ) ;
#42483 = VERTEX_POINT ( 'NONE', #11741 ) ;
#42484 = DIRECTION ( 'NONE',  ( -0.000000000000000000, -1.000000000000000000, -0.000000000000000000 ) ) ;
#42485 = ORIENTED_EDGE ( 'NONE', *, *, #74813, .F. ) ;
#42486 = DIRECTION ( 'NONE',  ( 0.000000000000000000, 0.000000000000000000, 1.000000000000000000 ) ) ;
#42487 = DIRECTION ( 'NONE',  ( 0.000000000000000000, 1.000000000000000000, 0.000000000000000000 ) ) ;
#42488 = CARTESIAN_POINT ( 'NONE',  ( -1.050000000000037792, 2.500000000000000000, 1.918653347947321564 ) ) ;
#42489 = DIRECTION ( 'NONE',  ( 0.000000000000000000, 0.000000000000000000, -1.000000000000000000 ) ) ;
#42490 = VECTOR ( 'NONE', #15080, 1000.000000000000000 ) ;
#42491 = CONICAL_SURFACE ( 'NONE', #40342, 0.09999999999999999167, 0.003490658503988666988 ) ;
#42492 = ORIENTED_EDGE ( 'NONE', *, *, #95835, .T. ) ;
#42493 = AXIS2_PLACEMENT_3D ( 'NONE', #59042, #108764, #49237 ) ;
#42494 = VERTEX_POINT ( 'NONE', #121689 ) ;
#42495 = ORIENTED_EDGE ( 'NONE', *, *, #119006, .F. ) ;
#42496 = CARTESIAN_POINT ( 'NONE',  ( -11.44999999999999751, 12.50000000000000000, -2.446380397790836270 ) ) ;
#42497 = FACE_OUTER_BOUND ( 'NONE', #46220, .T. ) ;
#42498 = DIRECTION ( 'NONE',  ( 0.000000000000000000, 0.000000000000000000, -1.000000000000000000 ) ) ;
#42499 = FACE_BOUND ( 'NONE', #97956, .T. ) ;
#42500 = DIRECTION ( 'NONE',  ( 0.000000000000000000, 0.000000000000000000, 1.000000000000000000 ) ) ;
#42502 = CARTESIAN_POINT ( 'NONE',  ( 5.449999999999937117, 2.500000000000000000, -6.595190528383302109 ) ) ;
#42501 = AXIS2_PLACEMENT_3D ( 'NONE', #14563, #42783, #53229 ) ;
#42503 = ADVANCED_FACE ( 'NONE', ( #91595 ), #92949, .T. ) ;
#42504 = DIRECTION ( 'NONE',  ( 0.000000000000000000, 0.000000000000000000, -1.000000000000000000 ) ) ;
#42505 = AXIS2_PLACEMENT_3D ( 'NONE', #102375, #93202, #53913 ) ;
#42506 = AXIS2_PLACEMENT_3D ( 'NONE', #28428, #9425, #97159 ) ;
#42507 = AXIS2_PLACEMENT_3D ( 'NONE', #31931, #1804, #100025 ) ;
#42508 = EDGE_CURVE ( 'NONE', #92907, #15629, #113870, .T. ) ;
#42509 = EDGE_CURVE ( 'NONE', #54541, #21011, #107607, .T. ) ;
#42510 = CARTESIAN_POINT ( 'NONE',  ( -0.4500000000000397571, 2.500000000000000000, -6.495190528383302464 ) ) ;
#42511 = CARTESIAN_POINT ( 'NONE',  ( 184.1666666666666856, -6.668395609140176816, -3.850000000000003642 ) ) ;
#42512 = AXIS2_PLACEMENT_3D ( 'NONE', #112385, #122842, #23334 ) ;
#42513 = EDGE_CURVE ( 'NONE', #129360, #94388, #124335, .T. ) ;
#42514 = CARTESIAN_POINT ( 'NONE',  ( 8.149999999999920419, 12.50000000000000000, 6.841600689897072485 ) ) ;
#42515 = ORIENTED_EDGE ( 'NONE', *, *, #86935, .F. ) ;
#42516 = ADVANCED_FACE ( 'NONE', ( #22229 ), #67882, .T. ) ;
#42517 = DIRECTION ( 'NONE',  ( 0.000000000000000000, 0.000000000000000000, 1.000000000000000000 ) ) ;
#42518 = DIRECTION ( 'NONE',  ( 0.000000000000000000, 1.000000000000000000, 0.000000000000000000 ) ) ;
#42519 = AXIS2_PLACEMENT_3D ( 'NONE', #5003, #123492, #75051 ) ;
#42520 = ADVANCED_FACE ( 'NONE', ( #122359 ), #90953, .T. ) ;
#42521 = ORIENTED_EDGE ( 'NONE', *, *, #64751, .F. ) ;
#42522 = EDGE_LOOP ( 'NONE', ( #44760, #8526 ) ) ;
#42523 = CARTESIAN_POINT ( 'NONE',  ( 8.349999999999923261, 2.500000000000000000, -7.088010851410853519 ) ) ;
#42524 = DIRECTION ( 'NONE',  ( 0.000000000000000000, 0.000000000000000000, 1.000000000000000000 ) ) ;
#42525 = FACE_BOUND ( 'NONE', #114536, .T. ) ;
#42526 = CARTESIAN_POINT ( 'NONE',  ( -2.100000000000033396, 2.500000000000000000, -3.637306695894650055 ) ) ;
#42527 = EDGE_CURVE ( 'NONE', #23084, #125100, #26137, .T. ) ;
#42528 = ADVANCED_FACE ( 'NONE', ( #1277 ), #101357, .T. ) ;
#42530 = ORIENTED_EDGE ( 'NONE', *, *, #52511, .F. ) ;
#42529 = CONICAL_SURFACE ( 'NONE', #734, 0.1000000000000002554, 0.003490658503988666988 ) ;
#42532 = CIRCLE ( 'NONE', #75946, 0.06509327318403745899 ) ;
#42531 = CARTESIAN_POINT ( 'NONE',  ( 10.59999999999990905, 2.500000000000000000, 3.883716857408420431 ) ) ;
#42533 = DIRECTION ( 'NONE',  ( 0.000000000000000000, 0.000000000000000000, 1.000000000000000000 ) ) ;
#42534 = ORIENTED_EDGE ( 'NONE', *, *, #115326, .T. ) ;
#42535 = DIRECTION ( 'NONE',  ( -4.274815082592931898E-19, -0.9999939076577903929, -0.003490651415223739937 ) ) ;
#42536 = FACE_OUTER_BOUND ( 'NONE', #6263, .T. ) ;
#42537 = CIRCLE ( 'NONE', #126137, 0.1000000000000002554 ) ;
#42538 = CONICAL_SURFACE ( 'NONE', #84373, 0.09999999999999982514, 0.003490658503988666988 ) ;
#42539 = CIRCLE ( 'NONE', #96884, 0.06509327318403745899 ) ;
#42540 = AXIS2_PLACEMENT_3D ( 'NONE', #108896, #107628, #18601 ) ;
#42541 = ORIENTED_EDGE ( 'NONE', *, *, #54314, .T. ) ;
#42542 = DIRECTION ( 'NONE',  ( 0.000000000000000000, 1.000000000000000000, 0.000000000000000000 ) ) ;
#42543 = CARTESIAN_POINT ( 'NONE',  ( -7.050000000000013145, 2.500000000000000000, 6.495190528383297135 ) ) ;
#42544 = EDGE_CURVE ( 'NONE', #29211, #97516, #95091, .T. ) ;
#42545 = CIRCLE ( 'NONE', #48797, 0.06509327318403745899 ) ;
#42546 = ORIENTED_EDGE ( 'NONE', *, *, #13062, .F. ) ;
#42547 = DIRECTION ( 'NONE',  ( 0.000000000000000000, -0.9999939076577903929, 0.003490651415223739937 ) ) ;
#42548 = CARTESIAN_POINT ( 'NONE',  ( 5.649999999999936406, 2.500000000000000000, -6.048780366869526581 ) ) ;
#42549 = CARTESIAN_POINT ( 'NONE',  ( -6.850000000000013856, 2.500000000000000000, 6.841600689897072485 ) ) ;
#42550 = VECTOR ( 'NONE', #45626, 1000.000000000000000 ) ;
#42552 = ORIENTED_EDGE ( 'NONE', *, *, #39262, .F. ) ;
#42551 = VECTOR ( 'NONE', #102152, 1000.000000000000000 ) ;
#42553 = ORIENTED_EDGE ( 'NONE', *, *, #51387, .F. ) ;
#42554 = CARTESIAN_POINT ( 'NONE',  ( -0.8000000000000315747, 2.500000000000000000, 0.1000000000000000056 ) ) ;
#42555 = ORIENTED_EDGE ( 'NONE', *, *, #26963, .T. ) ;
#42556 = CARTESIAN_POINT ( 'NONE',  ( 8.749999999999953815, 2.500000000000000000, 6.395190528383296602 ) ) ;
#42557 = DIRECTION ( 'NONE',  ( 0.000000000000000000, 0.000000000000000000, -1.000000000000000000 ) ) ;
#42558 = DIRECTION ( 'NONE',  ( 0.000000000000000000, -0.000000000000000000, 1.000000000000000000 ) ) ;
#42559 = ORIENTED_EDGE ( 'NONE', *, *, #38518, .T. ) ;
#42560 = FACE_OUTER_BOUND ( 'NONE', #66766, .T. ) ;
#42561 = CARTESIAN_POINT ( 'NONE',  ( 5.449999999999937117, 12.50000000000000000, -6.560283801567339701 ) ) ;
#42562 = CARTESIAN_POINT ( 'NONE',  ( -14.14999999999998614, 2.500000000000000000, 1.472243186433549456 ) ) ;
#42563 =( BOUNDED_CURVE ( )  B_SPLINE_CURVE ( 2, ( #13600, #110046, #20378, #91046, #64006, #30856, #44358 ),
 .UNSPECIFIED., .F., .T. ) 
 B_SPLINE_CURVE_WITH_KNOTS ( ( 3, 2, 2, 3 ),
 ( 0.2857142857142859760, 0.3095238095238098119, 0.3333333333333335924, 0.3571428571428574283 ),
 .UNSPECIFIED. ) 
 CURVE ( )  GEOMETRIC_REPRESENTATION_ITEM ( )  RATIONAL_B_SPLINE_CURVE ( ( 0.9999999999999984457, 0.8660254037844402619, 1.000000000000000000, 0.8660254037844387076, 1.000000000000000000, 0.8660254037844371533, 1.000000000000001554 ) ) 
 REPRESENTATION_ITEM ( '' )  );
#42564 = DIRECTION ( 'NONE',  ( -0.000000000000000000, -1.000000000000000000, -0.000000000000000000 ) ) ;
#42565 = DIRECTION ( 'NONE',  ( 0.000000000000000000, 0.000000000000000000, 1.000000000000000000 ) ) ;
#42566 = DIRECTION ( 'NONE',  ( 0.000000000000000000, 0.000000000000000000, -1.000000000000000000 ) ) ;
#42567 = VECTOR ( 'NONE', #28970, 1000.000000000000000 ) ;
#42568 = ORIENTED_EDGE ( 'NONE', *, *, #98971, .T. ) ;
#42569 = EDGE_CURVE ( 'NONE', #45906, #126243, #31401, .T. ) ;
#42570 = ORIENTED_EDGE ( 'NONE', *, *, #5669, .F. ) ;
#42571 = DIRECTION ( 'NONE',  ( 0.000000000000000000, 0.000000000000000000, -1.000000000000000000 ) ) ;
#42572 = VERTEX_POINT ( 'NONE', #52316 ) ;
#42573 = DIRECTION ( 'NONE',  ( -4.274815082592931898E-19, -0.9999939076577903929, -0.003490651415223739937 ) ) ;
#42575 = ORIENTED_EDGE ( 'NONE', *, *, #76862, .T. ) ;
#42574 = EDGE_LOOP ( 'NONE', ( #20325, #72969 ) ) ;
#42576 = ORIENTED_EDGE ( 'NONE', *, *, #24774, .F. ) ;
#42577 = DIRECTION ( 'NONE',  ( 0.000000000000000000, 0.000000000000000000, -1.000000000000000000 ) ) ;
#42578 = AXIS2_PLACEMENT_3D ( 'NONE', #11269, #71474, #121228 ) ;
#42579 = DIRECTION ( 'NONE',  ( 0.000000000000000000, 0.000000000000000000, 1.000000000000000000 ) ) ;
#42580 = VECTOR ( 'NONE', #45552, 1000.000000000000000 ) ;
#42581 = CARTESIAN_POINT ( 'NONE',  ( 4.149999999999941735, 2.500000000000000000, -5.802370205355749988 ) ) ;
#42582 = DIRECTION ( 'NONE',  ( 0.000000000000000000, 1.000000000000000000, 0.000000000000000000 ) ) ;
#42583 = CARTESIAN_POINT ( 'NONE',  ( -1.050000000000037348, 12.50000000000000000, -2.576566944158915184 ) ) ;
#42584 = DIRECTION ( 'NONE',  ( -0.000000000000000000, 1.000000000000000000, -0.000000000000000000 ) ) ;
#42585 = CARTESIAN_POINT ( 'NONE',  ( 11.64999999999990621, 2.500000000000000000, 6.495190528383297135 ) ) ;
#42586 = DIRECTION ( 'NONE',  ( -0.000000000000000000, -1.000000000000000000, -0.000000000000000000 ) ) ;
#42587 = AXIS2_PLACEMENT_3D ( 'NONE', #15593, #45723, #104621 ) ;
#42588 = AXIS2_PLACEMENT_3D ( 'NONE', #5545, #55941, #43570 ) ;
#42589 = DIRECTION ( 'NONE',  ( 0.000000000000000000, 0.000000000000000000, 1.000000000000000000 ) ) ;
#42590 = AXIS2_PLACEMENT_3D ( 'NONE', #61224, #348, #52056 ) ;
#42591 = EDGE_LOOP ( 'NONE', ( #42743, #37752, #115653, #17855 ) ) ;
#42592 = VECTOR ( 'NONE', #101540, 1000.000000000000000 ) ;
#42593 = DIRECTION ( 'NONE',  ( 0.000000000000000000, -0.9999939076577903929, 0.003490651415223739937 ) ) ;
#42594 = ORIENTED_EDGE ( 'NONE', *, *, #71720, .F. ) ;
#42595 = ORIENTED_EDGE ( 'NONE', *, *, #13362, .F. ) ;
#42596 = DIRECTION ( 'NONE',  ( -0.000000000000000000, -1.000000000000000000, -0.000000000000000000 ) ) ;
#42598 = AXIS2_PLACEMENT_3D ( 'NONE', #54748, #105142, #25282 ) ;
#42597 = DIRECTION ( 'NONE',  ( -0.000000000000000000, 1.000000000000000000, -0.000000000000000000 ) ) ;
#42599 = DIRECTION ( 'NONE',  ( 0.000000000000000000, -0.9999939076577903929, 0.003490651415223739937 ) ) ;
#42600 = CARTESIAN_POINT ( 'NONE',  ( -5.600000000000020073, 12.50000000000000000, 4.676537180435972552 ) ) ;
#42601 = DIRECTION ( 'NONE',  ( 0.000000000000000000, 0.000000000000000000, 1.000000000000000000 ) ) ;
#42602 = CONICAL_SURFACE ( 'NONE', #113686, 0.09999999999999982514, 0.003490658503988666988 ) ;
#42603 = CARTESIAN_POINT ( 'NONE',  ( 185.9895833340161175, -4.445597072760145707, -7.699999999999951328 ) ) ;
#42604 = CIRCLE ( 'NONE', #19597, 0.06509327318403745899 ) ;
#42605 = DIRECTION ( 'NONE',  ( 0.000000000000000000, 1.000000000000000000, 0.000000000000000000 ) ) ;
#42606 = EDGE_LOOP ( 'NONE', ( #91113, #14487 ) ) ;
#42607 = VECTOR ( 'NONE', #29799, 1000.000000000000000 ) ;
#42608 = CIRCLE ( 'NONE', #19605, 0.06509327318403745899 ) ;
#42609 = ORIENTED_EDGE ( 'NONE', *, *, #28324, .T. ) ;
#42610 = EDGE_CURVE ( 'NONE', #112676, #45445, #20924, .T. ) ;
#42611 = EDGE_LOOP ( 'NONE', ( #76697, #126730 ) ) ;
#42612 = ORIENTED_EDGE ( 'NONE', *, *, #5528, .T. ) ;
#42613 = ADVANCED_FACE ( 'NONE', ( #71298 ), #109666, .T. ) ;
#42614 = ORIENTED_EDGE ( 'NONE', *, *, #118237, .T. ) ;
#42615 = ADVANCED_FACE ( 'NONE', ( #24631 ), #53241, .T. ) ;
#42616 = FACE_OUTER_BOUND ( 'NONE', #60655, .T. ) ;
#42617 = PLANE ( 'NONE',  #122955 ) ;
#42618 = CARTESIAN_POINT ( 'NONE',  ( -6.071532165918824830E-15, 2.500000000000000000, -4.330127018922201643 ) ) ;
#42619 = DIRECTION ( 'NONE',  ( 0.000000000000000000, -0.000000000000000000, 1.000000000000000000 ) ) ;
#42620 = ADVANCED_FACE ( 'NONE', ( #66473 ), #63703, .T. ) ;
#42621 = CARTESIAN_POINT ( 'NONE',  ( 3.099999999999945466, 2.500000000000000000, -3.983716857408426293 ) ) ;
#42623 = ORIENTED_EDGE ( 'NONE', *, *, #95989, .F. ) ;
#42622 = EDGE_CURVE ( 'NONE', #99145, #93739, #81892, .T. ) ;
#42625 = VECTOR ( 'NONE', #91510, 1000.000000000000000 ) ;
#42624 = CARTESIAN_POINT ( 'NONE',  ( 5.199999999999931788, 12.50000000000000000, 4.741630453620009789 ) ) ;
#42626 = EDGE_CURVE ( 'NONE', #98546, #54633, #16068, .T. ) ;
#42627 = DIRECTION ( 'NONE',  ( 0.000000000000000000, 0.000000000000000000, 1.000000000000000000 ) ) ;
#42628 = ADVANCED_FACE ( 'NONE', ( #96565 ), #22032, .T. ) ;
#42629 = DIRECTION ( 'NONE',  ( 0.000000000000000000, 0.000000000000000000, 1.000000000000000000 ) ) ;
#42630 = DIRECTION ( 'NONE',  ( 0.000000000000000000, 0.000000000000000000, -1.000000000000000000 ) ) ;
#42631 = EDGE_LOOP ( 'NONE', ( #17043, #120365 ) ) ;
#42632 = CONICAL_SURFACE ( 'NONE', #67634, 0.1000000000000000472, 0.003490658503988666988 ) ;
#42633 = CIRCLE ( 'NONE', #61501, 0.1000000000000000472 ) ;
#42634 = AXIS2_PLACEMENT_3D ( 'NONE', #42136, #70948, #1552 ) ;
#42635 = ORIENTED_EDGE ( 'NONE', *, *, #109961, .T. ) ;
#42636 = AXIS2_PLACEMENT_3D ( 'NONE', #87451, #10198, #9557 ) ;
#42637 = EDGE_LOOP ( 'NONE', ( #42866, #99781, #6600, #56266 ) ) ;
#42638 = CONICAL_SURFACE ( 'NONE', #59364, 0.09999999999999999167, 0.003490658503988666988 ) ;
#42639 = LINE ( 'NONE', #101538, #101105 ) ;
#42640 = EDGE_CURVE ( 'NONE', #21274, #106026, #65167, .T. ) ;
#42641 = ORIENTED_EDGE ( 'NONE', *, *, #116746, .T. ) ;
#42642 = CARTESIAN_POINT ( 'NONE',  ( 5.449999999999936229, 2.500000000000000000, -2.165063509461101710 ) ) ;
#42643 = CARTESIAN_POINT ( 'NONE',  ( -2.500000000000031086, 2.500000000000000000, 3.537306695894645081 ) ) ;
#42644 = AXIS2_PLACEMENT_3D ( 'NONE', #96855, #117128, #67366 ) ;
#42645 = AXIS2_PLACEMENT_3D ( 'NONE', #46430, #64142, #53686 ) ;
#42646 = AXIS2_PLACEMENT_3D ( 'NONE', #125874, #36234, #7389 ) ;
#42647 = CIRCLE ( 'NONE', #115775, 0.09999999999999982514 ) ;
#42648 = ORIENTED_EDGE ( 'NONE', *, *, #47946, .T. ) ;
#42649 = FACE_OUTER_BOUND ( 'NONE', #78449, .T. ) ;
#42650 = DIRECTION ( 'NONE',  ( 0.000000000000000000, -0.9999939076577903929, 0.003490651415223739937 ) ) ;
#42651 = CARTESIAN_POINT ( 'NONE',  ( -8.550000000000013145, 12.50000000000000000, -1.818653347947326138 ) ) ;
#42652 = CARTESIAN_POINT ( 'NONE',  ( -0.8500000000000395017, 2.500000000000000000, 2.065063509461097624 ) ) ;
#42653 = CARTESIAN_POINT ( 'NONE',  ( -8.950000000000011724, 2.500000000000000000, -6.148780366869520897 ) ) ;
#42654 = VERTEX_POINT ( 'NONE', #55377 ) ;
#42655 = ORIENTED_EDGE ( 'NONE', *, *, #37156, .F. ) ;
#42656 = EDGE_CURVE ( 'NONE', #11179, #9679, #75639, .T. ) ;
#42657 = DIRECTION ( 'NONE',  ( 0.000000000000000000, 0.000000000000000000, 1.000000000000000000 ) ) ;
#42658 = LINE ( 'NONE', #32194, #12167 ) ;
#42659 = LINE ( 'NONE', #94297, #86840 ) ;
#42660 = CIRCLE ( 'NONE', #44798, 0.1000000000000000472 ) ;
#42661 = DIRECTION ( 'NONE',  ( 0.000000000000000000, 0.000000000000000000, 1.000000000000000000 ) ) ;
#42662 = ORIENTED_EDGE ( 'NONE', *, *, #24579, .T. ) ;
#42663 = ORIENTED_EDGE ( 'NONE', *, *, #14564, .F. ) ;
#42664 = EDGE_CURVE ( 'NONE', #29584, #93873, #97869, .T. ) ;
#42665 = CARTESIAN_POINT ( 'NONE',  ( 4.149999999999939959, 2.500000000000000000, 2.957883832488649389 ) ) ;
#42666 = DIRECTION ( 'NONE',  ( 0.000000000000000000, 0.000000000000000000, -1.000000000000000000 ) ) ;
#42667 = CARTESIAN_POINT ( 'NONE',  ( -11.84999999999999609, 12.50000000000000000, 6.148780366869520897 ) ) ;
#42668 = ADVANCED_FACE ( 'NONE', ( #115558 ), #105102, .T. ) ;
#42669 = LINE ( 'NONE', #113964, #88619 ) ;
#42670 = ORIENTED_EDGE ( 'NONE', *, *, #29390, .T. ) ;
#42671 = AXIS2_PLACEMENT_3D ( 'NONE', #50252, #40446, #30624 ) ;
#42672 = CIRCLE ( 'NONE', #78166, 0.1000000000000002554 ) ;
#42673 = CARTESIAN_POINT ( 'NONE',  ( 0.3999999999999628852, 12.50000000000000000, 0.6928203230275518099 ) ) ;
#42674 = ADVANCED_FACE ( 'NONE', ( #106402 ), #59703, .T. ) ;
#42675 = DIRECTION ( 'NONE',  ( -0.000000000000000000, 1.000000000000000000, -0.000000000000000000 ) ) ;
#42676 = ORIENTED_EDGE ( 'NONE', *, *, #45035, .F. ) ;
#42677 = DIRECTION ( 'NONE',  ( 0.000000000000000000, -0.9999939076577903929, 0.003490651415223739937 ) ) ;
#42678 = EDGE_CURVE ( 'NONE', #43625, #116926, #6885, .T. ) ;
#42679 = AXIS2_PLACEMENT_3D ( 'NONE', #50870, #121522, #53456 ) ;
#42680 = ORIENTED_EDGE ( 'NONE', *, *, #18548, .F. ) ;
#42681 = DIRECTION ( 'NONE',  ( 0.000000000000000000, -0.9999939076577903929, 0.003490651415223739937 ) ) ;
#42682 = EDGE_CURVE ( 'NONE', #122820, #122810, #88922, .T. ) ;
#42683 = AXIS2_PLACEMENT_3D ( 'NONE', #95195, #5502, #113539 ) ;
#42684 = ADVANCED_FACE ( 'NONE', ( #126031 ), #49231, .T. ) ;
#42685 = EDGE_CURVE ( 'NONE', #120064, #14553, #38774, .T. ) ;
#42686 = ORIENTED_EDGE ( 'NONE', *, *, #69846, .T. ) ;
#42687 = FACE_OUTER_BOUND ( 'NONE', #19806, .T. ) ;
#42688 = DIRECTION ( 'NONE',  ( 0.000000000000000000, 0.000000000000000000, 1.000000000000000000 ) ) ;
#42689 = VERTEX_POINT ( 'NONE', #86757 ) ;
#42690 = VERTEX_POINT ( 'NONE', #36397 ) ;
#42691 = CARTESIAN_POINT ( 'NONE',  ( 187.2552083336747444, 6.551208109652275624, -3.782341765624998686 ) ) ;
#42692 = DIRECTION ( 'NONE',  ( 0.000000000000000000, -0.000000000000000000, 1.000000000000000000 ) ) ;
#42693 = EDGE_CURVE ( 'NONE', #61962, #97794, #51290, .T. ) ;
#42694 = CARTESIAN_POINT ( 'NONE',  ( 186.9218750003414016, 0.000000000000000000, 7.564683531250000925 ) ) ;
#42695 = CARTESIAN_POINT ( 'NONE',  ( 185.0677083336747160, -4.367472073101514418, -7.564683531250002702 ) ) ;
#42696 = VECTOR ( 'NONE', #121199, 1000.000000000000000 ) ;
#42698 = CONICAL_SURFACE ( 'NONE', #99118, 0.09999999999999982514, 0.003490658503988666988 ) ;
#42697 = CARTESIAN_POINT ( 'NONE',  ( 0.3999999999999563904, 2.500000000000000000, 3.637306695894644726 ) ) ;
#42699 = AXIS2_PLACEMENT_3D ( 'NONE', #38822, #8653, #66935 ) ;
#42700 = CARTESIAN_POINT ( 'NONE',  ( -1.250000000000001554, 2.500000000000000000, 6.495190528383297135 ) ) ;
#42701 = DIRECTION ( 'NONE',  ( 0.000000000000000000, -0.000000000000000000, 1.000000000000000000 ) ) ;
#42702 = LINE ( 'NONE', #30937, #39031 ) ;
#42703 = VECTOR ( 'NONE', #88552, 1000.000000000000000 ) ;
#42704 = PLANE ( 'NONE',  #123673 ) ;
#42705 = AXIS2_PLACEMENT_3D ( 'NONE', #101249, #41705, #11574 ) ;
#42706 = ORIENTED_EDGE ( 'NONE', *, *, #79572, .T. ) ;
#42707 = ORIENTED_EDGE ( 'NONE', *, *, #32582, .F. ) ;
#42708 = FACE_OUTER_BOUND ( 'NONE', #7312, .T. ) ;
#42709 = EDGE_LOOP ( 'NONE', ( #95631, #85727 ) ) ;
#42710 = DIRECTION ( 'NONE',  ( -4.274815082592931898E-19, -0.9999939076577903929, -0.003490651415223739937 ) ) ;
#42711 = CARTESIAN_POINT ( 'NONE',  ( 7.499999999999925393, 2.500000000000000000, -3.537306695894649966 ) ) ;
#42712 = DIRECTION ( 'NONE',  ( -0.000000000000000000, 1.000000000000000000, -0.000000000000000000 ) ) ;
#42714 = ORIENTED_EDGE ( 'NONE', *, *, #124308, .T. ) ;
#42713 = ORIENTED_EDGE ( 'NONE', *, *, #45298, .F. ) ;
#42715 = FACE_BOUND ( 'NONE', #99298, .T. ) ;
#42716 = ORIENTED_EDGE ( 'NONE', *, *, #101863, .F. ) ;
#42717 = CARTESIAN_POINT ( 'NONE',  ( 11.89999999999990798, 12.50000000000000000, 3.983716857408420964 ) ) ;
#42718 = CARTESIAN_POINT ( 'NONE',  ( -0.4000000000000331624, 2.500000000000000000, -0.6928203230275519209 ) ) ;
#42719 = DIRECTION ( 'NONE',  ( 0.000000000000000000, 0.000000000000000000, 1.000000000000000000 ) ) ;
#42720 = DIRECTION ( 'NONE',  ( 0.000000000000000000, 0.000000000000000000, 1.000000000000000000 ) ) ;
#42721 = DIRECTION ( 'NONE',  ( 0.000000000000000000, -0.9999939076577903929, 0.003490651415223739937 ) ) ;
#42722 = CARTESIAN_POINT ( 'NONE',  ( -10.84999999999999964, 2.500000000000000000, 7.188010851410848723 ) ) ;
#42723 = AXIS2_PLACEMENT_3D ( 'NONE', #44348, #82369, #62079 ) ;
#42724 = DIRECTION ( 'NONE',  ( 0.000000000000000000, 1.000000000000000000, 0.000000000000000000 ) ) ;
#42725 = DIRECTION ( 'NONE',  ( 0.000000000000000000, 1.000000000000000000, 0.000000000000000000 ) ) ;
#42726 = AXIS2_PLACEMENT_3D ( 'NONE', #97947, #118235, #8271 ) ;
#42727 = AXIS2_PLACEMENT_3D ( 'NONE', #85516, #123498, #94051 ) ;
#42728 = DIRECTION ( 'NONE',  ( 0.000000000000000000, 1.000000000000000000, 0.000000000000000000 ) ) ;
#42729 = DIRECTION ( 'NONE',  ( -4.274815082592931898E-19, -0.9999939076577903929, -0.003490651415223739937 ) ) ;
#42730 = DIRECTION ( 'NONE',  ( 0.000000000000000000, 1.000000000000000000, 0.000000000000000000 ) ) ;
#42731 = CIRCLE ( 'NONE', #76152, 0.06509327318403745899 ) ;
#42733 = VERTEX_POINT ( 'NONE', #67091 ) ;
#42732 = VECTOR ( 'NONE', #120198, 1000.000000000000000 ) ;
#42734 = VERTEX_POINT ( 'NONE', #107032 ) ;
#42735 = ADVANCED_FACE ( 'NONE', ( #17357 ), #57313, .T. ) ;
#42736 = EDGE_LOOP ( 'NONE', ( #48502, #83314, #115458, #40406 ) ) ;
#42738 = CARTESIAN_POINT ( 'NONE',  ( -1.900000000000034106, 12.50000000000000000, 0.3464101615137735735 ) ) ;
#42737 = AXIS2_PLACEMENT_3D ( 'NONE', #102460, #43556, #50783 ) ;
#42739 = ORIENTED_EDGE ( 'NONE', *, *, #37873, .F. ) ;
#42740 = DIRECTION ( 'NONE',  ( 0.000000000000000000, 0.000000000000000000, 1.000000000000000000 ) ) ;
#42742 = ORIENTED_EDGE ( 'NONE', *, *, #5274, .T. ) ;
#42741 = VERTEX_POINT ( 'NONE', #68405 ) ;
#42743 = ORIENTED_EDGE ( 'NONE', *, *, #122243, .F. ) ;
#42744 = CARTESIAN_POINT ( 'NONE',  ( -7.900000000000014566, 12.50000000000000000, -4.957854068765716882 ) ) ;
#42745 = CONICAL_SURFACE ( 'NONE', #90534, 0.1000000000000002554, 0.003490658503988666988 ) ;
#42746 = AXIS2_PLACEMENT_3D ( 'NONE', #35341, #25493, #85711 ) ;
#42747 = CIRCLE ( 'NONE', #57290, 0.1000000000000002554 ) ;
#42748 = CARTESIAN_POINT ( 'NONE',  ( 9.999999999999952038, 12.50000000000000000, -0.06509327318403970719 ) ) ;
#42749 = DIRECTION ( 'NONE',  ( -0.000000000000000000, 1.000000000000000000, -0.000000000000000000 ) ) ;
#42750 = CARTESIAN_POINT ( 'NONE',  ( 21.24754738303276724, -0.7337760880902383098, -4.182111650399352953 ) ) ;
#42751 = DIRECTION ( 'NONE',  ( -0.000000000000000000, -1.000000000000000000, -0.000000000000000000 ) ) ;
#42752 = VECTOR ( 'NONE', #39240, 1000.000000000000000 ) ;
#42753 = DIRECTION ( 'NONE',  ( 0.000000000000000000, 0.000000000000000000, 1.000000000000000000 ) ) ;
#42754 = EDGE_CURVE ( 'NONE', #28650, #66463, #29779, .T. ) ;
#42755 = VERTEX_POINT ( 'NONE', #69703 ) ;
#42756 = DIRECTION ( 'NONE',  ( 0.000000000000000000, 0.000000000000000000, -1.000000000000000000 ) ) ;
#42757 = VERTEX_POINT ( 'NONE', #98500 ) ;
#42758 = ORIENTED_EDGE ( 'NONE', *, *, #30480, .T. ) ;
#42759 = ORIENTED_EDGE ( 'NONE', *, *, #122854, .F. ) ;
#42760 = CARTESIAN_POINT ( 'NONE',  ( 185.1562500006828031, 8.891194145520236347, 5.444286225454521982E-16 ) ) ;
#42761 = EDGE_LOOP ( 'NONE', ( #36358, #63161 ) ) ;
#42762 = EDGE_LOOP ( 'NONE', ( #103215, #80588 ) ) ;
#42763 = ORIENTED_EDGE ( 'NONE', *, *, #121071, .F. ) ;
#42764 = CIRCLE ( 'NONE', #113839, 0.1000000000000002554 ) ;
#42765 = SURFACE_SIDE_STYLE ('',( #23094 ) ) ;
#42766 = DIRECTION ( 'NONE',  ( 0.000000000000000000, 1.000000000000000000, 0.000000000000000000 ) ) ;
#42767 = DIRECTION ( 'NONE',  ( 0.000000000000000000, 1.000000000000000000, 0.000000000000000000 ) ) ;
#42768 = CARTESIAN_POINT ( 'NONE',  ( 187.5000000000000000, 0.000000000000000000, -7.699999999999999289 ) ) ;
#42769 = CARTESIAN_POINT ( 'NONE',  ( 0.3999999999999628852, 2.500000000000000000, 0.6928203230275518099 ) ) ;
#42770 = CARTESIAN_POINT ( 'NONE',  ( 5.399999999999931966, 2.500000000000000000, 4.430127018922196847 ) ) ;
#42771 = DIRECTION ( 'NONE',  ( 0.000000000000000000, 0.000000000000000000, 1.000000000000000000 ) ) ;
#42772 = CIRCLE ( 'NONE', #11433, 0.06509327318403745899 ) ;
#42773 = CIRCLE ( 'NONE', #115891, 0.1000000000000002554 ) ;
#42774 = ORIENTED_EDGE ( 'NONE', *, *, #84262, .T. ) ;
#42775 = DIRECTION ( 'NONE',  ( -4.274815082592931898E-19, -0.9999939076577903929, -0.003490651415223739937 ) ) ;
#42776 = EDGE_CURVE ( 'NONE', #129065, #100019, #10750, .T. ) ;
#42777 = EDGE_LOOP ( 'NONE', ( #42739, #78610 ) ) ;
#42778 = CARTESIAN_POINT ( 'NONE',  ( -6.249999999999981348, 12.50000000000000000, 2.165063509461097713 ) ) ;
#42779 = VERTEX_POINT ( 'NONE', #21241 ) ;
#42780 = FACE_OUTER_BOUND ( 'NONE', #39101, .T. ) ;
#42781 = VERTEX_POINT ( 'NONE', #50706 ) ;
#42782 = EDGE_CURVE ( 'NONE', #97955, #24335, #76307, .T. ) ;
#42783 = DIRECTION ( 'NONE',  ( -0.000000000000000000, -1.000000000000000000, -0.000000000000000000 ) ) ;
#42784 = AXIS2_PLACEMENT_3D ( 'NONE', #72899, #63726, #84648 ) ;
#42785 = DIRECTION ( 'NONE',  ( 0.000000000000000000, -0.000000000000000000, 1.000000000000000000 ) ) ;
#42786 = ORIENTED_EDGE ( 'NONE', *, *, #9792, .T. ) ;
#42787 = EDGE_CURVE ( 'NONE', #57274, #38043, #9500, .T. ) ;
#42789 = ORIENTED_EDGE ( 'NONE', *, *, #7789, .F. ) ;
#42788 = ADVANCED_FACE ( 'NONE', ( #18669 ), #57532, .T. ) ;
#42790 = DIRECTION ( 'NONE',  ( 0.000000000000000000, 0.000000000000000000, 1.000000000000000000 ) ) ;
#42791 = DIRECTION ( 'NONE',  ( 0.000000000000000000, 0.000000000000000000, -1.000000000000000000 ) ) ;
#42792 = ADVANCED_FACE ( 'NONE', ( #19967 ), #8833, .T. ) ;
#42793 = DIRECTION ( 'NONE',  ( -0.000000000000000000, -1.000000000000000000, -0.000000000000000000 ) ) ;
#42794 = EDGE_CURVE ( 'NONE', #111573, #116963, #28286, .T. ) ;
#42795 = ADVANCED_FACE ( 'NONE', ( #119434 ), #61175, .T. ) ;
#42796 = CARTESIAN_POINT ( 'NONE',  ( 6.049999999999932321, 2.500000000000000000, 6.941600689897073018 ) ) ;
#42797 = DIRECTION ( 'NONE',  ( 0.000000000000000000, 0.000000000000000000, 1.000000000000000000 ) ) ;
#42798 = ORIENTED_EDGE ( 'NONE', *, *, #124733, .F. ) ;
#42799 = AXIS2_PLACEMENT_3D ( 'NONE', #21061, #42004, #12529 ) ;
#42800 = CARTESIAN_POINT ( 'NONE',  ( 4.149999999999939959, 2.500000000000000000, 2.857883832488649301 ) ) ;
#42801 = AXIS2_PLACEMENT_3D ( 'NONE', #4031, #24333, #103546 ) ;
#42802 = EDGE_CURVE ( 'NONE', #128741, #31897, #19880, .T. ) ;
#42803 = ORIENTED_EDGE ( 'NONE', *, *, #79038, .T. ) ;
#42804 = EDGE_CURVE ( 'NONE', #64073, #59105, #48788, .T. ) ;
#42805 = DIRECTION ( 'NONE',  ( 0.000000000000000000, -0.000000000000000000, 1.000000000000000000 ) ) ;
#42806 = CARTESIAN_POINT ( 'NONE',  ( -9.350000000000004974, 2.500000000000000000, 6.841600689897072485 ) ) ;
#42807 = EDGE_CURVE ( 'NONE', #76002, #127039, #66500, .T. ) ;
#42808 = CARTESIAN_POINT ( 'NONE',  ( 184.3385416670080872, 6.551208109652274736, 3.782341765625001351 ) ) ;
#42809 = CARTESIAN_POINT ( 'NONE',  ( 8.549999999999920774, 2.500000000000000000, -2.411473670974877859 ) ) ;
#42810 = CARTESIAN_POINT ( 'NONE',  ( -4.350000000000023626, 12.50000000000000000, 6.148780366869520897 ) ) ;
#42811 = DIRECTION ( 'NONE',  ( -0.000000000000000000, -1.000000000000000000, -0.000000000000000000 ) ) ;
#42812 = DIRECTION ( 'NONE',  ( 0.000000000000000000, 0.000000000000000000, 1.000000000000000000 ) ) ;
#42813 = ORIENTED_EDGE ( 'NONE', *, *, #59498, .T. ) ;
#42814 = DIRECTION ( 'NONE',  ( -0.000000000000000000, 1.000000000000000000, -0.000000000000000000 ) ) ;
#42816 = DIRECTION ( 'NONE',  ( -0.000000000000000000, -0.000000000000000000, -1.000000000000000000 ) ) ;
#42815 = AXIS2_PLACEMENT_3D ( 'NONE', #119684, #118402, #119059 ) ;
#42817 = CARTESIAN_POINT ( 'NONE',  ( 12.09999999999990550, 12.50000000000000000, 5.022947341949748790 ) ) ;
#42818 = CIRCLE ( 'NONE', #26063, 0.09999999999999982514 ) ;
#42819 = ORIENTED_EDGE ( 'NONE', *, *, #42942, .F. ) ;
#42820 = VECTOR ( 'NONE', #126627, 1000.000000000000000 ) ;
#42821 = AXIS2_PLACEMENT_3D ( 'NONE', #17400, #57348, #28538 ) ;
#42822 = DIRECTION ( 'NONE',  ( -0.000000000000000000, -1.000000000000000000, -0.000000000000000000 ) ) ;
#42823 = CIRCLE ( 'NONE', #115949, 0.06509327318403745899 ) ;
#42824 = AXIS2_PLACEMENT_3D ( 'NONE', #41904, #122393, #112573 ) ;
#42825 = VERTEX_POINT ( 'NONE', #89350 ) ;
#42826 = VECTOR ( 'NONE', #78164, 1000.000000000000000 ) ;
#42827 = ORIENTED_EDGE ( 'NONE', *, *, #75287, .F. ) ;
#42828 = DIRECTION ( 'NONE',  ( -0.000000000000000000, 1.000000000000000000, -0.000000000000000000 ) ) ;
#42829 = VECTOR ( 'NONE', #49711, 1000.000000000000000 ) ;
#42830 = EDGE_LOOP ( 'NONE', ( #100711, #115635, #48048, #119923 ) ) ;
#42831 = CARTESIAN_POINT ( 'NONE',  ( -5.600000000000020073, 2.500000000000000000, 0.2464101615137736789 ) ) ;
#42832 = DIRECTION ( 'NONE',  ( 0.000000000000000000, 0.000000000000000000, 1.000000000000000000 ) ) ;
#42833 = DIRECTION ( 'NONE',  ( -4.274815082592931898E-19, -0.9999939076577903929, -0.003490651415223739937 ) ) ;
#42834 = EDGE_LOOP ( 'NONE', ( #76133, #87431 ) ) ;
#42835 = CIRCLE ( 'NONE', #30301, 0.09999999999999982514 ) ;
#42836 = AXIS2_PLACEMENT_3D ( 'NONE', #47679, #7727, #31110 ) ;
#42837 = DIRECTION ( 'NONE',  ( 0.000000000000000000, 0.000000000000000000, 1.000000000000000000 ) ) ;
#42838 = CARTESIAN_POINT ( 'NONE',  ( 10.19999999999991402, 12.50000000000000000, 0.3464101615137735735 ) ) ;
#42839 = VECTOR ( 'NONE', #120838, 1000.000000000000000 ) ;
#42840 = EDGE_CURVE ( 'NONE', #51134, #65511, #70350, .T. ) ;
#42841 = ORIENTED_EDGE ( 'NONE', *, *, #121527, .F. ) ;
#42842 = EDGE_CURVE ( 'NONE', #115296, #123777, #13594, .T. ) ;
#42843 = ORIENTED_EDGE ( 'NONE', *, *, #44111, .T. ) ;
#42844 = ADVANCED_FACE ( 'NONE', ( #39632 ), #72208, .T. ) ;
#42845 = EDGE_LOOP ( 'NONE', ( #66251, #42416, #39914, #32661 ) ) ;
#42846 = FACE_OUTER_BOUND ( 'NONE', #2184, .T. ) ;
#42847 = FACE_OUTER_BOUND ( 'NONE', #38561, .T. ) ;
#42848 = DIRECTION ( 'NONE',  ( 0.000000000000000000, -0.9999939076577903929, 0.003490651415223739937 ) ) ;
#42849 = FACE_BOUND ( 'NONE', #40566, .T. ) ;
#42850 = VERTEX_POINT ( 'NONE', #50093 ) ;
#42851 = DIRECTION ( 'NONE',  ( 0.000000000000000000, 0.000000000000000000, -1.000000000000000000 ) ) ;
#42852 = DIRECTION ( 'NONE',  ( 0.000000000000000000, 0.000000000000000000, 1.000000000000000000 ) ) ;
#42853 = CIRCLE ( 'NONE', #57405, 0.1000000000000002554 ) ;
#42854 = ORIENTED_EDGE ( 'NONE', *, *, #117690, .T. ) ;
#42855 = EDGE_CURVE ( 'NONE', #8476, #81572, #15739, .T. ) ;
#42856 = DIRECTION ( 'NONE',  ( 0.000000000000000000, 0.000000000000000000, -1.000000000000000000 ) ) ;
#42857 = CARTESIAN_POINT ( 'NONE',  ( -12.89999999999999147, 2.500000000000000000, 3.637306695894644726 ) ) ;
#42858 = DIRECTION ( 'NONE',  ( -0.000000000000000000, -1.000000000000000000, -0.000000000000000000 ) ) ;
#42859 = DIRECTION ( 'NONE',  ( -0.000000000000000000, 1.000000000000000000, -0.000000000000000000 ) ) ;
#42860 = DIRECTION ( 'NONE',  ( 0.000000000000000000, 1.000000000000000000, 0.000000000000000000 ) ) ;
#42861 = CARTESIAN_POINT ( 'NONE',  ( 11.24999999999990585, 12.50000000000000000, -5.737276932171712751 ) ) ;
#42862 = DIRECTION ( 'NONE',  ( 0.000000000000000000, 0.000000000000000000, -1.000000000000000000 ) ) ;
#42863 = CIRCLE ( 'NONE', #51267, 0.06509327318403745899 ) ;
#42864 = ORIENTED_EDGE ( 'NONE', *, *, #90518, .F. ) ;
#42865 = VERTEX_POINT ( 'NONE', #83404 ) ;
#42866 = ORIENTED_EDGE ( 'NONE', *, *, #102191, .F. ) ;
#42867 = ORIENTED_EDGE ( 'NONE', *, *, #98933, .F. ) ;
#42868 = DIRECTION ( 'NONE',  ( 0.000000000000000000, 1.000000000000000000, 0.000000000000000000 ) ) ;
#42869 = PLANE ( 'NONE',  #43599 ) ;
#42870 = CARTESIAN_POINT ( 'NONE',  ( 11.84999999999990727, 12.50000000000000000, 6.776507416713035248 ) ) ;
#42871 = ORIENTED_EDGE ( 'NONE', *, *, #123535, .T. ) ;
#42872 = FACE_BOUND ( 'NONE', #5715, .T. ) ;
#42873 = ADVANCED_FACE ( 'NONE', ( #24473 ), #1596, .T. ) ;
#42874 = CARTESIAN_POINT ( 'NONE',  ( 184.5000000000000000, 0.000000000000000000, 0.000000000000000000 ) ) ;
#42875 = FACE_OUTER_BOUND ( 'NONE', #36657, .T. ) ;
#42876 = CIRCLE ( 'NONE', #93023, 0.09999999999999982514 ) ;
#42877 = DIRECTION ( 'NONE',  ( 0.000000000000000000, 1.000000000000000000, 0.000000000000000000 ) ) ;
#42878 = DIRECTION ( 'NONE',  ( 0.000000000000000000, 0.000000000000000000, -1.000000000000000000 ) ) ;
#42879 = CONICAL_SURFACE ( 'NONE', #97219, 0.1000000000000002554, 0.003490658503988666988 ) ;
#42880 = CARTESIAN_POINT ( 'NONE',  ( -7.950000000000016165, 12.50000000000000000, -6.560283801567334372 ) ) ;
#42881 = CARTESIAN_POINT ( 'NONE',  ( 10.19999999999991402, 2.500000000000000000, 0.2464101615137735679 ) ) ;
#42882 = CARTESIAN_POINT ( 'NONE',  ( -12.49999999999999289, 2.500000000000000000, 5.122947341949749323 ) ) ;
#42883 = CARTESIAN_POINT ( 'NONE',  ( 14.14999999999989377, 12.50000000000000000, -2.857883832488653741 ) ) ;
#42884 = EDGE_LOOP ( 'NONE', ( #47182, #93711, #23614, #92927 ) ) ;
#42885 = CIRCLE ( 'NONE', #122290, 0.1000000000000002554 ) ;
#42886 = EDGE_LOOP ( 'NONE', ( #46376, #84472 ) ) ;
#42887 = EDGE_LOOP ( 'NONE', ( #18894, #74442, #28949, #116817 ) ) ;
#42888 = AXIS2_PLACEMENT_3D ( 'NONE', #114168, #15939, #46712 ) ;
#42889 = ADVANCED_FACE ( 'NONE', ( #62481 ), #61750, .T. ) ;
#42890 = ORIENTED_EDGE ( 'NONE', *, *, #121513, .F. ) ;
#42891 = ORIENTED_EDGE ( 'NONE', *, *, #109572, .T. ) ;
#42892 = ORIENTED_EDGE ( 'NONE', *, *, #65718, .F. ) ;
#42893 = DIRECTION ( 'NONE',  ( 0.000000000000000000, 0.000000000000000000, 1.000000000000000000 ) ) ;
#42894 = ORIENTED_EDGE ( 'NONE', *, *, #92393, .T. ) ;
#42895 = ORIENTED_EDGE ( 'NONE', *, *, #50076, .T. ) ;
#42896 = DIRECTION ( 'NONE',  ( -4.274815082592931898E-19, -0.9999939076577903929, -0.003490651415223739937 ) ) ;
#42897 = DIRECTION ( 'NONE',  ( 0.000000000000000000, 0.000000000000000000, -1.000000000000000000 ) ) ;
#42898 = CARTESIAN_POINT ( 'NONE',  ( 185.7812500006828031, 0.000000000000000000, 7.700000000000000178 ) ) ;
#42899 = EDGE_CURVE ( 'NONE', #44047, #4826, #26226, .T. ) ;
#42900 = CONICAL_SURFACE ( 'NONE', #105569, 0.1000000000000002554, 0.003490658503988666988 ) ;
#42901 = ORIENTED_EDGE ( 'NONE', *, *, #32445, .F. ) ;
#42902 = CARTESIAN_POINT ( 'NONE',  ( 5.399999999999932854, 2.500000000000000000, 3.637306695894644726 ) ) ;
#42903 = EDGE_LOOP ( 'NONE', ( #108372, #70128, #110442, #68691 ) ) ;
#42905 = VERTEX_POINT ( 'NONE', #23834 ) ;
#42904 = AXIS2_PLACEMENT_3D ( 'NONE', #22810, #33895, #52253 ) ;
#42906 = DIRECTION ( 'NONE',  ( 0.000000000000000000, -0.9999939076577903929, 0.003490651415223739937 ) ) ;
#42907 = AXIS2_PLACEMENT_3D ( 'NONE', #99760, #120040, #47436 ) ;
#42908 = CONICAL_SURFACE ( 'NONE', #111844, 0.1000000000000002554, 0.003490658503988666988 ) ;
#42910 = ADVANCED_FACE ( 'NONE', ( #44104 ), #113958, .T. ) ;
#42909 = CARTESIAN_POINT ( 'NONE',  ( -2.050000000000032685, 12.50000000000000000, -6.495190528383302464 ) ) ;
#42911 = ORIENTED_EDGE ( 'NONE', *, *, #60821, .T. ) ;
#42912 = ORIENTED_EDGE ( 'NONE', *, *, #41878, .F. ) ;
#42913 = CARTESIAN_POINT ( 'NONE',  ( 9.149999999999915090, 12.50000000000000000, 6.495190528383297135 ) ) ;
#42914 = VECTOR ( 'NONE', #78330, 1000.000000000000000 ) ;
#42915 = AXIS2_PLACEMENT_3D ( 'NONE', #92935, #83114, #63469 ) ;
#42916 = VECTOR ( 'NONE', #20852, 1000.000000000000000 ) ;
#42917 = LINE ( 'NONE', #52074, #99752 ) ;
#42918 = DIRECTION ( 'NONE',  ( -0.000000000000000000, -1.000000000000000000, -0.000000000000000000 ) ) ;
#42919 = DIRECTION ( 'NONE',  ( 0.000000000000000000, -0.9999939076577903929, 0.003490651415223739937 ) ) ;
#42920 = CIRCLE ( 'NONE', #30298, 0.06509327318403745899 ) ;
#42921 = DIRECTION ( 'NONE',  ( 0.000000000000000000, 1.000000000000000000, 0.000000000000000000 ) ) ;
#42922 = ORIENTED_EDGE ( 'NONE', *, *, #128334, .T. ) ;
#42923 = CARTESIAN_POINT ( 'NONE',  ( 2.299999999999949640, 12.50000000000000000, -0.3464101615137782364 ) ) ;
#42924 = AXIS2_PLACEMENT_3D ( 'NONE', #32481, #71730, #20701 ) ;
#42925 = VECTOR ( 'NONE', #984, 1000.000000000000000 ) ;
#42926 = ORIENTED_EDGE ( 'NONE', *, *, #21934, .F. ) ;
#42927 = CARTESIAN_POINT ( 'NONE',  ( 87.50000000000001421, 6.099025433955699960, -4.412011999987998756 ) ) ;
#42928 = ADVANCED_FACE ( 'NONE', ( #82767 ), #24081, .T. ) ;
#42929 = ORIENTED_EDGE ( 'NONE', *, *, #382, .F. ) ;
#42930 = DIRECTION ( 'NONE',  ( 0.000000000000000000, 0.000000000000000000, -1.000000000000000000 ) ) ;
#42931 = CARTESIAN_POINT ( 'NONE',  ( -9.600000000000008527, 2.500000000000000000, -5.022947341949749678 ) ) ;
#42932 = AXIS2_PLACEMENT_3D ( 'NONE', #49223, #106813, #129075 ) ;
#42933 = CARTESIAN_POINT ( 'NONE',  ( -8.749999999999976907, 2.500000000000000000, -6.395190528383296602 ) ) ;
#42934 = CARTESIAN_POINT ( 'NONE',  ( -10.65000000000000213, 2.500000000000000000, 6.841600689897072485 ) ) ;
#42935 = ORIENTED_EDGE ( 'NONE', *, *, #91105, .F. ) ;
#42936 = EDGE_CURVE ( 'NONE', #39885, #95740, #92564, .T. ) ;
#42937 = FACE_OUTER_BOUND ( 'NONE', #127659, .T. ) ;
#42938 = DIRECTION ( 'NONE',  ( -0.000000000000000000, -1.000000000000000000, -0.000000000000000000 ) ) ;
#42939 = ORIENTED_EDGE ( 'NONE', *, *, #109686, .F. ) ;
#42940 = ORIENTED_EDGE ( 'NONE', *, *, #37666, .T. ) ;
#42941 = EDGE_CURVE ( 'NONE', #75000, #22575, #95179, .T. ) ;
#42943 = ORIENTED_EDGE ( 'NONE', *, *, #11788, .F. ) ;
#42942 = EDGE_CURVE ( 'NONE', #66987, #5464, #71636, .T. ) ;
#42944 = CARTESIAN_POINT ( 'NONE',  ( 17.50000000000000000, -0.9166666666666695162, 3.432456362931491700 ) ) ;
#42945 = DIRECTION ( 'NONE',  ( 0.000000000000000000, 0.000000000000000000, 1.000000000000000000 ) ) ;
#42946 = ADVANCED_FACE ( 'NONE', ( #112213 ), #74251, .T. ) ;
#42947 = CARTESIAN_POINT ( 'NONE',  ( 185.8593750003413732, 0.000000000000000000, 7.564683531250000925 ) ) ;
#42948 = ADVANCED_FACE ( 'NONE', ( #93223 ), #122471, .T. ) ;
#42949 = AXIS2_PLACEMENT_3D ( 'NONE', #116083, #85335, #26426 ) ;
#42950 = CARTESIAN_POINT ( 'NONE',  ( -5.000000000000023093, 2.500000000000000000, 0.6928203230275494784 ) ) ;
#42951 = CARTESIAN_POINT ( 'NONE',  ( -2.300000000000033573, 2.500000000000000000, -3.983716857408426293 ) ) ;
#42952 = DIRECTION ( 'NONE',  ( 0.000000000000000000, 0.000000000000000000, 1.000000000000000000 ) ) ;
#42953 = FACE_OUTER_BOUND ( 'NONE', #59571, .T. ) ;
#42954 = ADVANCED_FACE ( 'NONE', ( #91925 ), #63874, .T. ) ;
#42955 = EDGE_CURVE ( 'NONE', #76244, #3965, #82766, .T. ) ;
#42956 = AXIS2_PLACEMENT_3D ( 'NONE', #83887, #85817, #125733 ) ;
#42957 = EDGE_CURVE ( 'NONE', #89603, #59130, #103688, .T. ) ;
#42958 = VECTOR ( 'NONE', #112861, 1000.000000000000000 ) ;
#42959 = EDGE_CURVE ( 'NONE', #128096, #34323, #32607, .T. ) ;
#42960 = DIRECTION ( 'NONE',  ( -4.274815082592931898E-19, -0.9999939076577903929, -0.003490651415223739937 ) ) ;
#42961 = EDGE_CURVE ( 'NONE', #106163, #27262, #7426, .T. ) ;
#42962 = ORIENTED_EDGE ( 'NONE', *, *, #125825, .F. ) ;
#42963 = CARTESIAN_POINT ( 'NONE',  ( 15.19999999999989271, 12.50000000000000000, -0.4115034346978157509 ) ) ;
#42964 = CARTESIAN_POINT ( 'NONE',  ( -0.4000000000000404898, 12.50000000000000000, 4.957854068765711553 ) ) ;
#42965 = PLANE ( 'NONE',  #56918 ) ;
#42966 = PLANE ( 'NONE',  #4116 ) ;
#42967 = EDGE_CURVE ( 'NONE', #112113, #30658, #68070, .T. ) ;
#42968 = ORIENTED_EDGE ( 'NONE', *, *, #2932, .F. ) ;
#42969 = CARTESIAN_POINT ( 'NONE',  ( -2.300000000000032685, 12.50000000000000000, -0.3464101615137783474 ) ) ;
#42970 = VECTOR ( 'NONE', #10575, 1000.000000000000000 ) ;
#42971 = AXIS2_PLACEMENT_3D ( 'NONE', #24657, #94038, #105792 ) ;
#42972 = DIRECTION ( 'NONE',  ( 0.000000000000000000, -0.000000000000000000, 1.000000000000000000 ) ) ;
#42974 = EDGE_LOOP ( 'NONE', ( #99479, #40980, #32622, #94285 ) ) ;
#42973 = DIRECTION ( 'NONE',  ( 0.000000000000000000, 0.000000000000000000, 1.000000000000000000 ) ) ;
#42975 = ORIENTED_EDGE ( 'NONE', *, *, #125098, .T. ) ;
#42976 = CARTESIAN_POINT ( 'NONE',  ( 9.149999999999920419, 2.500000000000000000, -5.802370205355749988 ) ) ;
#42977 = AXIS2_PLACEMENT_3D ( 'NONE', #116213, #77575, #84825 ) ;
#42978 = CIRCLE ( 'NONE', #49232, 0.09999999999999982514 ) ;
#42979 = ORIENTED_EDGE ( 'NONE', *, *, #67633, .T. ) ;
#42980 = VERTEX_POINT ( 'NONE', #33650 ) ;
#42981 = DIRECTION ( 'NONE',  ( 0.000000000000000000, -0.9999939076577903929, 0.003490651415223739937 ) ) ;
#42982 = CARTESIAN_POINT ( 'NONE',  ( -3.150000000000030109, 12.50000000000000000, -2.511473670974877948 ) ) ;
#42983 = DIRECTION ( 'NONE',  ( 0.000000000000000000, 0.000000000000000000, 1.000000000000000000 ) ) ;
#42984 = CARTESIAN_POINT ( 'NONE',  ( 3.549999999999943867, 12.50000000000000000, -1.818653347947326138 ) ) ;
#42985 = ORIENTED_EDGE ( 'NONE', *, *, #78799, .F. ) ;
#42986 = AXIS2_PLACEMENT_3D ( 'NONE', #71855, #12266, #22127 ) ;
#42987 = FACE_OUTER_BOUND ( 'NONE', #115780, .T. ) ;
#42989 = EDGE_LOOP ( 'NONE', ( #50452, #8572, #78959, #57376 ) ) ;
#42988 = DIRECTION ( 'NONE',  ( 0.000000000000000000, 0.000000000000000000, -1.000000000000000000 ) ) ;
#42990 = CARTESIAN_POINT ( 'NONE',  ( 16.55874544816223448, 0.4845305829267578801, 6.091953208799004926 ) ) ;
#42991 = DIRECTION ( 'NONE',  ( 0.000000000000000000, 0.000000000000000000, 1.000000000000000000 ) ) ;
#42992 = AXIS2_PLACEMENT_3D ( 'NONE', #107923, #86993, #9078 ) ;
#42993 = ORIENTED_EDGE ( 'NONE', *, *, #62769, .F. ) ;
#42994 = EDGE_CURVE ( 'NONE', #118519, #9515, #120316, .T. ) ;
#42995 = AXIS2_PLACEMENT_3D ( 'NONE', #27078, #48016, #48652 ) ;
#42996 = VERTEX_POINT ( 'NONE', #34310 ) ;
#42997 = CIRCLE ( 'NONE', #61855, 0.1000000000000002554 ) ;
#42999 = ORIENTED_EDGE ( 'NONE', *, *, #71949, .F. ) ;
#42998 = ADVANCED_FACE ( 'NONE', ( #55228 ), #36701, .T. ) ;
#43000 = ORIENTED_EDGE ( 'NONE', *, *, #35785, .F. ) ;
#43001 = CARTESIAN_POINT ( 'NONE',  ( 11.04999999999990834, 2.500000000000000000, 1.818653347947321475 ) ) ;
#43002 = CARTESIAN_POINT ( 'NONE',  ( 15.83209681635555377, 2.499999999999999556, 5.404881881984140435 ) ) ;
#43003 = CARTESIAN_POINT ( 'NONE',  ( 8.149999999999923972, 12.50000000000000000, 2.511473670974873507 ) ) ;
#43004 = FACE_BOUND ( 'NONE', #99881, .T. ) ;
#43005 = ORIENTED_EDGE ( 'NONE', *, *, #985, .F. ) ;
#43006 = CARTESIAN_POINT ( 'NONE',  ( 185.6562500006828316, 8.891194145520236347, 5.444286225454521982E-16 ) ) ;
#43007 = CARTESIAN_POINT ( 'NONE',  ( -9.800000000000006040, 2.500000000000000000, 0.4464101615137735513 ) ) ;
#43008 = CARTESIAN_POINT ( 'NONE',  ( 10.64999999999991331, 2.500000000000000000, 6.148780366869520897 ) ) ;
#43010 = EDGE_CURVE ( 'NONE', #13366, #26403, #24165, .T. ) ;
#43009 = VECTOR ( 'NONE', #87158, 1000.000000000000000 ) ;
#43011 = CARTESIAN_POINT ( 'NONE',  ( -0.6000000000000388356, 2.500000000000000000, 4.083716857408421497 ) ) ;
#43012 = VECTOR ( 'NONE', #63219, 1000.000000000000000 ) ;
#43013 = LINE ( 'NONE', #90787, #96928 ) ;
#43014 = DIRECTION ( 'NONE',  ( 0.000000000000000000, 0.000000000000000000, -1.000000000000000000 ) ) ;
#43015 = AXIS2_PLACEMENT_3D ( 'NONE', #16012, #97806, #127285 ) ;
#43016 = AXIS2_PLACEMENT_3D ( 'NONE', #106273, #56520, #47359 ) ;
#43017 = DIRECTION ( 'NONE',  ( -0.000000000000000000, 1.000000000000000000, -0.000000000000000000 ) ) ;
#43018 = AXIS2_PLACEMENT_3D ( 'NONE', #8717, #66370, #118046 ) ;
#43019 = ORIENTED_EDGE ( 'NONE', *, *, #49282, .F. ) ;
#43020 = ORIENTED_EDGE ( 'NONE', *, *, #119132, .T. ) ;
#43021 = VERTEX_POINT ( 'NONE', #46689 ) ;
#43022 = EDGE_LOOP ( 'NONE', ( #105006, #10359, #10498, #32605 ) ) ;
#43023 = AXIS2_PLACEMENT_3D ( 'NONE', #95573, #3321, #93000 ) ;
#43024 = VERTEX_POINT ( 'NONE', #4808 ) ;
#43025 = DIRECTION ( 'NONE',  ( 0.000000000000000000, 0.000000000000000000, 1.000000000000000000 ) ) ;
#43026 = DIRECTION ( 'NONE',  ( 0.000000000000000000, -0.9999939076577903929, 0.003490651415223739937 ) ) ;
#43027 = ORIENTED_EDGE ( 'NONE', *, *, #114636, .F. ) ;
#43028 = FACE_BOUND ( 'NONE', #71927, .T. ) ;
#43029 = PLANE ( 'NONE',  #110467 ) ;
#43030 = EDGE_LOOP ( 'NONE', ( #53489, #7251, #5658, #26336 ) ) ;
#43031 = CARTESIAN_POINT ( 'NONE',  ( 7.099999999999927702, 12.50000000000000000, 5.022947341949748790 ) ) ;
#43032 = DIRECTION ( 'NONE',  ( -0.000000000000000000, -1.000000000000000000, -0.000000000000000000 ) ) ;
#43033 = CARTESIAN_POINT ( 'NONE',  ( 4.799999999999935874, 12.50000000000000000, 0.3464101615137735735 ) ) ;
#43035 = ORIENTED_EDGE ( 'NONE', *, *, #34649, .T. ) ;
#43034 = CIRCLE ( 'NONE', #116153, 0.09999999999999999167 ) ;
#43036 = DIRECTION ( 'NONE',  ( -0.000000000000000000, -1.000000000000000000, -0.000000000000000000 ) ) ;
#43037 = EDGE_CURVE ( 'NONE', #23590, #15508, #9593, .T. ) ;
#43038 = ORIENTED_EDGE ( 'NONE', *, *, #68365, .T. ) ;
#43039 = ORIENTED_EDGE ( 'NONE', *, *, #118188, .F. ) ;
#43040 = VERTEX_POINT ( 'NONE', #27673 ) ;
#43041 = CARTESIAN_POINT ( 'NONE',  ( 11.44999999999990692, 12.50000000000000000, -6.841600689897078702 ) ) ;
#43042 = CARTESIAN_POINT ( 'NONE',  ( 8.749999999999918288, 12.50000000000000000, 7.188010851410848723 ) ) ;
#43043 = CIRCLE ( 'NONE', #76468, 0.06509327318403745899 ) ;
#43044 = CARTESIAN_POINT ( 'NONE',  ( -6.450000000000016165, 12.50000000000000000, 2.511473670974873507 ) ) ;
#43045 = EDGE_LOOP ( 'NONE', ( #9479, #59827, #89140, #60459 ) ) ;
#43046 = CARTESIAN_POINT ( 'NONE',  ( -12.09999999999999432, 2.500000000000000000, 3.637306695894644726 ) ) ;
#43047 = AXIS2_PLACEMENT_3D ( 'NONE', #15922, #46694, #86605 ) ;
#43048 = DIRECTION ( 'NONE',  ( 0.000000000000000000, 0.000000000000000000, 1.000000000000000000 ) ) ;
#43049 = AXIS2_PLACEMENT_3D ( 'NONE', #60386, #100916, #30276 ) ;
#43050 = DIRECTION ( 'NONE',  ( 0.000000000000000000, 0.000000000000000000, 1.000000000000000000 ) ) ;
#43051 = CARTESIAN_POINT ( 'NONE',  ( 186.2812500006828031, 0.000000000000000000, 7.700000000000000178 ) ) ;
#43052 = VERTEX_POINT ( 'NONE', #26416 ) ;
#43053 = EDGE_CURVE ( 'NONE', #69984, #84331, #128750, .T. ) ;
#43054 = DIRECTION ( 'NONE',  ( 0.000000000000000000, -0.000000000000000000, 1.000000000000000000 ) ) ;
#43055 = ADVANCED_FACE ( 'NONE', ( #36235 ), #104319, .T. ) ;
#43056 = ORIENTED_EDGE ( 'NONE', *, *, #128983, .T. ) ;
#43057 = CARTESIAN_POINT ( 'NONE',  ( 6.249999999999928946, 2.500000000000000000, 2.957883832488649389 ) ) ;
#43058 = AXIS2_PLACEMENT_3D ( 'NONE', #11068, #9153, #79825 ) ;
#43059 = ORIENTED_EDGE ( 'NONE', *, *, #72640, .T. ) ;
#43060 = AXIS2_PLACEMENT_3D ( 'NONE', #37702, #70868, #57336 ) ;
#43061 = ORIENTED_EDGE ( 'NONE', *, *, #125890, .T. ) ;
#43062 = FACE_OUTER_BOUND ( 'NONE', #114662, .T. ) ;
#43063 = DIRECTION ( 'NONE',  ( -0.000000000000000000, 1.000000000000000000, -0.000000000000000000 ) ) ;
#43064 = DIRECTION ( 'NONE',  ( -0.000000000000000000, -1.000000000000000000, -0.000000000000000000 ) ) ;
#43066 = ADVANCED_FACE ( 'NONE', ( #84676 ), #105732, .T. ) ;
#43065 = FACE_OUTER_BOUND ( 'NONE', #121088, .T. ) ;
#43067 = DIRECTION ( 'NONE',  ( 0.000000000000000000, 0.000000000000000000, 1.000000000000000000 ) ) ;
#43068 = VERTEX_POINT ( 'NONE', #6099 ) ;
#43069 = ORIENTED_EDGE ( 'NONE', *, *, #79145, .T. ) ;
#43070 = DIRECTION ( 'NONE',  ( 0.000000000000000000, 0.000000000000000000, -1.000000000000000000 ) ) ;
#43071 = VECTOR ( 'NONE', #6727, 1000.000000000000000 ) ;
#43072 = VECTOR ( 'NONE', #98225, 1000.000000000000000 ) ;
#43073 = PLANE ( 'NONE',  #32686 ) ;
#43074 = CARTESIAN_POINT ( 'NONE',  ( 10.84999999999991260, 12.50000000000000000, 5.867463478539781896 ) ) ;
#43075 = ORIENTED_EDGE ( 'NONE', *, *, #80019, .T. ) ;
#43076 = ORIENTED_EDGE ( 'NONE', *, *, #17277, .F. ) ;
#43077 = DIRECTION ( 'NONE',  ( 0.000000000000000000, 1.000000000000000000, 0.000000000000000000 ) ) ;
#43078 = VERTEX_POINT ( 'NONE', #55856 ) ;
#43079 = DIRECTION ( 'NONE',  ( 0.000000000000000000, 0.000000000000000000, -1.000000000000000000 ) ) ;
#43080 = FACE_OUTER_BOUND ( 'NONE', #31601, .T. ) ;
#43081 = FACE_OUTER_BOUND ( 'NONE', #101672, .T. ) ;
#43082 = ORIENTED_EDGE ( 'NONE', *, *, #48257, .T. ) ;
#43083 = CARTESIAN_POINT ( 'NONE',  ( -2.500000000000031086, 12.50000000000000000, 3.637306695894644726 ) ) ;
#43084 = CARTESIAN_POINT ( 'NONE',  ( 14.14999999999989200, 2.500000000000000000, -2.065063509461102065 ) ) ;
#43085 = DIRECTION ( 'NONE',  ( -0.000000000000000000, 1.000000000000000000, -0.000000000000000000 ) ) ;
#43086 = DIRECTION ( 'NONE',  ( -0.000000000000000000, -1.000000000000000000, -0.000000000000000000 ) ) ;
#43087 = CARTESIAN_POINT ( 'NONE',  ( 7.299999999999926104, 12.50000000000000000, -4.048810130592463530 ) ) ;
#43088 = ORIENTED_EDGE ( 'NONE', *, *, #66979, .T. ) ;
#43089 = ADVANCED_FACE ( 'NONE', ( #65011, #16559 ), #86602, .T. ) ;
#43090 = FACE_OUTER_BOUND ( 'NONE', #91574, .T. ) ;
#43091 = AXIS2_PLACEMENT_3D ( 'NONE', #9922, #99604, #37467 ) ;
#43092 = CARTESIAN_POINT ( 'NONE',  ( 26.61818291006423109, -2.722754637273441691, 4.358315985292433581 ) ) ;
#43093 = ORIENTED_EDGE ( 'NONE', *, *, #65788, .T. ) ;
#43094 = EDGE_LOOP ( 'NONE', ( #87186, #27036 ) ) ;
#43095 = EDGE_CURVE ( 'NONE', #87886, #70557, #66018, .T. ) ;
#43096 = CARTESIAN_POINT ( 'NONE',  ( 184.3593750003413732, 0.000000000000000000, 7.564683531250000925 ) ) ;
#43097 = DIRECTION ( 'NONE',  ( 0.000000000000000000, 0.000000000000000000, 1.000000000000000000 ) ) ;
#43098 = CARTESIAN_POINT ( 'NONE',  ( -3.100000000000028511, 2.500000000000000000, 0.4464101615137736623 ) ) ;
#43099 = EDGE_CURVE ( 'NONE', #45964, #68456, #55562, .T. ) ;
#43100 = CARTESIAN_POINT ( 'NONE',  ( -9.150000000000009237, 2.500000000000000000, -2.957883832488653830 ) ) ;
#43101 = DIRECTION ( 'NONE',  ( 0.000000000000000000, 0.000000000000000000, -1.000000000000000000 ) ) ;
#43102 = LINE ( 'NONE', #83648, #34581 ) ;
#43103 = CARTESIAN_POINT ( 'NONE',  ( -2.950000000000029932, 2.500000000000000000, 2.165063509461097713 ) ) ;
#43104 = CARTESIAN_POINT ( 'NONE',  ( -9.150000000000009237, 2.500000000000000000, -6.495190528383297135 ) ) ;
#43105 = CARTESIAN_POINT ( 'NONE',  ( -11.64999999999999858, 2.500000000000000000, -5.902370205355746968 ) ) ;
#43106 = EDGE_CURVE ( 'NONE', #90933, #77506, #74865, .T. ) ;
#43107 = EDGE_CURVE ( 'NONE', #39770, #122938, #22135, .T. ) ;
#43108 = EDGE_CURVE ( 'NONE', #45836, #67411, #25108, .T. ) ;
#43109 = CARTESIAN_POINT ( 'NONE',  ( -2.500000000000032419, 2.500000000000000000, -3.537306695894649966 ) ) ;
#43110 = ORIENTED_EDGE ( 'NONE', *, *, #81357, .F. ) ;
#43111 = VERTEX_POINT ( 'NONE', #126546 ) ;
#43112 = CIRCLE ( 'NONE', #84835, 0.06509327318403745899 ) ;
#43113 = EDGE_CURVE ( 'NONE', #124524, #67119, #95272, .T. ) ;
#43114 = EDGE_LOOP ( 'NONE', ( #111223, #14874 ) ) ;
#43115 = CIRCLE ( 'NONE', #55604, 0.06509327318403745899 ) ;
#43116 = EDGE_LOOP ( 'NONE', ( #2976, #45642 ) ) ;
#43117 = CARTESIAN_POINT ( 'NONE',  ( -10.45000000000000107, 12.50000000000000000, 2.230156782645134950 ) ) ;
#43118 = CARTESIAN_POINT ( 'NONE',  ( 5.649999999999934630, 12.50000000000000000, -2.511473670974877948 ) ) ;
#43119 = EDGE_CURVE ( 'NONE', #30275, #24551, #56495, .T. ) ;
#43120 = ORIENTED_EDGE ( 'NONE', *, *, #968, .T. ) ;
#43121 = DIRECTION ( 'NONE',  ( 0.000000000000000000, 0.000000000000000000, -1.000000000000000000 ) ) ;
#43122 = LINE ( 'NONE', #83035, #13538 ) ;
#43124 = VERTEX_POINT ( 'NONE', #27052 ) ;
#43123 = CARTESIAN_POINT ( 'NONE',  ( -3.100000000000028511, 12.50000000000000000, 0.3464101615137736845 ) ) ;
#43125 = FACE_OUTER_BOUND ( 'NONE', #115369, .T. ) ;
#43126 = DIRECTION ( 'NONE',  ( -0.000000000000000000, -1.000000000000000000, -0.000000000000000000 ) ) ;
#43127 = VERTEX_POINT ( 'NONE', #106879 ) ;
#43128 = AXIS2_PLACEMENT_3D ( 'NONE', #47749, #27437, #108591 ) ;
#43129 = ORIENTED_EDGE ( 'NONE', *, *, #76014, .T. ) ;
#43130 = EDGE_LOOP ( 'NONE', ( #16569, #113783 ) ) ;
#43131 = EDGE_LOOP ( 'NONE', ( #13304, #80860, #117388, #125603 ) ) ;
#43132 = CARTESIAN_POINT ( 'NONE',  ( 1.249999999999952482, 12.50000000000000000, -5.802370205355749988 ) ) ;
#43133 = AXIS2_PLACEMENT_3D ( 'NONE', #107245, #126248, #47051 ) ;
#43134 = LINE ( 'NONE', #92865, #25830 ) ;
#43135 = DIRECTION ( 'NONE',  ( 0.000000000000000000, 0.000000000000000000, 1.000000000000000000 ) ) ;
#43136 = AXIS2_PLACEMENT_3D ( 'NONE', #79385, #47346, #87245 ) ;
#43137 = CARTESIAN_POINT ( 'NONE',  ( -4.350000000000023626, 2.500000000000000000, -2.411473670974877859 ) ) ;
#43138 = ORIENTED_EDGE ( 'NONE', *, *, #95561, .F. ) ;
#43139 = AXIS2_PLACEMENT_3D ( 'NONE', #28829, #99503, #79843 ) ;
#43140 = DIRECTION ( 'NONE',  ( 0.000000000000000000, 1.000000000000000000, 0.000000000000000000 ) ) ;
#43141 = VERTEX_POINT ( 'NONE', #15264 ) ;
#43142 = PLANE ( 'NONE',  #18293 ) ;
#43143 = CARTESIAN_POINT ( 'NONE',  ( 7.173569985889933776, -2.500000000000000000, -8.713264184204838614 ) ) ;
#43144 = PLANE ( 'NONE',  #60933 ) ;
#43145 = DIRECTION ( 'NONE',  ( -0.000000000000000000, -1.000000000000000000, -0.000000000000000000 ) ) ;
#43146 = AXIS2_PLACEMENT_3D ( 'NONE', #104614, #76460, #126198 ) ;
#43147 = VERTEX_POINT ( 'NONE', #45412 ) ;
#43148 = EDGE_CURVE ( 'NONE', #112146, #45854, #7390, .T. ) ;
#43150 = AXIS2_PLACEMENT_3D ( 'NONE', #5332, #47208, #24983 ) ;
#43149 = VECTOR ( 'NONE', #69926, 1000.000000000000000 ) ;
#43151 = ORIENTED_EDGE ( 'NONE', *, *, #29533, .T. ) ;
#43152 = ORIENTED_EDGE ( 'NONE', *, *, #118049, .T. ) ;
#43153 = DIRECTION ( 'NONE',  ( -0.000000000000000000, -1.000000000000000000, -0.000000000000000000 ) ) ;
#43154 = CARTESIAN_POINT ( 'NONE',  ( -3.642919299551294898E-14, 2.500000000000000000, 0.6928203230275518099 ) ) ;
#43155 = DIRECTION ( 'NONE',  ( -0.000000000000000000, 1.000000000000000000, -0.000000000000000000 ) ) ;
#43156 = FACE_BOUND ( 'NONE', #85104, .T. ) ;
#43157 = CARTESIAN_POINT ( 'NONE',  ( -5.800000000000018474, 2.500000000000000000, 4.330127018922196314 ) ) ;
#43158 = DIRECTION ( 'NONE',  ( 0.000000000000000000, 0.000000000000000000, -1.000000000000000000 ) ) ;
#43159 = CARTESIAN_POINT ( 'NONE',  ( 7.499999999999927169, 12.50000000000000000, -5.022947341949754119 ) ) ;
#43160 = EDGE_CURVE ( 'NONE', #88434, #58364, #59795, .T. ) ;
#43161 = CARTESIAN_POINT ( 'NONE',  ( 9.399999999999918643, 12.50000000000000000, 0.3464101615137736845 ) ) ;
#43162 = CARTESIAN_POINT ( 'NONE',  ( 184.2083333333333144, -4.445597072760187451, -7.699999999999876721 ) ) ;
#43163 = CARTESIAN_POINT ( 'NONE',  ( 1.899999999999949507, 2.500000000000000000, 4.083716857408421497 ) ) ;
#43164 = ORIENTED_EDGE ( 'NONE', *, *, #108351, .T. ) ;
#43165 = CARTESIAN_POINT ( 'NONE',  ( -6.900000000000015454, 12.50000000000000000, 4.048810130592458201 ) ) ;
#43166 = ORIENTED_EDGE ( 'NONE', *, *, #9284, .T. ) ;
#43167 = VERTEX_POINT ( 'NONE', #108813 ) ;
#43168 = CARTESIAN_POINT ( 'NONE',  ( -0.4000000000000396572, 12.50000000000000000, 3.572213422710607489 ) ) ;
#43169 = DIRECTION ( 'NONE',  ( 0.000000000000000000, 0.000000000000000000, -1.000000000000000000 ) ) ;
#43170 = FACE_BOUND ( 'NONE', #29278, .T. ) ;
#43171 = CARTESIAN_POINT ( 'NONE',  ( -11.64999999999999680, 2.500000000000000000, -7.188010851410850499 ) ) ;
#43172 = CIRCLE ( 'NONE', #30563, 0.1000000000000002554 ) ;
#43173 = AXIS2_PLACEMENT_3D ( 'NONE', #26834, #58872, #58242 ) ;
#43174 = EDGE_LOOP ( 'NONE', ( #29167, #60920, #46364, #119367 ) ) ;
#43175 = CARTESIAN_POINT ( 'NONE',  ( 87.49999999944498086, 3.974992050012154277, 6.359987280019447020 ) ) ;
#43176 = FACE_OUTER_BOUND ( 'NONE', #118483, .T. ) ;
#43177 = ORIENTED_EDGE ( 'NONE', *, *, #109226, .T. ) ;
#43178 = CARTESIAN_POINT ( 'NONE',  ( -2.700000000000031264, 12.50000000000000000, 4.676537180435972552 ) ) ;
#43179 = DIRECTION ( 'NONE',  ( 0.000000000000000000, 1.000000000000000000, 0.000000000000000000 ) ) ;
#43181 = VECTOR ( 'NONE', #74376, 1000.000000000000000 ) ;
#43180 = CONICAL_SURFACE ( 'NONE', #61947, 0.1000000000000002554, 0.003490658503988666988 ) ;
#43182 = ADVANCED_FACE ( 'NONE', ( #109475 ), #38835, .T. ) ;
#43183 = EDGE_LOOP ( 'NONE', ( #110829, #26599 ) ) ;
#43184 = FACE_OUTER_BOUND ( 'NONE', #35819, .T. ) ;
#43185 = DIRECTION ( 'NONE',  ( 0.000000000000000000, 0.000000000000000000, 1.000000000000000000 ) ) ;
#43187 = AXIS2_PLACEMENT_3D ( 'NONE', #13165, #60381, #93047 ) ;
#43186 = AXIS2_PLACEMENT_3D ( 'NONE', #64813, #11841, #51785 ) ;
#43188 = ADVANCED_FACE ( 'NONE', ( #17862 ), #19132, .T. ) ;
#43189 = ORIENTED_EDGE ( 'NONE', *, *, #29137, .T. ) ;
#43190 = AXIS2_PLACEMENT_3D ( 'NONE', #74598, #4532, #52380 ) ;
#43191 = DIRECTION ( 'NONE',  ( 0.000000000000000000, 0.000000000000000000, 1.000000000000000000 ) ) ;
#43192 = DIRECTION ( 'NONE',  ( -0.000000000000000000, -1.000000000000000000, -0.000000000000000000 ) ) ;
#43193 = CARTESIAN_POINT ( 'NONE',  ( 10.19999999999991225, 12.50000000000000000, -4.676537180435978769 ) ) ;
#43194 = ORIENTED_EDGE ( 'NONE', *, *, #96816, .T. ) ;
#43195 = EDGE_CURVE ( 'NONE', #47459, #20502, #26325, .T. ) ;
#43196 = ORIENTED_EDGE ( 'NONE', *, *, #23726, .T. ) ;
#43197 = EDGE_CURVE ( 'NONE', #95641, #52044, #74335, .T. ) ;
#43198 = EDGE_LOOP ( 'NONE', ( #103740, #65622 ) ) ;
#43199 = DIRECTION ( 'NONE',  ( 0.000000000000000000, 0.000000000000000000, 1.000000000000000000 ) ) ;
#43200 = DIRECTION ( 'NONE',  ( 0.000000000000000000, 0.000000000000000000, 1.000000000000000000 ) ) ;
#43201 = EDGE_LOOP ( 'NONE', ( #16623, #61145 ) ) ;
#43202 = EDGE_CURVE ( 'NONE', #3469, #100762, #116181, .T. ) ;
#43203 = CARTESIAN_POINT ( 'NONE',  ( 12.69999999999990337, 12.50000000000000000, 3.983716857408420076 ) ) ;
#43204 = CARTESIAN_POINT ( 'NONE',  ( -14.14999999999998614, 12.50000000000000000, 1.537336459617586915 ) ) ;
#43205 = DIRECTION ( 'NONE',  ( 0.000000000000000000, 0.000000000000000000, 1.000000000000000000 ) ) ;
#43206 = CARTESIAN_POINT ( 'NONE',  ( -4.150000000000028777, 2.500000000000000000, -5.902370205355750521 ) ) ;
#43207 = EDGE_CURVE ( 'NONE', #127992, #110877, #101534, .T. ) ;
#43208 = CONICAL_SURFACE ( 'NONE', #78708, 0.09999999999999982514, 0.003490658503988666988 ) ;
#43209 = DIRECTION ( 'NONE',  ( -0.000000000000000000, 1.000000000000000000, -0.000000000000000000 ) ) ;
#43210 = AXIS2_PLACEMENT_3D ( 'NONE', #116098, #44138, #116732 ) ;
#43211 = VERTEX_POINT ( 'NONE', #40760 ) ;
#43212 = VERTEX_POINT ( 'NONE', #88534 ) ;
#43213 = DIRECTION ( 'NONE',  ( -0.000000000000000000, 1.000000000000000000, -0.000000000000000000 ) ) ;
#43214 = VERTEX_POINT ( 'NONE', #68251 ) ;
#43215 = VECTOR ( 'NONE', #94622, 1000.000000000000000 ) ;
#43216 = CARTESIAN_POINT ( 'NONE',  ( 105.4682043743740110, 6.375218138983957061, -4.323317965031781007 ) ) ;
#43218 = EDGE_LOOP ( 'NONE', ( #126246, #34996 ) ) ;
#43217 = ORIENTED_EDGE ( 'NONE', *, *, #26220, .F. ) ;
#43219 = VERTEX_POINT ( 'NONE', #78750 ) ;
#43220 = CARTESIAN_POINT ( 'NONE',  ( 1.049999999999954525, 12.50000000000000000, 1.818653347947321475 ) ) ;
#43221 = VECTOR ( 'NONE', #118337, 1000.000000000000000 ) ;
#43222 = CARTESIAN_POINT ( 'NONE',  ( 5.849999999999933031, 2.500000000000000000, 7.288010851410849256 ) ) ;
#43223 = DIRECTION ( 'NONE',  ( 0.000000000000000000, 0.000000000000000000, 1.000000000000000000 ) ) ;
#43224 = CONICAL_SURFACE ( 'NONE', #53585, 0.1000000000000000056, 0.003490658503988666988 ) ;
#43225 =( NAMED_UNIT ( * ) PLANE_ANGLE_UNIT ( ) SI_UNIT ( $, .RADIAN. ) );
#43226 = DIRECTION ( 'NONE',  ( 0.000000000000000000, -0.000000000000000000, 1.000000000000000000 ) ) ;
#43227 = EDGE_CURVE ( 'NONE', #61297, #61474, #80670, .T. ) ;
#43228 = DIRECTION ( 'NONE',  ( 0.000000000000000000, 0.000000000000000000, 1.000000000000000000 ) ) ;
#43229 = CARTESIAN_POINT ( 'NONE',  ( -8.350000000000013856, 2.500000000000000000, -6.595190528383296780 ) ) ;
#43230 = CARTESIAN_POINT ( 'NONE',  ( -12.04999999999999716, 2.500000000000000000, -6.595190528383298556 ) ) ;
#43231 = DIRECTION ( 'NONE',  ( 0.000000000000000000, 0.000000000000000000, 1.000000000000000000 ) ) ;
#43232 = AXIS2_PLACEMENT_3D ( 'NONE', #101476, #11791, #62207 ) ;
#43233 = CARTESIAN_POINT ( 'NONE',  ( 7.899999999999921307, 2.500000000000000000, -2.385244779468109755E-15 ) ) ;
#43234 = AXIS2_PLACEMENT_3D ( 'NONE', #86587, #117309, #18498 ) ;
#43235 = ORIENTED_EDGE ( 'NONE', *, *, #121234, .T. ) ;
#43236 = ADVANCED_FACE ( 'NONE', ( #80012 ), #19966, .T. ) ;
#43237 = VECTOR ( 'NONE', #69116, 1000.000000000000000 ) ;
#43238 = DIRECTION ( 'NONE',  ( -0.000000000000000000, 1.000000000000000000, -0.000000000000000000 ) ) ;
#43239 = ORIENTED_EDGE ( 'NONE', *, *, #73950, .T. ) ;
#43240 = ORIENTED_EDGE ( 'NONE', *, *, #65832, .T. ) ;
#43241 = CARTESIAN_POINT ( 'NONE',  ( 11.84999999999990727, 12.50000000000000000, -2.511473670974877948 ) ) ;
#43242 = CARTESIAN_POINT ( 'NONE',  ( 5.849999999999933920, 12.50000000000000000, 6.495190528383297135 ) ) ;
#43243 = DIRECTION ( 'NONE',  ( -0.000000000000000000, -1.000000000000000000, -0.000000000000000000 ) ) ;
#43244 = EDGE_CURVE ( 'NONE', #35406, #81765, #5376, .T. ) ;
#43245 = DIRECTION ( 'NONE',  ( 0.000000000000000000, 0.000000000000000000, 1.000000000000000000 ) ) ;
#43246 = DIRECTION ( 'NONE',  ( 0.000000000000000000, 0.000000000000000000, 1.000000000000000000 ) ) ;
#43247 = DIRECTION ( 'NONE',  ( 0.000000000000000000, 0.000000000000000000, 1.000000000000000000 ) ) ;
#43248 = DIRECTION ( 'NONE',  ( 0.000000000000000000, -0.9999939076577903929, 0.003490651415223739937 ) ) ;
#43249 = EDGE_LOOP ( 'NONE', ( #127345, #95620 ) ) ;
#43250 = EDGE_CURVE ( 'NONE', #94263, #86875, #65074, .T. ) ;
#43251 = ADVANCED_FACE ( 'NONE', ( #23031 ), #102856, .T. ) ;
#43252 = EDGE_CURVE ( 'NONE', #67756, #94856, #26897, .T. ) ;
#43253 = DIRECTION ( 'NONE',  ( 0.000000000000000000, 0.000000000000000000, -1.000000000000000000 ) ) ;
#43254 = ORIENTED_EDGE ( 'NONE', *, *, #42955, .T. ) ;
#43255 = EDGE_LOOP ( 'NONE', ( #12538, #66709 ) ) ;
#43256 = ADVANCED_FACE ( 'NONE', ( #96913 ), #101347, .T. ) ;
#43257 = EDGE_LOOP ( 'NONE', ( #62934, #70235 ) ) ;
#43258 = EDGE_LOOP ( 'NONE', ( #110164, #26468 ) ) ;
#43259 = CARTESIAN_POINT ( 'NONE',  ( -2.500000000000030642, 12.50000000000000000, -0.6928203230275541413 ) ) ;
#43260 = DIRECTION ( 'NONE',  ( -0.000000000000000000, -1.000000000000000000, -0.000000000000000000 ) ) ;
#43261 = EDGE_CURVE ( 'NONE', #41869, #9888, #44908, .T. ) ;
#43262 = EDGE_CURVE ( 'NONE', #63955, #110791, #99199, .T. ) ;
#43263 = CIRCLE ( 'NONE', #9787, 0.06509327318403745899 ) ;
#43264 = DIRECTION ( 'NONE',  ( 0.000000000000000000, 0.000000000000000000, 1.000000000000000000 ) ) ;
#43266 = DIRECTION ( 'NONE',  ( 0.000000000000000000, 1.000000000000000000, 0.000000000000000000 ) ) ;
#43265 = AXIS2_PLACEMENT_3D ( 'NONE', #11696, #32004, #81719 ) ;
#43267 = CARTESIAN_POINT ( 'NONE',  ( -5.000000000000023093, 2.500000000000000000, 0.5928203230275495006 ) ) ;
#43268 = VERTEX_POINT ( 'NONE', #34144 ) ;
#43269 = DIRECTION ( 'NONE',  ( 0.000000000000000000, 0.000000000000000000, 1.000000000000000000 ) ) ;
#43270 = CARTESIAN_POINT ( 'NONE',  ( -9.600000000000008527, 2.500000000000000000, -2.385244779468109755E-15 ) ) ;
#43271 = DIRECTION ( 'NONE',  ( -0.000000000000000000, -1.000000000000000000, -0.000000000000000000 ) ) ;
#43273 = AXIS2_PLACEMENT_3D ( 'NONE', #80013, #20457, #18514 ) ;
#43272 = VECTOR ( 'NONE', #83201, 1000.000000000000000 ) ;
#43274 = DIRECTION ( 'NONE',  ( 0.000000000000000000, 0.000000000000000000, 1.000000000000000000 ) ) ;
#43275 = ORIENTED_EDGE ( 'NONE', *, *, #32851, .F. ) ;
#43276 = EDGE_LOOP ( 'NONE', ( #122923, #124794, #18653, #27640 ) ) ;
#43277 = ORIENTED_EDGE ( 'NONE', *, *, #22672, .T. ) ;
#43278 = DIRECTION ( 'NONE',  ( 0.000000000000000000, 0.000000000000000000, -1.000000000000000000 ) ) ;
#43279 = AXIS2_PLACEMENT_3D ( 'NONE', #69152, #35371, #118260 ) ;
#43280 = LINE ( 'NONE', #33458, #17412 ) ;
#43281 = CARTESIAN_POINT ( 'NONE',  ( -12.89999999999999147, 2.500000000000000000, -0.7928203230275501223 ) ) ;
#43282 = AXIS2_PLACEMENT_3D ( 'NONE', #84033, #123962, #85959 ) ;
#43283 = ORIENTED_EDGE ( 'NONE', *, *, #54776, .T. ) ;
#43284 = DIRECTION ( 'NONE',  ( -4.274815082592931898E-19, -0.9999939076577903929, -0.003490651415223739937 ) ) ;
#43285 = LINE ( 'NONE', #14429, #85052 ) ;
#43286 = DIRECTION ( 'NONE',  ( 0.000000000000000000, 0.000000000000000000, 1.000000000000000000 ) ) ;
#43287 = DIRECTION ( 'NONE',  ( 0.000000000000000000, -0.000000000000000000, 1.000000000000000000 ) ) ;
#43288 = DIRECTION ( 'NONE',  ( 0.000000000000000000, 1.000000000000000000, 0.000000000000000000 ) ) ;
#43289 = EDGE_CURVE ( 'NONE', #89858, #23588, #19774, .T. ) ;
#43290 = VERTEX_POINT ( 'NONE', #56342 ) ;
#43291 = ORIENTED_EDGE ( 'NONE', *, *, #110819, .F. ) ;
#43292 = LINE ( 'NONE', #14438, #45977 ) ;
#43293 = AXIS2_PLACEMENT_3D ( 'NONE', #43689, #32583, #83598 ) ;
#43294 = CARTESIAN_POINT ( 'NONE',  ( 11.24999999999990941, 2.500000000000000000, -1.372243186433550033 ) ) ;
#43295 = CIRCLE ( 'NONE', #116423, 0.1000000000000002554 ) ;
#43296 = CARTESIAN_POINT ( 'NONE',  ( -5.000000000000022204, 12.50000000000000000, 3.702399969078682407 ) ) ;
#43297 = DIRECTION ( 'NONE',  ( 1.000000000000000000, 0.000000000000000000, 0.000000000000000000 ) ) ;
#43298 = DIRECTION ( 'NONE',  ( 0.000000000000000000, 0.000000000000000000, 1.000000000000000000 ) ) ;
#43299 = EDGE_CURVE ( 'NONE', #58093, #7017, #65521, .T. ) ;
#43300 = ORIENTED_EDGE ( 'NONE', *, *, #69291, .F. ) ;
#43301 = AXIS2_PLACEMENT_3D ( 'NONE', #122652, #91906, #33002 ) ;
#43302 = ORIENTED_EDGE ( 'NONE', *, *, #24708, .T. ) ;
#43303 = DIRECTION ( 'NONE',  ( 0.000000000000000000, -0.9999939076577903929, 0.003490651415223739937 ) ) ;
#43304 = CARTESIAN_POINT ( 'NONE',  ( 9.999999999999912959, 2.500000000000000000, -4.922947341949753586 ) ) ;
#43306 = CARTESIAN_POINT ( 'NONE',  ( 16.88398418148221225, -2.500000000000000000, -4.430584152985939106 ) ) ;
#43305 = AXIS2_PLACEMENT_3D ( 'NONE', #4990, #15456, #92754 ) ;
#43307 = DIRECTION ( 'NONE',  ( 0.000000000000000000, -0.9999939076577903929, 0.003490651415223739937 ) ) ;
#43308 = DIRECTION ( 'NONE',  ( 0.000000000000000000, 0.000000000000000000, -1.000000000000000000 ) ) ;
#43309 = ORIENTED_EDGE ( 'NONE', *, *, #38796, .F. ) ;
#43310 = FACE_OUTER_BOUND ( 'NONE', #105539, .T. ) ;
#43311 = CIRCLE ( 'NONE', #37040, 0.06509327318403745899 ) ;
#43312 = CARTESIAN_POINT ( 'NONE',  ( 4.349999999999941025, 2.500000000000000000, -1.718653347947326049 ) ) ;
#43313 = EDGE_LOOP ( 'NONE', ( #50105, #77126, #67865, #35272 ) ) ;
#43314 = CARTESIAN_POINT ( 'NONE',  ( 10.64999999999991331, 2.500000000000000000, 6.741600689897071952 ) ) ;
#43315 = ORIENTED_EDGE ( 'NONE', *, *, #6656, .T. ) ;
#43317 = AXIS2_PLACEMENT_3D ( 'NONE', #51198, #42011, #71455 ) ;
#43316 = CARTESIAN_POINT ( 'NONE',  ( 2.499999999999981792, 12.50000000000000000, 4.330127018922196314 ) ) ;
#43318 = AXIS2_PLACEMENT_3D ( 'NONE', #90823, #31277, #111081 ) ;
#43319 = ORIENTED_EDGE ( 'NONE', *, *, #49612, .F. ) ;
#43320 = DIRECTION ( 'NONE',  ( 0.000000000000000000, -0.000000000000000000, 1.000000000000000000 ) ) ;
#43321 = CARTESIAN_POINT ( 'NONE',  ( -8.950000000000011724, 2.500000000000000000, -6.148780366869520897 ) ) ;
#43322 = ORIENTED_EDGE ( 'NONE', *, *, #6872, .T. ) ;
#43323 =( BOUNDED_CURVE ( )  B_SPLINE_CURVE ( 2, ( #129532, #9730, #40503, #60765, #120331, #25329, #44332 ),
 .UNSPECIFIED., .F., .F. ) 
 B_SPLINE_CURVE_WITH_KNOTS ( ( 3, 2, 2, 3 ),
 ( 0.5000000000000004441, 0.5238095238095242800, 0.5476190476190482270, 0.5714285714285719520 ),
 .UNSPECIFIED. ) 
 CURVE ( )  GEOMETRIC_REPRESENTATION_ITEM ( )  RATIONAL_B_SPLINE_CURVE ( ( 0.9999999999999974465, 0.8660254037844412611, 1.000000000000000000, 0.8660254037844387076, 1.000000000000000000, 0.8660254037844355990, 1.000000000000003109 ) ) 
 REPRESENTATION_ITEM ( '' )  );
#43324 = ORIENTED_EDGE ( 'NONE', *, *, #107947, .T. ) ;
#43325 = CARTESIAN_POINT ( 'NONE',  ( 184.7135416670080872, 4.367472073101518859, -7.564683531249999149 ) ) ;
#43326 = DIRECTION ( 'NONE',  ( 0.000000000000000000, -0.9999939076577903929, 0.003490651415223739937 ) ) ;
#43327 = CARTESIAN_POINT ( 'NONE',  ( 186.3802083336747444, 4.367472073101515306, 7.564683531250000925 ) ) ;
#43328 = CARTESIAN_POINT ( 'NONE',  ( 186.0677083336747444, -4.367472073101514418, -7.564683531250002702 ) ) ;
#43329 = CARTESIAN_POINT ( 'NONE',  ( 2.299999999999949640, 12.50000000000000000, -0.3464101615137782364 ) ) ;
#43330 = CARTESIAN_POINT ( 'NONE',  ( -2.499999999999996447, 2.500000000000000000, 4.330127018922196314 ) ) ;
#43331 = DIRECTION ( 'NONE',  ( 0.000000000000000000, -0.000000000000000000, 1.000000000000000000 ) ) ;
#43332 = DIRECTION ( 'NONE',  ( -0.000000000000000000, 1.000000000000000000, -0.000000000000000000 ) ) ;
#43333 = CONICAL_SURFACE ( 'NONE', #83045, 0.09999999999999982514, 0.003490658503988666988 ) ;
#43334 = EDGE_CURVE ( 'NONE', #13172, #54302, #86944, .T. ) ;
#43335 = ORIENTED_EDGE ( 'NONE', *, *, #21180, .F. ) ;
#43336 = EDGE_LOOP ( 'NONE', ( #87214, #35800, #74130, #46809 ) ) ;
#43337 = DIRECTION ( 'NONE',  ( 0.000000000000000000, 0.000000000000000000, -1.000000000000000000 ) ) ;
#43338 = ORIENTED_EDGE ( 'NONE', *, *, #71830, .F. ) ;
#43339 = DIRECTION ( 'NONE',  ( 0.000000000000000000, 0.000000000000000000, -1.000000000000000000 ) ) ;
#43340 = DIRECTION ( 'NONE',  ( -0.000000000000000000, 1.000000000000000000, -0.000000000000000000 ) ) ;
#43341 = CARTESIAN_POINT ( 'NONE',  ( 12.89999999999990266, 2.500000000000000000, -3.537306695894649966 ) ) ;
#43343 = VERTEX_POINT ( 'NONE', #124451 ) ;
#43342 = VERTEX_POINT ( 'NONE', #95636 ) ;
#43344 = ADVANCED_FACE ( 'NONE', ( #5943 ), #103687, .T. ) ;
#43345 = FACE_BOUND ( 'NONE', #76191, .T. ) ;
#43346 = ORIENTED_EDGE ( 'NONE', *, *, #37422, .F. ) ;
#43347 = EDGE_CURVE ( 'NONE', #109625, #73015, #53514, .T. ) ;
#43348 = CARTESIAN_POINT ( 'NONE',  ( -10.40000000000000213, 12.50000000000000000, -0.6928203230275541413 ) ) ;
#43349 = DIRECTION ( 'NONE',  ( 0.000000000000000000, 0.000000000000000000, -1.000000000000000000 ) ) ;
#43350 = DIRECTION ( 'NONE',  ( 0.000000000000000000, 0.000000000000000000, 1.000000000000000000 ) ) ;
#43351 = FACE_OUTER_BOUND ( 'NONE', #8212, .T. ) ;
#43352 = AXIS2_PLACEMENT_3D ( 'NONE', #60745, #88917, #49006 ) ;
#43353 = FACE_OUTER_BOUND ( 'NONE', #18948, .T. ) ;
#43354 = AXIS2_PLACEMENT_3D ( 'NONE', #120695, #93818, #21202 ) ;
#43355 = CARTESIAN_POINT ( 'NONE',  ( -3.300000000000028244, 2.500000000000000000, 4.330127018922196314 ) ) ;
#43356 = ADVANCED_FACE ( 'NONE', ( #55066 ), #61636, .T. ) ;
#43357 = DIRECTION ( 'NONE',  ( -0.000000000000000000, 1.000000000000000000, -0.000000000000000000 ) ) ;
#43358 = ADVANCED_FACE ( 'NONE', ( #116554 ), #74153, .T. ) ;
#43359 = LINE ( 'NONE', #34835, #48459 ) ;
#43360 = FACE_OUTER_BOUND ( 'NONE', #99751, .T. ) ;
#43361 = CARTESIAN_POINT ( 'NONE',  ( 187.5000000000000000, 9.429780353434619030E-16, -7.700000000000000178 ) ) ;
#43362 = EDGE_CURVE ( 'NONE', #23039, #59349, #30544, .T. ) ;
#43363 = CARTESIAN_POINT ( 'NONE',  ( -10.45000000000000107, 12.50000000000000000, 6.495190528383297135 ) ) ;
#43365 = VECTOR ( 'NONE', #119081, 1000.000000000000000 ) ;
#43364 = AXIS2_PLACEMENT_3D ( 'NONE', #39122, #79655, #79031 ) ;
#43366 = EDGE_LOOP ( 'NONE', ( #93382, #65262 ) ) ;
#43367 = ORIENTED_EDGE ( 'NONE', *, *, #73653, .T. ) ;
#43368 = VECTOR ( 'NONE', #55752, 1000.000000000000000 ) ;
#43369 = ORIENTED_EDGE ( 'NONE', *, *, #6045, .F. ) ;
#43370 = FACE_OUTER_BOUND ( 'NONE', #4273, .T. ) ;
#43371 = EDGE_LOOP ( 'NONE', ( #32431, #124883 ) ) ;
#43372 = DIRECTION ( 'NONE',  ( 0.000000000000000000, 0.000000000000000000, -1.000000000000000000 ) ) ;
#43374 = ORIENTED_EDGE ( 'NONE', *, *, #67889, .T. ) ;
#43373 = ORIENTED_EDGE ( 'NONE', *, *, #18810, .F. ) ;
#43375 = ORIENTED_EDGE ( 'NONE', *, *, #52310, .T. ) ;
#43376 = CARTESIAN_POINT ( 'NONE',  ( -8.150000000000012790, 2.500000000000000000, -1.818653347947326138 ) ) ;
#43378 = AXIS2_PLACEMENT_3D ( 'NONE', #84353, #93531, #54882 ) ;
#43377 = AXIS2_PLACEMENT_3D ( 'NONE', #46146, #86054, #93964 ) ;
#43379 = VECTOR ( 'NONE', #121240, 1000.000000000000000 ) ;
#43380 = LINE ( 'NONE', #101643, #17464 ) ;
#43381 = FACE_OUTER_BOUND ( 'NONE', #5634, .T. ) ;
#43382 = CARTESIAN_POINT ( 'NONE',  ( -6.249999999999981348, 2.500000000000000000, 2.165063509461097713 ) ) ;
#43383 = CARTESIAN_POINT ( 'NONE',  ( 11.04999999999990834, 2.500000000000000000, 1.818653347947321475 ) ) ;
#43384 = ORIENTED_EDGE ( 'NONE', *, *, #63860, .F. ) ;
#43385 = LINE ( 'NONE', #112114, #83236 ) ;
#43386 = ORIENTED_EDGE ( 'NONE', *, *, #95510, .F. ) ;
#43387 = ORIENTED_EDGE ( 'NONE', *, *, #24810, .T. ) ;
#43388 = EDGE_LOOP ( 'NONE', ( #59807, #18497, #123211, #39543 ) ) ;
#43389 = AXIS2_PLACEMENT_3D ( 'NONE', #71184, #87117, #127061 ) ;
#43390 = DIRECTION ( 'NONE',  ( 0.000000000000000000, -0.000000000000000000, 1.000000000000000000 ) ) ;
#43391 = EDGE_LOOP ( 'NONE', ( #109918, #106920, #53638, #71156 ) ) ;
#43392 = ORIENTED_EDGE ( 'NONE', *, *, #124594, .F. ) ;
#43393 = EDGE_LOOP ( 'NONE', ( #73718, #15096, #55299, #25119 ) ) ;
#43394 = AXIS2_PLACEMENT_3D ( 'NONE', #17571, #77777, #28057 ) ;
#43395 = DIRECTION ( 'NONE',  ( 0.000000000000000000, 1.000000000000000000, 0.000000000000000000 ) ) ;
#43396 = CARTESIAN_POINT ( 'NONE',  ( -2.499999999999996447, 12.50000000000000000, 4.330127018922196314 ) ) ;
#43398 = CIRCLE ( 'NONE', #62173, 0.06509327318403745899 ) ;
#43397 = DIRECTION ( 'NONE',  ( -0.000000000000000000, 1.000000000000000000, -0.000000000000000000 ) ) ;
#43399 = FACE_OUTER_BOUND ( 'NONE', #125435, .T. ) ;
#43400 = CARTESIAN_POINT ( 'NONE',  ( 4.349999999999941025, 2.500000000000000000, -6.148780366869526226 ) ) ;
#43401 = EDGE_CURVE ( 'NONE', #113534, #70253, #78367, .T. ) ;
#43402 = PLANE ( 'NONE',  #77935 ) ;
#43403 = EDGE_CURVE ( 'NONE', #20780, #112974, #13487, .T. ) ;
#43404 = AXIS2_PLACEMENT_3D ( 'NONE', #93246, #74892, #101774 ) ;
#43405 = ADVANCED_FACE ( 'NONE', ( #126387 ), #76643, .T. ) ;
#43407 = AXIS2_PLACEMENT_3D ( 'NONE', #40280, #48819, #99850 ) ;
#43406 = PLANE ( 'NONE',  #24107 ) ;
#43408 = ORIENTED_EDGE ( 'NONE', *, *, #74525, .T. ) ;
#43409 = AXIS2_PLACEMENT_3D ( 'NONE', #100381, #128580, #79462 ) ;
#43410 = AXIS2_PLACEMENT_3D ( 'NONE', #108623, #117134, #48419 ) ;
#43411 = DIRECTION ( 'NONE',  ( 0.000000000000000000, 0.000000000000000000, 1.000000000000000000 ) ) ;
#43412 = ORIENTED_EDGE ( 'NONE', *, *, #89334, .F. ) ;
#43413 = FACE_OUTER_BOUND ( 'NONE', #80768, .T. ) ;
#43415 = ORIENTED_EDGE ( 'NONE', *, *, #34003, .F. ) ;
#43414 = EDGE_CURVE ( 'NONE', #93998, #56130, #76215, .T. ) ;
#43416 = CONICAL_SURFACE ( 'NONE', #49676, 0.09999999999999999167, 0.003490658503988666988 ) ;
#43417 = ADVANCED_FACE ( 'NONE', ( #45250 ), #38665, .T. ) ;
#43418 = VERTEX_POINT ( 'NONE', #49780 ) ;
#43420 = ADVANCED_FACE ( 'NONE', ( #117175 ), #89683, .T. ) ;
#43419 = PLANE ( 'NONE',  #30234 ) ;
#43421 = CARTESIAN_POINT ( 'NONE',  ( 2.499999999999945377, 2.500000000000000000, 5.022947341949748790 ) ) ;
#43422 = EDGE_CURVE ( 'NONE', #781, #64023, #111814, .T. ) ;
#43425 = EDGE_CURVE ( 'NONE', #85131, #83089, #34450, .T. ) ;
#43424 = CIRCLE ( 'NONE', #10047, 0.06509327318403745899 ) ;
#43423 = CIRCLE ( 'NONE', #76854, 0.09999999999999982514 ) ;
#43426 = DIRECTION ( 'NONE',  ( 0.000000000000000000, -0.000000000000000000, 1.000000000000000000 ) ) ;
#43427 = VERTEX_POINT ( 'NONE', #127044 ) ;
#43428 = VERTEX_POINT ( 'NONE', #77917 ) ;
#43429 = CARTESIAN_POINT ( 'NONE',  ( -2.700000000000030820, 2.500000000000000000, 0.2464101615137735679 ) ) ;
#43430 = CARTESIAN_POINT ( 'NONE',  ( 12.29999999999990479, 2.500000000000000000, -3.983716857408426293 ) ) ;
#43431 = DIRECTION ( 'NONE',  ( 0.000000000000000000, 0.000000000000000000, 1.000000000000000000 ) ) ;
#43432 = DIRECTION ( 'NONE',  ( 0.000000000000000000, 1.000000000000000000, 0.000000000000000000 ) ) ;
#43433 = ADVANCED_FACE ( 'NONE', ( #37375 ), #51176, .T. ) ;
#43434 = DIRECTION ( 'NONE',  ( 0.000000000000000000, 1.000000000000000000, 0.000000000000000000 ) ) ;
#43435 = ORIENTED_EDGE ( 'NONE', *, *, #54088, .T. ) ;
#43436 = CARTESIAN_POINT ( 'NONE',  ( -4.600000000000028066, 2.500000000000000000, -4.922947341949753586 ) ) ;
#43437 = CIRCLE ( 'NONE', #80977, 0.1000000000000002554 ) ;
#43438 = ORIENTED_EDGE ( 'NONE', *, *, #40155, .T. ) ;
#43439 = FACE_OUTER_BOUND ( 'NONE', #28170, .T. ) ;
#43440 = CARTESIAN_POINT ( 'NONE',  ( 8.749999999999953815, 2.500000000000000000, -2.165063509461101710 ) ) ;
#43441 = CARTESIAN_POINT ( 'NONE',  ( 187.0000000000000000, 0.000000000000000000, 7.700000000000000178 ) ) ;
#43442 = LINE ( 'NONE', #64346, #5130 ) ;
#43443 = CARTESIAN_POINT ( 'NONE',  ( -11.64999999999999680, 12.50000000000000000, -2.230156782645135394 ) ) ;
#43444 = CARTESIAN_POINT ( 'NONE',  ( -7.700000000000016165, 2.500000000000000000, -3.983716857408426293 ) ) ;
#43445 = DIRECTION ( 'NONE',  ( 0.000000000000000000, 1.000000000000000000, 0.000000000000000000 ) ) ;
#43446 = ORIENTED_EDGE ( 'NONE', *, *, #123424, .T. ) ;
#43447 = VECTOR ( 'NONE', #93426, 1000.000000000000000 ) ;
#43448 = FACE_OUTER_BOUND ( 'NONE', #76335, .T. ) ;
#43449 = CIRCLE ( 'NONE', #64352, 0.06509327318403745899 ) ;
#43450 = FACE_OUTER_BOUND ( 'NONE', #72644, .T. ) ;
#43451 = LINE ( 'NONE', #44073, #89440 ) ;
#43452 = ORIENTED_EDGE ( 'NONE', *, *, #93055, .T. ) ;
#43453 = DIRECTION ( 'NONE',  ( 0.000000000000000000, 1.000000000000000000, 0.000000000000000000 ) ) ;
#43454 = CONICAL_SURFACE ( 'NONE', #66415, 0.1000000000000000056, 0.003490658503988666988 ) ;
#43455 = EDGE_CURVE ( 'NONE', #44343, #84404, #7516, .T. ) ;
#43456 = CONICAL_SURFACE ( 'NONE', #50007, 0.1000000000000000472, 0.003490658503988666988 ) ;
#43457 = EDGE_LOOP ( 'NONE', ( #61365, #96149 ) ) ;
#43458 = FACE_OUTER_BOUND ( 'NONE', #36362, .T. ) ;
#43459 = EDGE_LOOP ( 'NONE', ( #113729, #111352 ) ) ;
#43460 = PLANE ( 'NONE',  #91926 ) ;
#43461 = CARTESIAN_POINT ( 'NONE',  ( -3.150000000000030109, 12.50000000000000000, 1.753560074763284016 ) ) ;
#43462 = CARTESIAN_POINT ( 'NONE',  ( 129.5000000000000000, 0.000000000000000000, 0.000000000000000000 ) ) ;
#43463 = ORIENTED_EDGE ( 'NONE', *, *, #62451, .F. ) ;
#43464 = AXIS2_PLACEMENT_3D ( 'NONE', #41255, #121721, #50404 ) ;
#43465 = DIRECTION ( 'NONE',  ( -0.000000000000000000, -1.000000000000000000, -0.000000000000000000 ) ) ;
#43466 = CARTESIAN_POINT ( 'NONE',  ( 11.64999999999990798, 2.500000000000000000, 5.802370205355744659 ) ) ;
#43467 = CIRCLE ( 'NONE', #60193, 0.06509327318403745899 ) ;
#43468 = ORIENTED_EDGE ( 'NONE', *, *, #55250, .F. ) ;
#43469 = VECTOR ( 'NONE', #43307, 1000.000000000000000 ) ;
#43470 = ORIENTED_EDGE ( 'NONE', *, *, #14410, .F. ) ;
#43471 = EDGE_LOOP ( 'NONE', ( #56566, #36665 ) ) ;
#43472 = DIRECTION ( 'NONE',  ( 0.000000000000000000, 1.000000000000000000, 0.000000000000000000 ) ) ;
#43473 = CARTESIAN_POINT ( 'NONE',  ( -5.650000000000019895, 12.50000000000000000, 6.776507416713035248 ) ) ;
#43474 = DIRECTION ( 'NONE',  ( 0.000000000000000000, 1.000000000000000000, -1.224646799147353207E-16 ) ) ;
#43475 = VERTEX_POINT ( 'NONE', #77281 ) ;
#43476 = CIRCLE ( 'NONE', #53927, 0.06509327318403745899 ) ;
#43477 = CARTESIAN_POINT ( 'NONE',  ( 175.5000000000000000, 5.510910596163088569E-16, 4.000000000000000000 ) ) ;
#43478 = FACE_OUTER_BOUND ( 'NONE', #8643, .T. ) ;
#43479 = CIRCLE ( 'NONE', #62353, 0.09999999999999982514 ) ;
#43480 = ORIENTED_EDGE ( 'NONE', *, *, #2173, .T. ) ;
#43481 = DIRECTION ( 'NONE',  ( -0.000000000000000000, 1.000000000000000000, -0.000000000000000000 ) ) ;
#43482 = CARTESIAN_POINT ( 'NONE',  ( 0.8499999999999536815, 12.50000000000000000, 6.495190528383297135 ) ) ;
#43483 = CONICAL_SURFACE ( 'NONE', #5790, 0.09999999999999982514, 0.003490658503988666988 ) ;
#43484 = DIRECTION ( 'NONE',  ( 0.000000000000000000, -0.000000000000000000, 1.000000000000000000 ) ) ;
#43485 = CARTESIAN_POINT ( 'NONE',  ( 11.69999999999990870, 12.50000000000000000, 4.265033745738159077 ) ) ;
#43486 = DIRECTION ( 'NONE',  ( -0.000000000000000000, -1.000000000000000000, -0.000000000000000000 ) ) ;
#43487 = DIRECTION ( 'NONE',  ( 0.000000000000000000, 1.000000000000000000, 0.000000000000000000 ) ) ;
#43488 = DIRECTION ( 'NONE',  ( 0.000000000000000000, 1.000000000000000000, 0.000000000000000000 ) ) ;
#43489 = AXIS2_PLACEMENT_3D ( 'NONE', #66980, #16591, #85351 ) ;
#43490 = AXIS2_PLACEMENT_3D ( 'NONE', #115053, #77087, #25387 ) ;
#43491 = EDGE_CURVE ( 'NONE', #67379, #60185, #30137, .T. ) ;
#43492 = ORIENTED_EDGE ( 'NONE', *, *, #45182, .F. ) ;
#43493 = EDGE_LOOP ( 'NONE', ( #3715, #16985, #79161, #25953 ) ) ;
#43494 = ORIENTED_EDGE ( 'NONE', *, *, #117673, .T. ) ;
#43495 = EDGE_LOOP ( 'NONE', ( #114603, #84715 ) ) ;
#43496 = DIRECTION ( 'NONE',  ( -4.274815082592931898E-19, -0.9999939076577903929, -0.003490651415223739937 ) ) ;
#43497 = DIRECTION ( 'NONE',  ( -0.000000000000000000, 1.000000000000000000, -0.000000000000000000 ) ) ;
#43498 = CARTESIAN_POINT ( 'NONE',  ( 8.949999999999921130, 2.500000000000000000, -6.741600689897078169 ) ) ;
#43499 = CIRCLE ( 'NONE', #129200, 2.318304356886072615 ) ;
#43500 = VERTEX_POINT ( 'NONE', #70047 ) ;
#43501 = EDGE_CURVE ( 'NONE', #76876, #108726, #38000, .T. ) ;
#43502 = FACE_BOUND ( 'NONE', #97209, .T. ) ;
#43503 = EDGE_CURVE ( 'NONE', #92053, #69317, #67425, .T. ) ;
#43504 = DIRECTION ( 'NONE',  ( 0.000000000000000000, 0.000000000000000000, 1.000000000000000000 ) ) ;
#43505 = CARTESIAN_POINT ( 'NONE',  ( -8.150000000000012790, 2.500000000000000000, -1.818653347947326138 ) ) ;
#43506 = DIRECTION ( 'NONE',  ( 0.000000000000000000, 0.000000000000000000, 1.000000000000000000 ) ) ;
#43508 = AXIS2_PLACEMENT_3D ( 'NONE', #2691, #124420, #82573 ) ;
#43507 = CIRCLE ( 'NONE', #12166, 0.06509327318403745899 ) ;
#43509 = CARTESIAN_POINT ( 'NONE',  ( 7.099999999999928590, 2.500000000000000000, -5.022947341949754119 ) ) ;
#43510 = CARTESIAN_POINT ( 'NONE',  ( 21.34481565588170682, -0.7053969147713181620, 2.184679923000722113 ) ) ;
#43511 = EDGE_CURVE ( 'NONE', #40817, #25459, #108025, .T. ) ;
#43512 = DIRECTION ( 'NONE',  ( 0.000000000000000000, -0.000000000000000000, 1.000000000000000000 ) ) ;
#43513 = EDGE_CURVE ( 'NONE', #1730, #65247, #124321, .T. ) ;
#43514 = CARTESIAN_POINT ( 'NONE',  ( -5.600000000000023626, 2.500000000000000000, -4.776537180435977525 ) ) ;
#43515 = DIRECTION ( 'NONE',  ( -0.000000000000000000, 1.000000000000000000, -0.000000000000000000 ) ) ;
#43516 = EDGE_CURVE ( 'NONE', #79091, #73015, #97562, .T. ) ;
#43517 = FACE_OUTER_BOUND ( 'NONE', #39166, .T. ) ;
#43518 = EDGE_CURVE ( 'NONE', #43610, #49071, #30257, .T. ) ;
#43519 = ADVANCED_FACE ( 'NONE', ( #98204 ), #109973, .F. ) ;
#43520 = ORIENTED_EDGE ( 'NONE', *, *, #25914, .F. ) ;
#43521 = ORIENTED_EDGE ( 'NONE', *, *, #64077, .T. ) ;
#43522 = EDGE_LOOP ( 'NONE', ( #69444, #99, #6491, #107006 ) ) ;
#43523 = ORIENTED_EDGE ( 'NONE', *, *, #101590, .F. ) ;
#43524 = EDGE_LOOP ( 'NONE', ( #35175, #99250 ) ) ;
#43525 = ORIENTED_EDGE ( 'NONE', *, *, #65456, .T. ) ;
#43526 = DIRECTION ( 'NONE',  ( 0.000000000000000000, 1.000000000000000000, 0.000000000000000000 ) ) ;
#43527 = VERTEX_POINT ( 'NONE', #87091 ) ;
#43528 = EDGE_CURVE ( 'NONE', #40454, #97017, #84616, .T. ) ;
#43529 = ORIENTED_EDGE ( 'NONE', *, *, #55883, .F. ) ;
#43530 = ADVANCED_FACE ( 'NONE', ( #88368 ), #109658, .T. ) ;
#43532 = CIRCLE ( 'NONE', #127145, 0.1000000000000002554 ) ;
#43531 = CARTESIAN_POINT ( 'NONE',  ( 14.37945523803864845, -1.500000000000095701, 7.667852710427166762 ) ) ;
#43533 = DIRECTION ( 'NONE',  ( 0.000000000000000000, 0.000000000000000000, 1.000000000000000000 ) ) ;
#43534 = DIRECTION ( 'NONE',  ( 0.000000000000000000, 0.000000000000000000, -1.000000000000000000 ) ) ;
#43535 = CIRCLE ( 'NONE', #37270, 0.09999999999999982514 ) ;
#43536 = ORIENTED_EDGE ( 'NONE', *, *, #82551, .F. ) ;
#43537 = FACE_OUTER_BOUND ( 'NONE', #22414, .T. ) ;
#43538 = AXIS2_PLACEMENT_3D ( 'NONE', #72196, #81376, #42756 ) ;
#43539 = ORIENTED_EDGE ( 'NONE', *, *, #70349, .F. ) ;
#43540 = CIRCLE ( 'NONE', #81175, 0.06509327318403743123 ) ;
#43541 = ORIENTED_EDGE ( 'NONE', *, *, #77508, .F. ) ;
#43542 = DIRECTION ( 'NONE',  ( -0.000000000000000000, -1.000000000000000000, -0.000000000000000000 ) ) ;
#43543 = LINE ( 'NONE', #103086, #60852 ) ;
#43544 = VERTEX_POINT ( 'NONE', #99518 ) ;
#43546 = ORIENTED_EDGE ( 'NONE', *, *, #50168, .F. ) ;
#43545 = CIRCLE ( 'NONE', #118831, 0.09999999999999999167 ) ;
#43547 = PLANE ( 'NONE',  #33876 ) ;
#43548 = CIRCLE ( 'NONE', #18391, 0.1000000000000002554 ) ;
#43549 = DIRECTION ( 'NONE',  ( 0.000000000000000000, -0.000000000000000000, 1.000000000000000000 ) ) ;
#43550 = DIRECTION ( 'NONE',  ( 0.000000000000000000, 1.000000000000000000, 0.000000000000000000 ) ) ;
#43551 = DIRECTION ( 'NONE',  ( -4.274815082592931898E-19, -0.9999939076577903929, -0.003490651415223739937 ) ) ;
#43552 = LINE ( 'NONE', #124680, #2234 ) ;
#43553 = ADVANCED_FACE ( 'NONE', ( #128994 ), #63971, .T. ) ;
#43554 = ORIENTED_EDGE ( 'NONE', *, *, #36580, .T. ) ;
#43555 = EDGE_CURVE ( 'NONE', #19960, #72741, #40720, .T. ) ;
#43556 = DIRECTION ( 'NONE',  ( 0.000000000000000000, 1.000000000000000000, 0.000000000000000000 ) ) ;
#43557 = CIRCLE ( 'NONE', #110428, 0.1000000000000002554 ) ;
#43558 = EDGE_LOOP ( 'NONE', ( #106374, #30092, #103326, #41650 ) ) ;
#43560 = ADVANCED_FACE ( 'NONE', ( #1294 ), #1932, .T. ) ;
#43559 = PLANE ( 'NONE',  #29484 ) ;
#43561 = EDGE_LOOP ( 'NONE', ( #92880, #120324, #110891, #69280 ) ) ;
#43562 = CARTESIAN_POINT ( 'NONE',  ( 6.249999999999932498, 12.50000000000000000, 5.802370205355744659 ) ) ;
#43563 = CARTESIAN_POINT ( 'NONE',  ( 8.749999999999921840, 12.50000000000000000, -5.802370205355749988 ) ) ;
#43564 = CIRCLE ( 'NONE', #104176, 0.06509327318403745899 ) ;
#43565 = PLANE ( 'NONE',  #6854 ) ;
#43566 = ADVANCED_FACE ( 'NONE', ( #32069 ), #71987, .T. ) ;
#43567 = DIRECTION ( 'NONE',  ( 0.000000000000000000, 1.000000000000000000, 0.000000000000000000 ) ) ;
#43568 = ORIENTED_EDGE ( 'NONE', *, *, #75141, .T. ) ;
#43569 = EDGE_CURVE ( 'NONE', #84139, #114467, #30783, .T. ) ;
#43571 = AXIS2_PLACEMENT_3D ( 'NONE', #68664, #9096, #47112 ) ;
#43570 = DIRECTION ( 'NONE',  ( 0.000000000000000000, 0.000000000000000000, -1.000000000000000000 ) ) ;
#43572 = EDGE_CURVE ( 'NONE', #41344, #27533, #49124, .T. ) ;
#43573 =( GEOMETRIC_REPRESENTATION_CONTEXT ( 3 ) GLOBAL_UNCERTAINTY_ASSIGNED_CONTEXT ( ( #121523 ) ) GLOBAL_UNIT_ASSIGNED_CONTEXT ( ( #115286, #55749, #95689 ) ) REPRESENTATION_CONTEXT ( 'NONE', 'WORKASPACE' ) );
#43574 = CARTESIAN_POINT ( 'NONE',  ( 6.049999999999932321, 2.500000000000000000, -1.918653347947326004 ) ) ;
#43575 = ORIENTED_EDGE ( 'NONE', *, *, #99348, .T. ) ;
#43576 = ORIENTED_EDGE ( 'NONE', *, *, #12546, .F. ) ;
#43577 = ORIENTED_EDGE ( 'NONE', *, *, #23427, .F. ) ;
#43578 = CARTESIAN_POINT ( 'NONE',  ( 6.249999999999930722, 2.500000000000000000, 7.288010851410849256 ) ) ;
#43579 = CARTESIAN_POINT ( 'NONE',  ( 7.099999999999928590, 2.500000000000000000, 3.637306695894644726 ) ) ;
#43580 = CARTESIAN_POINT ( 'NONE',  ( 185.1510416670080872, 4.367472073101518859, -7.564683531249999149 ) ) ;
#43582 = CIRCLE ( 'NONE', #18509, 0.09999999999999982514 ) ;
#43581 = DIRECTION ( 'NONE',  ( 0.000000000000000000, 0.000000000000000000, 1.000000000000000000 ) ) ;
#43583 = ADVANCED_FACE ( 'NONE', ( #123014 ), #3241, .T. ) ;
#43584 = CARTESIAN_POINT ( 'NONE',  ( 186.0000000000000000, 0.000000000000000000, 7.700000000000000178 ) ) ;
#43585 = CIRCLE ( 'NONE', #10206, 0.06509327318403743123 ) ;
#43586 = PLANE ( 'NONE',  #90729 ) ;
#43587 = DIRECTION ( 'NONE',  ( 0.000000000000000000, 0.000000000000000000, -1.000000000000000000 ) ) ;
#43588 = CIRCLE ( 'NONE', #125141, 0.06509327318403745899 ) ;
#43589 = ORIENTED_EDGE ( 'NONE', *, *, #17085, .F. ) ;
#43590 = CARTESIAN_POINT ( 'NONE',  ( 11.24999999999990941, 12.50000000000000000, -1.472243186433550122 ) ) ;
#43591 = ORIENTED_EDGE ( 'NONE', *, *, #33148, .T. ) ;
#43592 = CARTESIAN_POINT ( 'NONE',  ( 9.399999999999915090, 12.50000000000000000, 3.983716857408420964 ) ) ;
#43593 = VECTOR ( 'NONE', #118329, 1000.000000000000000 ) ;
#43594 = PLANE ( 'NONE',  #18014 ) ;
#43595 = EDGE_CURVE ( 'NONE', #59835, #12583, #126257, .T. ) ;
#43596 = DIRECTION ( 'NONE',  ( 0.000000000000000000, -0.9999939076577903929, 0.003490651415223739937 ) ) ;
#43597 = DIRECTION ( 'NONE',  ( -4.274815082592931898E-19, -0.9999939076577903929, -0.003490651415223739937 ) ) ;
#43598 = EDGE_LOOP ( 'NONE', ( #87800, #120110 ) ) ;
#43599 = AXIS2_PLACEMENT_3D ( 'NONE', #33665, #74232, #15284 ) ;
#43600 = DIRECTION ( 'NONE',  ( -0.000000000000000000, -1.000000000000000000, -0.000000000000000000 ) ) ;
#43602 = EDGE_LOOP ( 'NONE', ( #47999, #127862 ) ) ;
#43601 = DIRECTION ( 'NONE',  ( -4.274815082592931898E-19, -0.9999939076577903929, -0.003490651415223739937 ) ) ;
#43603 = VERTEX_POINT ( 'NONE', #103373 ) ;
#43604 = DIRECTION ( 'NONE',  ( -0.000000000000000000, -1.000000000000000000, -0.000000000000000000 ) ) ;
#43605 = ADVANCED_FACE ( 'NONE', ( #113176 ), #95171, .T. ) ;
#43606 = EDGE_LOOP ( 'NONE', ( #129217, #57922, #17838, #72094 ) ) ;
#43607 = ORIENTED_EDGE ( 'NONE', *, *, #64475, .T. ) ;
#43608 = DIRECTION ( 'NONE',  ( 0.000000000000000000, -0.000000000000000000, 1.000000000000000000 ) ) ;
#43609 = CIRCLE ( 'NONE', #116740, 0.06509327318403745899 ) ;
#43610 = VERTEX_POINT ( 'NONE', #60864 ) ;
#43611 = CARTESIAN_POINT ( 'NONE',  ( 17.33812564108800203, 2.538896947916920777, -5.379288978441866931 ) ) ;
#43612 = FACE_OUTER_BOUND ( 'NONE', #101001, .T. ) ;
#43613 = DIRECTION ( 'NONE',  ( 0.000000000000000000, 0.000000000000000000, 1.000000000000000000 ) ) ;
#43614 = ORIENTED_EDGE ( 'NONE', *, *, #33975, .F. ) ;
#43615 = CIRCLE ( 'NONE', #49881, 0.06509327318403745899 ) ;
#43616 = CONICAL_SURFACE ( 'NONE', #24818, 0.1000000000000000472, 0.003490658503988666988 ) ;
#43617 = AXIS2_PLACEMENT_3D ( 'NONE', #112441, #51591, #83626 ) ;
#43618 = LINE ( 'NONE', #63885, #123562 ) ;
#43620 = ORIENTED_EDGE ( 'NONE', *, *, #2762, .T. ) ;
#43619 = CARTESIAN_POINT ( 'NONE',  ( -10.85000000000000142, 2.500000000000000000, 2.165063509461097713 ) ) ;
#43621 = CARTESIAN_POINT ( 'NONE',  ( 11.24999999999991118, 2.500000000000000000, -2.857883832488653741 ) ) ;
#43622 = EDGE_CURVE ( 'NONE', #43976, #100575, #47058, .T. ) ;
#43623 = CARTESIAN_POINT ( 'NONE',  ( 17.27571223834416969, -2.230085210383244476, 5.047251339833896289 ) ) ;
#43624 = AXIS2_PLACEMENT_3D ( 'NONE', #108379, #90013, #116893 ) ;
#43625 = VERTEX_POINT ( 'NONE', #22248 ) ;
#43626 = CIRCLE ( 'NONE', #77061, 0.06509327318403745899 ) ;
#43627 = ORIENTED_EDGE ( 'NONE', *, *, #12136, .F. ) ;
#43628 = AXIS2_PLACEMENT_3D ( 'NONE', #77460, #31593, #80701 ) ;
#43629 = EDGE_LOOP ( 'NONE', ( #10252, #44683, #104120, #115717 ) ) ;
#43630 = VERTEX_POINT ( 'NONE', #31416 ) ;
#43631 = DIRECTION ( 'NONE',  ( 0.000000000000000000, 1.000000000000000000, 0.000000000000000000 ) ) ;
#43632 = CARTESIAN_POINT ( 'NONE',  ( -10.20000000000000639, 12.50000000000000000, -3.983716857408421852 ) ) ;
#43633 = CARTESIAN_POINT ( 'NONE',  ( -14.34999999999998543, 12.50000000000000000, -1.753560074763286236 ) ) ;
#43634 = FACE_BOUND ( 'NONE', #10117, .T. ) ;
#43635 = ORIENTED_EDGE ( 'NONE', *, *, #102641, .F. ) ;
#43636 = CARTESIAN_POINT ( 'NONE',  ( 185.5729166673494319, 4.445597072760120838, -7.699999999999998401 ) ) ;
#43637 = CIRCLE ( 'NONE', #116768, 0.1000000000000002554 ) ;
#43638 = FACE_OUTER_BOUND ( 'NONE', #68285, .T. ) ;
#43639 = CARTESIAN_POINT ( 'NONE',  ( 9.549999999999915445, 2.500000000000000000, -2.165063509461101710 ) ) ;
#43640 = AXIS2_PLACEMENT_3D ( 'NONE', #128262, #108602, #9110 ) ;
#43641 = DIRECTION ( 'NONE',  ( -0.000000000000000000, -1.000000000000000000, -0.000000000000000000 ) ) ;
#43642 = FACE_OUTER_BOUND ( 'NONE', #111596, .T. ) ;
#43643 = DIRECTION ( 'NONE',  ( -0.000000000000000000, -1.000000000000000000, -0.000000000000000000 ) ) ;
#43644 = VECTOR ( 'NONE', #6141, 1000.000000000000000 ) ;
#43645 = DIRECTION ( 'NONE',  ( -0.000000000000000000, -1.000000000000000000, -0.000000000000000000 ) ) ;
#43646 = ADVANCED_FACE ( 'NONE', ( #41887 ), #13027, .T. ) ;
#43647 = ORIENTED_EDGE ( 'NONE', *, *, #61499, .T. ) ;
#43648 = VERTEX_POINT ( 'NONE', #62172 ) ;
#43649 = ORIENTED_EDGE ( 'NONE', *, *, #53415, .F. ) ;
#43650 = ORIENTED_EDGE ( 'NONE', *, *, #47946, .F. ) ;
#43651 = ORIENTED_EDGE ( 'NONE', *, *, #5932, .T. ) ;
#43652 = CIRCLE ( 'NONE', #10192, 0.06509327318403745899 ) ;
#43653 = DIRECTION ( 'NONE',  ( 0.000000000000000000, 1.000000000000000000, 0.000000000000000000 ) ) ;
#43654 = LINE ( 'NONE', #2397, #63329 ) ;
#43655 = ORIENTED_EDGE ( 'NONE', *, *, #127594, .T. ) ;
#43656 = FACE_BOUND ( 'NONE', #82401, .T. ) ;
#43657 = CARTESIAN_POINT ( 'NONE',  ( -6.050000000000018474, 12.50000000000000000, 2.511473670974873507 ) ) ;
#43658 = ADVANCED_FACE ( 'NONE', ( #92247 ), #51065, .T. ) ;
#43659 = CONICAL_SURFACE ( 'NONE', #125212, 0.1000000000000002554, 0.003490658503988666988 ) ;
#43660 = ORIENTED_EDGE ( 'NONE', *, *, #122144, .F. ) ;
#43661 = EDGE_CURVE ( 'NONE', #96104, #38146, #76292, .T. ) ;
#43662 = DIRECTION ( 'NONE',  ( 0.000000000000000000, 1.000000000000000000, 0.000000000000000000 ) ) ;
#43663 = ADVANCED_FACE ( 'NONE', ( #21584 ), #128560, .T. ) ;
#43664 = DIRECTION ( 'NONE',  ( 0.000000000000000000, 0.000000000000000000, 1.000000000000000000 ) ) ;
#43665 = ADVANCED_FACE ( 'NONE', ( #42536 ), #52980, .T. ) ;
#43666 = CARTESIAN_POINT ( 'NONE',  ( 11.89999999999990798, 12.50000000000000000, -3.983716857408426293 ) ) ;
#43667 = ADVANCED_FACE ( 'NONE', ( #96116 ), #65813, .T. ) ;
#43668 = ORIENTED_EDGE ( 'NONE', *, *, #45862, .F. ) ;
#43670 = AXIS2_PLACEMENT_3D ( 'NONE', #83431, #40944, #72325 ) ;
#43669 = CIRCLE ( 'NONE', #125219, 0.06509327318403745899 ) ;
#43671 = DIRECTION ( 'NONE',  ( -0.000000000000000000, -1.000000000000000000, -0.000000000000000000 ) ) ;
#43673 = EDGE_LOOP ( 'NONE', ( #66841, #73290 ) ) ;
#43672 = AXIS2_PLACEMENT_3D ( 'NONE', #76597, #6523, #36690 ) ;
#43674 = ADVANCED_FACE ( 'NONE', ( #83733 ), #124416, .T. ) ;
#43675 = VERTEX_POINT ( 'NONE', #45104 ) ;
#43676 = EDGE_CURVE ( 'NONE', #88341, #59884, #90966, .T. ) ;
#43677 = ORIENTED_EDGE ( 'NONE', *, *, #97135, .T. ) ;
#43678 = CARTESIAN_POINT ( 'NONE',  ( -8.350000000000008527, 12.50000000000000000, 5.867463478539781896 ) ) ;
#43679 = FACE_OUTER_BOUND ( 'NONE', #107442, .T. ) ;
#43680 = CARTESIAN_POINT ( 'NONE',  ( -10.65000000000000213, 12.50000000000000000, 6.841600689897072485 ) ) ;
#43681 = AXIS2_PLACEMENT_3D ( 'NONE', #44814, #25151, #34356 ) ;
#43682 = VERTEX_POINT ( 'NONE', #105943 ) ;
#43683 = EDGE_CURVE ( 'NONE', #11681, #112102, #80515, .T. ) ;
#43684 = CARTESIAN_POINT ( 'NONE',  ( 15.59999999999988951, 12.50000000000000000, 0.3464101615137735735 ) ) ;
#43685 = ADVANCED_FACE ( 'NONE', ( #95478 ), #84700, .T. ) ;
#43686 = DIRECTION ( 'NONE',  ( 0.000000000000000000, -0.9999939076577903929, 0.003490651415223739937 ) ) ;
#43687 = EDGE_CURVE ( 'NONE', #126108, #51535, #82569, .T. ) ;
#43690 = AXIS2_PLACEMENT_3D ( 'NONE', #125547, #26076, #76464 ) ;
#43689 = CARTESIAN_POINT ( 'NONE',  ( 9.349999999999919709, 2.500000000000000000, -6.148780366869526226 ) ) ;
#43688 = CONICAL_SURFACE ( 'NONE', #26944, 0.1000000000000002554, 0.003490658503988666988 ) ;
#43691 = CARTESIAN_POINT ( 'NONE',  ( 185.6562500006828316, 8.891194145520236347, 5.444286225454521982E-16 ) ) ;
#43692 = VERTEX_POINT ( 'NONE', #45743 ) ;
#43693 = CIRCLE ( 'NONE', #37424, 0.06509327318403745899 ) ;
#43694 = LINE ( 'NONE', #82956, #70421 ) ;
#43695 = ADVANCED_FACE ( 'NONE', ( #33986 ), #99288, .T. ) ;
#43696 = ORIENTED_EDGE ( 'NONE', *, *, #109256, .F. ) ;
#43697 = DIRECTION ( 'NONE',  ( -0.000000000000000000, 1.000000000000000000, -0.000000000000000000 ) ) ;
#43699 = AXIS2_PLACEMENT_3D ( 'NONE', #35237, #43772, #52288 ) ;
#43698 = CONICAL_SURFACE ( 'NONE', #114674, 0.1000000000000002554, 0.003490658503988666988 ) ;
#43700 = ORIENTED_EDGE ( 'NONE', *, *, #29444, .T. ) ;
#43701 = ORIENTED_EDGE ( 'NONE', *, *, #82711, .T. ) ;
#43702 = DIRECTION ( 'NONE',  ( -0.000000000000000000, -1.000000000000000000, -0.000000000000000000 ) ) ;
#43703 = DIRECTION ( 'NONE',  ( 0.000000000000000000, 0.000000000000000000, -1.000000000000000000 ) ) ;
#43704 = CARTESIAN_POINT ( 'NONE',  ( 3.149999999999942624, 2.500000000000000000, 6.941600689897073018 ) ) ;
#43705 = DIRECTION ( 'NONE',  ( 0.000000000000000000, 1.000000000000000000, 0.000000000000000000 ) ) ;
#43706 = LINE ( 'NONE', #123513, #22521 ) ;
#43707 = EDGE_LOOP ( 'NONE', ( #104152, #16916, #52197, #55957 ) ) ;
#43708 = EDGE_LOOP ( 'NONE', ( #55260, #73291 ) ) ;
#43709 = DIRECTION ( 'NONE',  ( 0.000000000000000000, 0.000000000000000000, 1.000000000000000000 ) ) ;
#43710 = DIRECTION ( 'NONE',  ( 0.000000000000000000, 0.000000000000000000, 1.000000000000000000 ) ) ;
#43711 = DIRECTION ( 'NONE',  ( 0.4999999999999992228, 0.000000000000000000, 0.8660254037844391517 ) ) ;
#43713 = VERTEX_POINT ( 'NONE', #85006 ) ;
#43712 = AXIS2_PLACEMENT_3D ( 'NONE', #112232, #39164, #79075 ) ;
#43714 = ORIENTED_EDGE ( 'NONE', *, *, #128660, .T. ) ;
#43715 = CARTESIAN_POINT ( 'NONE',  ( 9.999999999999948486, 12.50000000000000000, 4.330127018922196314 ) ) ;
#43716 = EDGE_LOOP ( 'NONE', ( #31128, #4559, #98863, #45338 ) ) ;
#43717 = CARTESIAN_POINT ( 'NONE',  ( 6.049999999999932321, 12.50000000000000000, 1.883746621131358934 ) ) ;
#43718 = AXIS2_PLACEMENT_3D ( 'NONE', #94933, #7177, #15705 ) ;
#43720 = DIRECTION ( 'NONE',  ( -0.000000000000000000, -1.000000000000000000, -0.000000000000000000 ) ) ;
#43719 = VECTOR ( 'NONE', #106655, 1000.000000000000000 ) ;
#43721 = ORIENTED_EDGE ( 'NONE', *, *, #71565, .F. ) ;
#43722 = FACE_OUTER_BOUND ( 'NONE', #37064, .T. ) ;
#43723 = DIRECTION ( 'NONE',  ( 0.000000000000000000, 0.000000000000000000, 1.000000000000000000 ) ) ;
#43724 = CARTESIAN_POINT ( 'NONE',  ( -1.900000000000035438, 12.50000000000000000, 3.983716857408420076 ) ) ;
#43725 = FACE_OUTER_BOUND ( 'NONE', #62927, .T. ) ;
#43726 = AXIS2_PLACEMENT_3D ( 'NONE', #21185, #20552, #100400 ) ;
#43727 = ORIENTED_EDGE ( 'NONE', *, *, #114252, .T. ) ;
#43728 = ADVANCED_FACE ( 'NONE', ( #53625 ), #115999, .T. ) ;
#43730 = DIRECTION ( 'NONE',  ( 0.000000000000000000, 0.000000000000000000, -1.000000000000000000 ) ) ;
#43729 = AXIS2_PLACEMENT_3D ( 'NONE', #114991, #65900, #25322 ) ;
#43732 = EDGE_CURVE ( 'NONE', #78632, #16842, #5789, .T. ) ;
#43731 = CARTESIAN_POINT ( 'NONE',  ( 48.84100846698766674, -2.320798421879386453, 5.300800859560139244 ) ) ;
#43733 = EDGE_LOOP ( 'NONE', ( #15227, #106097, #14743, #102233 ) ) ;
#43734 = VERTEX_POINT ( 'NONE', #85656 ) ;
#43735 = CARTESIAN_POINT ( 'NONE',  ( 183.9010416670080588, -4.367472073101519747, 7.564683531249999149 ) ) ;
#43736 = LINE ( 'NONE', #5700, #55418 ) ;
#43737 = DIRECTION ( 'NONE',  ( -0.000000000000000000, 1.000000000000000000, -0.000000000000000000 ) ) ;
#43738 = CONICAL_SURFACE ( 'NONE', #116852, 0.09999999999999982514, 0.003490658503988666988 ) ;
#43739 = FACE_OUTER_BOUND ( 'NONE', #21249, .T. ) ;
#43740 = ADVANCED_FACE ( 'NONE', ( #125568 ), #42879, .T. ) ;
#43741 = DIRECTION ( 'NONE',  ( 0.000000000000000000, -0.9999939076577903929, 0.003490651415223739937 ) ) ;
#43742 = CIRCLE ( 'NONE', #127349, 0.06509327318403745899 ) ;
#43743 = FACE_OUTER_BOUND ( 'NONE', #86615, .T. ) ;
#43744 = DIRECTION ( 'NONE',  ( 0.000000000000000000, 1.000000000000000000, 0.000000000000000000 ) ) ;
#43745 = LINE ( 'NONE', #24725, #28048 ) ;
#43746 = CARTESIAN_POINT ( 'NONE',  ( -13.34999999999999076, 2.500000000000000000, 2.165063509461101265 ) ) ;
#43747 = CARTESIAN_POINT ( 'NONE',  ( -3.350000000000028511, 12.50000000000000000, 1.472243186433545459 ) ) ;
#43748 = FACE_OUTER_BOUND ( 'NONE', #117776, .T. ) ;
#43749 = VERTEX_POINT ( 'NONE', #124941 ) ;
#43750 = ORIENTED_EDGE ( 'NONE', *, *, #75759, .F. ) ;
#43751 = ORIENTED_EDGE ( 'NONE', *, *, #124846, .F. ) ;
#43752 = AXIS2_PLACEMENT_3D ( 'NONE', #46093, #57194, #57852 ) ;
#43753 = ORIENTED_EDGE ( 'NONE', *, *, #106270, .T. ) ;
#43754 = DIRECTION ( 'NONE',  ( 0.000000000000000000, 0.000000000000000000, 1.000000000000000000 ) ) ;
#43755 = DIRECTION ( 'NONE',  ( 0.000000000000000000, 1.000000000000000000, 0.000000000000000000 ) ) ;
#43756 = ORIENTED_EDGE ( 'NONE', *, *, #44548, .T. ) ;
#43757 = DIRECTION ( 'NONE',  ( -0.000000000000000000, 1.000000000000000000, -0.000000000000000000 ) ) ;
#43758 = DIRECTION ( 'NONE',  ( 0.000000000000000000, -0.000000000000000000, 1.000000000000000000 ) ) ;
#43760 = ORIENTED_EDGE ( 'NONE', *, *, #67563, .F. ) ;
#43759 = DIRECTION ( 'NONE',  ( 0.000000000000000000, -0.000000000000000000, 1.000000000000000000 ) ) ;
#43761 = DIRECTION ( 'NONE',  ( 0.000000000000000000, 1.000000000000000000, 0.000000000000000000 ) ) ;
#43762 = CIRCLE ( 'NONE', #72986, 0.06509327318403745899 ) ;
#43763 = DIRECTION ( 'NONE',  ( -4.274815082592931898E-19, -0.9999939076577903929, -0.003490651415223739937 ) ) ;
#43764 = ORIENTED_EDGE ( 'NONE', *, *, #43819, .T. ) ;
#43765 = CIRCLE ( 'NONE', #10298, 0.1000000000000002554 ) ;
#43766 = ORIENTED_EDGE ( 'NONE', *, *, #49447, .T. ) ;
#43767 = EDGE_LOOP ( 'NONE', ( #37433, #122055, #88555, #40105 ) ) ;
#43768 = ORIENTED_EDGE ( 'NONE', *, *, #45394, .F. ) ;
#43769 = DIRECTION ( 'NONE',  ( 0.000000000000000000, 1.000000000000000000, 0.000000000000000000 ) ) ;
#43770 = FACE_OUTER_BOUND ( 'NONE', #9400, .T. ) ;
#43771 = DIRECTION ( 'NONE',  ( 0.000000000000000000, 0.000000000000000000, 1.000000000000000000 ) ) ;
#43772 = DIRECTION ( 'NONE',  ( -0.000000000000000000, -1.000000000000000000, -0.000000000000000000 ) ) ;
#43773 = ORIENTED_EDGE ( 'NONE', *, *, #126989, .T. ) ;
#43775 = VECTOR ( 'NONE', #73707, 1000.000000000000000 ) ;
#43774 = CIRCLE ( 'NONE', #116892, 0.06509327318403745899 ) ;
#43776 = DIRECTION ( 'NONE',  ( 0.000000000000000000, -0.9999939076577903929, 0.003490651415223739937 ) ) ;
#43778 = ORIENTED_EDGE ( 'NONE', *, *, #34960, .F. ) ;
#43777 = EDGE_CURVE ( 'NONE', #61872, #64688, #17791, .T. ) ;
#43779 = CARTESIAN_POINT ( 'NONE',  ( -6.249999999999981348, 2.500000000000000000, 6.595190528383296780 ) ) ;
#43781 = CONICAL_SURFACE ( 'NONE', #116898, 0.09999999999999982514, 0.003490658503988666988 ) ;
#43780 = CARTESIAN_POINT ( 'NONE',  ( 10.28037028461948488, -1.499999999999745981, -9.136909653556401167 ) ) ;
#43782 = DIRECTION ( 'NONE',  ( 0.000000000000000000, 0.000000000000000000, 1.000000000000000000 ) ) ;
#43783 = CARTESIAN_POINT ( 'NONE',  ( -3.100000000000028511, 2.500000000000000000, 0.4464101615137736623 ) ) ;
#43784 = EDGE_CURVE ( 'NONE', #62169, #107629, #43826, .T. ) ;
#43785 = ORIENTED_EDGE ( 'NONE', *, *, #106217, .F. ) ;
#43787 = CIRCLE ( 'NONE', #39594, 0.1000000000000002554 ) ;
#43786 = AXIS2_PLACEMENT_3D ( 'NONE', #41161, #121614, #60780 ) ;
#43788 = EDGE_LOOP ( 'NONE', ( #10722, #83527, #61208, #89765 ) ) ;
#43789 = EDGE_LOOP ( 'NONE', ( #119315, #40236, #13636, #7027 ) ) ;
#43790 = DIRECTION ( 'NONE',  ( -0.000000000000000000, 1.000000000000000000, -0.000000000000000000 ) ) ;
#43791 = CARTESIAN_POINT ( 'NONE',  ( -7.900000000000014566, 2.500000000000000000, -3.637306695894650055 ) ) ;
#43792 = ADVANCED_FACE ( 'NONE', ( #84369 ), #104641, .T. ) ;
#43793 = CARTESIAN_POINT ( 'NONE',  ( -11.25000000000000000, 2.500000000000000000, -7.188010851410850499 ) ) ;
#43794 = FACE_BOUND ( 'NONE', #17645, .T. ) ;
#43795 = FACE_OUTER_BOUND ( 'NONE', #106062, .T. ) ;
#43796 = CARTESIAN_POINT ( 'NONE',  ( 6.849999999999929479, 2.500000000000000000, -2.411473670974877859 ) ) ;
#43797 = LINE ( 'NONE', #5127, #72911 ) ;
#43798 = CARTESIAN_POINT ( 'NONE',  ( 187.4609375001707008, 0.000000000000000000, 7.632341765625000107 ) ) ;
#43799 = DIRECTION ( 'NONE',  ( 0.000000000000000000, 0.000000000000000000, -1.000000000000000000 ) ) ;
#43800 = DIRECTION ( 'NONE',  ( 0.000000000000000000, 1.000000000000000000, 0.000000000000000000 ) ) ;
#43801 = ORIENTED_EDGE ( 'NONE', *, *, #27110, .T. ) ;
#43802 = AXIS2_PLACEMENT_3D ( 'NONE', #20571, #29741, #120057 ) ;
#43803 = CONICAL_SURFACE ( 'NONE', #104420, 0.1000000000000002554, 0.003490658503988666988 ) ;
#43804 = CARTESIAN_POINT ( 'NONE',  ( -11.05000000000000249, 12.50000000000000000, -1.818653347947322141 ) ) ;
#43805 = EDGE_CURVE ( 'NONE', #7901, #18257, #53325, .T. ) ;
#43806 = ORIENTED_EDGE ( 'NONE', *, *, #8794, .T. ) ;
#43807 = VERTEX_POINT ( 'NONE', #114470 ) ;
#43808 = ORIENTED_EDGE ( 'NONE', *, *, #76632, .F. ) ;
#43809 = EDGE_LOOP ( 'NONE', ( #47144, #16955, #111153, #38701 ) ) ;
#43810 = DIRECTION ( 'NONE',  ( -0.000000000000000000, -1.000000000000000000, -0.000000000000000000 ) ) ;
#43811 = FACE_BOUND ( 'NONE', #7454, .T. ) ;
#43812 = CARTESIAN_POINT ( 'NONE',  ( 7.299999999999926104, 2.500000000000000000, 4.576537180435972019 ) ) ;
#43813 = VECTOR ( 'NONE', #66900, 1000.000000000000000 ) ;
#43814 = EDGE_CURVE ( 'NONE', #110184, #101430, #126478, .T. ) ;
#43815 = AXIS2_PLACEMENT_3D ( 'NONE', #80558, #38046, #49178 ) ;
#43816 = ORIENTED_EDGE ( 'NONE', *, *, #48549, .T. ) ;
#43817 = ADVANCED_FACE ( 'NONE', ( #55561 ), #107688, .T. ) ;
#43818 = CARTESIAN_POINT ( 'NONE',  ( 76.45351065597657225, 3.568406926244133803, 6.085611129013356546 ) ) ;
#43819 = EDGE_CURVE ( 'NONE', #64996, #113749, #51282, .T. ) ;
#43820 = DIRECTION ( 'NONE',  ( -0.000000000000000000, 1.000000000000000000, -0.000000000000000000 ) ) ;
#43821 = EDGE_CURVE ( 'NONE', #6862, #740, #128173, .T. ) ;
#43823 = EDGE_CURVE ( 'NONE', #112245, #35444, #69225, .T. ) ;
#43822 = CIRCLE ( 'NONE', #68929, 0.06509327318403745899 ) ;
#43824 = ORIENTED_EDGE ( 'NONE', *, *, #51485, .F. ) ;
#43825 = DIRECTION ( 'NONE',  ( 0.000000000000000000, 0.000000000000000000, 1.000000000000000000 ) ) ;
#43826 = LINE ( 'NONE', #44446, #128644 ) ;
#43827 = AXIS2_PLACEMENT_3D ( 'NONE', #73508, #113441, #24420 ) ;
#43828 = AXIS2_PLACEMENT_3D ( 'NONE', #54529, #74838, #55834 ) ;
#43829 = EDGE_CURVE ( 'NONE', #110014, #35498, #94446, .T. ) ;
#43830 = VERTEX_POINT ( 'NONE', #56817 ) ;
#43831 = DIRECTION ( 'NONE',  ( 0.000000000000000000, -0.000000000000000000, 1.000000000000000000 ) ) ;
#43832 = EDGE_CURVE ( 'NONE', #110433, #27, #113949, .T. ) ;
#43833 = CARTESIAN_POINT ( 'NONE',  ( 11.04999999999991012, 2.500000000000000000, 6.741600689897071952 ) ) ;
#43834 = ADVANCED_FACE ( 'NONE', ( #118986 ), #9020, .T. ) ;
#43835 = ORIENTED_EDGE ( 'NONE', *, *, #125927, .T. ) ;
#43836 = DIRECTION ( 'NONE',  ( 0.000000000000000000, -0.9999939076577903929, 0.003490651415223739937 ) ) ;
#43837 = ADVANCED_FACE ( 'NONE', ( #119620 ), #3235, .T. ) ;
#43838 = DIRECTION ( 'NONE',  ( 0.000000000000000000, 0.000000000000000000, 1.000000000000000000 ) ) ;
#43839 = CARTESIAN_POINT ( 'NONE',  ( -9.350000000000006750, 2.500000000000000000, 1.818653347947321475 ) ) ;
#43840 = VECTOR ( 'NONE', #119328, 1000.000000000000000 ) ;
#43841 = ORIENTED_EDGE ( 'NONE', *, *, #96541, .T. ) ;
#43842 = ORIENTED_EDGE ( 'NONE', *, *, #15496, .T. ) ;
#43843 = ADVANCED_FACE ( 'NONE', ( #18844 ), #88205, .T. ) ;
#43844 = PLANE ( 'NONE',  #49387 ) ;
#43845 = EDGE_CURVE ( 'NONE', #2544, #37147, #45098, .T. ) ;
#43846 = ORIENTED_EDGE ( 'NONE', *, *, #128990, .T. ) ;
#43847 = FACE_OUTER_BOUND ( 'NONE', #123985, .T. ) ;
#43848 = CARTESIAN_POINT ( 'NONE',  ( -7.500000000000016875, 2.500000000000000000, 0.5928203230275495006 ) ) ;
#43849 = ORIENTED_EDGE ( 'NONE', *, *, #96639, .T. ) ;
#43850 = CARTESIAN_POINT ( 'NONE',  ( 11.44999999999991047, 2.500000000000000000, -2.511473670974877948 ) ) ;
#43851 = CARTESIAN_POINT ( 'NONE',  ( 3.949999999999940670, 12.50000000000000000, 1.883746621131358934 ) ) ;
#43852 = DIRECTION ( 'NONE',  ( 0.000000000000000000, 1.000000000000000000, 0.000000000000000000 ) ) ;
#43853 = CARTESIAN_POINT ( 'NONE',  ( -10.40000000000000391, 2.500000000000000000, -3.637306695894645614 ) ) ;
#43854 = DIRECTION ( 'NONE',  ( 0.000000000000000000, 0.000000000000000000, 1.000000000000000000 ) ) ;
#43855 = ORIENTED_EDGE ( 'NONE', *, *, #50395, .F. ) ;
#43856 = EDGE_LOOP ( 'NONE', ( #128189, #100097, #70920, #64253 ) ) ;
#43857 = DIRECTION ( 'NONE',  ( 0.000000000000000000, 0.000000000000000000, -1.000000000000000000 ) ) ;
#43858 = CARTESIAN_POINT ( 'NONE',  ( 103.1680366585140405, 7.591785779721488936, -1.328661963585094918 ) ) ;
#43860 = ORIENTED_EDGE ( 'NONE', *, *, #36877, .T. ) ;
#43859 = ORIENTED_EDGE ( 'NONE', *, *, #78944, .F. ) ;
#43861 = ORIENTED_EDGE ( 'NONE', *, *, #126584, .T. ) ;
#43862 = VECTOR ( 'NONE', #5825, 1000.000000000000000 ) ;
#43863 = DIRECTION ( 'NONE',  ( -0.000000000000000000, -1.000000000000000000, -0.000000000000000000 ) ) ;
#43864 = CARTESIAN_POINT ( 'NONE',  ( -0.2000000000000412836, 12.50000000000000000, 4.676537180435972552 ) ) ;
#43865 = CARTESIAN_POINT ( 'NONE',  ( -10.85000000000000142, 2.500000000000000000, -5.802370205355746435 ) ) ;
#43866 = SURFACE_STYLE_FILL_AREA ( #84413 ) ;
#43868 = CIRCLE ( 'NONE', #33404, 0.06509327318403745899 ) ;
#43867 = CIRCLE ( 'NONE', #41815, 0.1000000000000002554 ) ;
#43869 = CYLINDRICAL_SURFACE ( 'NONE', #9725, 2.000000000000000000 ) ;
#43870 = LINE ( 'NONE', #15001, #112920 ) ;
#43871 = CARTESIAN_POINT ( 'NONE',  ( -7.300000000000018474, 12.50000000000000000, 0.3464101615137735735 ) ) ;
#43872 = DIRECTION ( 'NONE',  ( 0.000000000000000000, 0.000000000000000000, 1.000000000000000000 ) ) ;
#43873 = DIRECTION ( 'NONE',  ( 0.000000000000000000, -0.9999939076577903929, 0.003490651415223739937 ) ) ;
#43874 = CIRCLE ( 'NONE', #56356, 0.09999999999999999167 ) ;
#43875 = DIRECTION ( 'NONE',  ( 0.000000000000000000, -0.000000000000000000, 1.000000000000000000 ) ) ;
#43876 = VECTOR ( 'NONE', #38424, 1000.000000000000000 ) ;
#43877 = EDGE_LOOP ( 'NONE', ( #80168, #24466, #48954, #34494 ) ) ;
#43878 = EDGE_CURVE ( 'NONE', #109968, #112742, #55555, .T. ) ;
#43879 = EDGE_CURVE ( 'NONE', #16443, #50744, #68591, .T. ) ;
#43880 = CARTESIAN_POINT ( 'NONE',  ( -4.999999999999986677, 12.50000000000000000, 4.330127018922196314 ) ) ;
#43881 = ORIENTED_EDGE ( 'NONE', *, *, #59422, .F. ) ;
#43882 = ORIENTED_EDGE ( 'NONE', *, *, #25081, .F. ) ;
#43883 = DIRECTION ( 'NONE',  ( 0.000000000000000000, 1.000000000000000000, 0.000000000000000000 ) ) ;
#43884 = LINE ( 'NONE', #54964, #21891 ) ;
#43885 = LINE ( 'NONE', #94248, #115472 ) ;
#43886 = CARTESIAN_POINT ( 'NONE',  ( 186.5000000000000000, 0.000000000000000000, 7.700000000000000178 ) ) ;
#43887 = DIRECTION ( 'NONE',  ( 0.000000000000000000, 0.000000000000000000, 1.000000000000000000 ) ) ;
#43888 = DIRECTION ( 'NONE',  ( -0.000000000000000000, -1.000000000000000000, -0.000000000000000000 ) ) ;
#43889 = DIRECTION ( 'NONE',  ( 0.000000000000000000, 0.000000000000000000, 1.000000000000000000 ) ) ;
#43890 = VERTEX_POINT ( 'NONE', #39167 ) ;
#43891 = CARTESIAN_POINT ( 'NONE',  ( -1.650000000000034772, 12.50000000000000000, 5.802370205355744659 ) ) ;
#43892 = CARTESIAN_POINT ( 'NONE',  ( 10.59999999999991260, 2.500000000000000000, 0.4464101615137735513 ) ) ;
#43893 = VERTEX_POINT ( 'NONE', #47039 ) ;
#43894 = CIRCLE ( 'NONE', #68905, 0.06509327318403745899 ) ;
#43896 = VERTEX_POINT ( 'NONE', #28033 ) ;
#43895 = AXIS2_PLACEMENT_3D ( 'NONE', #78120, #59794, #57839 ) ;
#43897 = ORIENTED_EDGE ( 'NONE', *, *, #101908, .F. ) ;
#43898 = VERTEX_POINT ( 'NONE', #108518 ) ;
#43899 = DIRECTION ( 'NONE',  ( 0.000000000000000000, 0.000000000000000000, 1.000000000000000000 ) ) ;
#43900 = DIRECTION ( 'NONE',  ( 0.000000000000000000, 0.000000000000000000, 1.000000000000000000 ) ) ;
#43901 = AXIS2_PLACEMENT_3D ( 'NONE', #34199, #82655, #24368 ) ;
#43902 = DIRECTION ( 'NONE',  ( 0.000000000000000000, 0.000000000000000000, -1.000000000000000000 ) ) ;
#43903 = DIRECTION ( 'NONE',  ( -0.000000000000000000, 1.000000000000000000, -0.000000000000000000 ) ) ;
#43904 = CARTESIAN_POINT ( 'NONE',  ( 4.199999999999938005, 2.500000000000000000, 4.330127018922196314 ) ) ;
#43905 = EDGE_LOOP ( 'NONE', ( #120599, #10326, #105791, #2504 ) ) ;
#43906 = CARTESIAN_POINT ( 'NONE',  ( 12.29999999999990656, 12.50000000000000000, 4.048810130592458201 ) ) ;
#43907 = CARTESIAN_POINT ( 'NONE',  ( -5.200000000000025935, 2.500000000000000000, -3.983716857408426293 ) ) ;
#43908 = FACE_OUTER_BOUND ( 'NONE', #11185, .T. ) ;
#43909 = VECTOR ( 'NONE', #62940, 1000.000000000000000 ) ;
#43910 = DIRECTION ( 'NONE',  ( 0.000000000000000000, 0.000000000000000000, 1.000000000000000000 ) ) ;
#43912 = EDGE_CURVE ( 'NONE', #67896, #111941, #129483, .T. ) ;
#43911 = AXIS2_PLACEMENT_3D ( 'NONE', #66907, #6677, #46004 ) ;
#43913 = ORIENTED_EDGE ( 'NONE', *, *, #96978, .T. ) ;
#43914 = AXIS2_PLACEMENT_3D ( 'NONE', #44578, #113309, #54384 ) ;
#43915 = EDGE_LOOP ( 'NONE', ( #90796, #126629 ) ) ;
#43916 = ORIENTED_EDGE ( 'NONE', *, *, #95965, .T. ) ;
#43917 = CARTESIAN_POINT ( 'NONE',  ( -1.650000000000035660, 2.500000000000000000, 7.188010851410848723 ) ) ;
#43918 = AXIS2_PLACEMENT_3D ( 'NONE', #127693, #38704, #39347 ) ;
#43919 = VECTOR ( 'NONE', #53102, 1000.000000000000000 ) ;
#43920 = CARTESIAN_POINT ( 'NONE',  ( -8.350000000000013856, 2.500000000000000000, -2.165063509461101710 ) ) ;
#43921 = DIRECTION ( 'NONE',  ( 0.000000000000000000, -0.9999939076577903929, 0.003490651415223739937 ) ) ;
#43922 = VECTOR ( 'NONE', #17011, 1000.000000000000000 ) ;
#43924 = ORIENTED_EDGE ( 'NONE', *, *, #91665, .F. ) ;
#43923 = ADVANCED_FACE ( 'NONE', ( #79080 ), #68061, .T. ) ;
#43925 = FACE_OUTER_BOUND ( 'NONE', #31861, .T. ) ;
#43926 = DIRECTION ( 'NONE',  ( -0.000000000000000000, -1.000000000000000000, -0.000000000000000000 ) ) ;
#43927 = CARTESIAN_POINT ( 'NONE',  ( -7.300000000000014921, 12.50000000000000000, 4.676537180435972552 ) ) ;
#43928 = EDGE_CURVE ( 'NONE', #65883, #101366, #79703, .T. ) ;
#43929 = CARTESIAN_POINT ( 'NONE',  ( -4.800000000000022915, 2.500000000000000000, 3.883716857408420431 ) ) ;
#43930 = LINE ( 'NONE', #104130, #41529 ) ;
#43931 = ORIENTED_EDGE ( 'NONE', *, *, #27415, .T. ) ;
#43932 = EDGE_LOOP ( 'NONE', ( #107672, #9610, #69110, #103101 ) ) ;
#43933 = EDGE_CURVE ( 'NONE', #3855, #12513, #15730, .T. ) ;
#43934 = DIRECTION ( 'NONE',  ( -1.000000000000000000, 0.000000000000000000, 0.000000000000000000 ) ) ;
#43935 = DIRECTION ( 'NONE',  ( 0.000000000000000000, -0.9999939076577903929, 0.003490651415223739937 ) ) ;
#43936 = CARTESIAN_POINT ( 'NONE',  ( -3.550000000000028688, 12.50000000000000000, 6.841600689897072485 ) ) ;
#43937 = CARTESIAN_POINT ( 'NONE',  ( -5.650000000000019895, 2.500000000000000000, 1.818653347947321475 ) ) ;
#43938 = CARTESIAN_POINT ( 'NONE',  ( 194.5000000000000000, 0.000000000000000000, 0.000000000000000000 ) ) ;
#43939 = ORIENTED_EDGE ( 'NONE', *, *, #115017, .T. ) ;
#43940 = ORIENTED_EDGE ( 'NONE', *, *, #82073, .F. ) ;
#43942 = CIRCLE ( 'NONE', #85773, 0.1000000000000000472 ) ;
#43941 = DIRECTION ( 'NONE',  ( -0.000000000000000000, 1.000000000000000000, -0.000000000000000000 ) ) ;
#43943 = FACE_OUTER_BOUND ( 'NONE', #55128, .T. ) ;
#43944 = DIRECTION ( 'NONE',  ( 0.000000000000000000, 0.000000000000000000, -1.000000000000000000 ) ) ;
#43945 = CARTESIAN_POINT ( 'NONE',  ( -10.85000000000000142, 12.50000000000000000, -7.253104124594887736 ) ) ;
#43946 = ORIENTED_EDGE ( 'NONE', *, *, #45927, .F. ) ;
#43947 = CARTESIAN_POINT ( 'NONE',  ( -12.49999999999999467, 2.500000000000000000, -3.637306695894647390 ) ) ;
#43948 = AXIS2_PLACEMENT_3D ( 'NONE', #10747, #40248, #80167 ) ;
#43949 = DIRECTION ( 'NONE',  ( -0.000000000000000000, -1.000000000000000000, -0.000000000000000000 ) ) ;
#43950 = ORIENTED_EDGE ( 'NONE', *, *, #14789, .T. ) ;
#43951 = DIRECTION ( 'NONE',  ( 0.000000000000000000, 0.000000000000000000, 1.000000000000000000 ) ) ;
#43952 = EDGE_LOOP ( 'NONE', ( #101332, #116123, #56649, #88820 ) ) ;
#43953 = DIRECTION ( 'NONE',  ( 0.000000000000000000, 1.000000000000000000, 0.000000000000000000 ) ) ;
#43954 = EDGE_CURVE ( 'NONE', #56674, #125960, #128740, .T. ) ;
#43955 = ORIENTED_EDGE ( 'NONE', *, *, #70427, .T. ) ;
#43956 = DIRECTION ( 'NONE',  ( 0.000000000000000000, 0.000000000000000000, 1.000000000000000000 ) ) ;
#43957 = DIRECTION ( 'NONE',  ( 0.000000000000000000, -0.000000000000000000, 1.000000000000000000 ) ) ;
#43958 = ORIENTED_EDGE ( 'NONE', *, *, #79617, .F. ) ;
#43959 = ORIENTED_EDGE ( 'NONE', *, *, #66517, .T. ) ;
#43960 = EDGE_CURVE ( 'NONE', #86305, #48204, #11629, .T. ) ;
#43961 = CARTESIAN_POINT ( 'NONE',  ( 185.7968750003414300, 8.734944146203032389, 5.348610694689227483E-16 ) ) ;
#43962 = FACE_OUTER_BOUND ( 'NONE', #89837, .T. ) ;
#43963 = ADVANCED_FACE ( 'NONE', ( #1775 ), #97318, .T. ) ;
#43964 = CARTESIAN_POINT ( 'NONE',  ( -4.293440603042597559E-14, 2.500000000000000000, 5.022947341949748790 ) ) ;
#43965 = CARTESIAN_POINT ( 'NONE',  ( 185.9843750003414016, -8.734944146203032389, -1.604583208406767949E-15 ) ) ;
#43966 = CARTESIAN_POINT ( 'NONE',  ( -0.4000000000000396572, 12.50000000000000000, 3.637306695894644726 ) ) ;
#43967 = DIRECTION ( 'NONE',  ( -0.000000000000000000, 1.000000000000000000, -0.000000000000000000 ) ) ;
#43968 = EDGE_CURVE ( 'NONE', #122097, #88713, #122858, .T. ) ;
#43969 = ADVANCED_FACE ( 'NONE', ( #81630 ), #12872, .T. ) ;
#43970 = CARTESIAN_POINT ( 'NONE',  ( -5.600000000000020073, 12.50000000000000000, -0.2813168883297408329 ) ) ;
#43971 = CARTESIAN_POINT ( 'NONE',  ( 0.1999999999999567124, 2.500000000000000000, -3.983716857408426293 ) ) ;
#43972 = EDGE_CURVE ( 'NONE', #64387, #97052, #12240, .T. ) ;
#43973 = EDGE_CURVE ( 'NONE', #11990, #62008, #31267, .T. ) ;
#43974 = CONICAL_SURFACE ( 'NONE', #23037, 0.09999999999999982514, 0.003490658503988666988 ) ;
#43975 = AXIS2_PLACEMENT_3D ( 'NONE', #94520, #55886, #74250 ) ;
#43976 = VERTEX_POINT ( 'NONE', #82296 ) ;
#43977 = ORIENTED_EDGE ( 'NONE', *, *, #23867, .T. ) ;
#43978 = DIRECTION ( 'NONE',  ( 0.000000000000000000, 0.000000000000000000, -1.000000000000000000 ) ) ;
#43979 = EDGE_CURVE ( 'NONE', #39644, #15846, #51553, .T. ) ;
#43980 = EDGE_LOOP ( 'NONE', ( #16245, #17508 ) ) ;
#43981 = DIRECTION ( 'NONE',  ( -0.000000000000000000, 1.000000000000000000, -0.000000000000000000 ) ) ;
#43982 = DIRECTION ( 'NONE',  ( 0.000000000000000000, -0.000000000000000000, 1.000000000000000000 ) ) ;
#43983 = LINE ( 'NONE', #74074, #906 ) ;
#43985 = ORIENTED_EDGE ( 'NONE', *, *, #66804, .F. ) ;
#43984 = EDGE_LOOP ( 'NONE', ( #126065, #91114, #60230, #91180 ) ) ;
#43986 = FACE_BOUND ( 'NONE', #102002, .T. ) ;
#43987 = EDGE_LOOP ( 'NONE', ( #10537, #100154 ) ) ;
#43988 = DIRECTION ( 'NONE',  ( 0.000000000000000000, 0.000000000000000000, -1.000000000000000000 ) ) ;
#43989 = PLANE ( 'NONE',  #112622 ) ;
#43991 = ADVANCED_FACE ( 'NONE', ( #90147 ), #126568, .T. ) ;
#43990 = CIRCLE ( 'NONE', #69009, 0.06509327318403741736 ) ;
#43992 = VERTEX_POINT ( 'NONE', #20149 ) ;
#43993 = DIRECTION ( 'NONE',  ( 0.000000000000000000, 0.000000000000000000, 1.000000000000000000 ) ) ;
#43994 = LINE ( 'NONE', #123812, #114228 ) ;
#43995 = DIRECTION ( 'NONE',  ( -0.000000000000000000, 1.000000000000000000, -0.000000000000000000 ) ) ;
#43996 = DIRECTION ( 'NONE',  ( -0.000000000000000000, -1.000000000000000000, -0.000000000000000000 ) ) ;
#43997 = CARTESIAN_POINT ( 'NONE',  ( -5.850000000000022737, 2.500000000000000000, -6.495190528383302464 ) ) ;
#43998 = FACE_OUTER_BOUND ( 'NONE', #15073, .T. ) ;
#43999 = DIRECTION ( 'NONE',  ( 0.000000000000000000, 0.000000000000000000, 1.000000000000000000 ) ) ;
#44000 = DIRECTION ( 'NONE',  ( 0.000000000000000000, 0.000000000000000000, 1.000000000000000000 ) ) ;
#44001 = DIRECTION ( 'NONE',  ( 0.000000000000000000, 0.000000000000000000, 1.000000000000000000 ) ) ;
#44002 = CIRCLE ( 'NONE', #58664, 0.06509327318403745899 ) ;
#44003 = ORIENTED_EDGE ( 'NONE', *, *, #26639, .T. ) ;
#44004 = ORIENTED_EDGE ( 'NONE', *, *, #90348, .T. ) ;
#44005 = VECTOR ( 'NONE', #73870, 1000.000000000000000 ) ;
#44006 = ORIENTED_EDGE ( 'NONE', *, *, #43299, .F. ) ;
#44007 = FACE_OUTER_BOUND ( 'NONE', #88919, .T. ) ;
#44008 = ORIENTED_EDGE ( 'NONE', *, *, #32768, .T. ) ;
#44010 = ORIENTED_EDGE ( 'NONE', *, *, #120975, .F. ) ;
#44009 = ORIENTED_EDGE ( 'NONE', *, *, #5950, .F. ) ;
#44011 = ORIENTED_EDGE ( 'NONE', *, *, #24324, .F. ) ;
#44012 = DIRECTION ( 'NONE',  ( 0.000000000000000000, 0.000000000000000000, 1.000000000000000000 ) ) ;
#44013 = AXIS2_PLACEMENT_3D ( 'NONE', #94965, #25547, #65484 ) ;
#44014 = DIRECTION ( 'NONE',  ( 0.000000000000000000, -0.000000000000000000, 1.000000000000000000 ) ) ;
#44015 =( NAMED_UNIT ( * ) PLANE_ANGLE_UNIT ( ) SI_UNIT ( $, .RADIAN. ) );
#44016 = DIRECTION ( 'NONE',  ( 0.000000000000000000, -0.000000000000000000, 1.000000000000000000 ) ) ;
#44017 = AXIS2_PLACEMENT_3D ( 'NONE', #83083, #25251, #27199 ) ;
#44018 = DIRECTION ( 'NONE',  ( 0.000000000000000000, 1.000000000000000000, 0.000000000000000000 ) ) ;
#44019 = FACE_OUTER_BOUND ( 'NONE', #114490, .T. ) ;
#44020 = ORIENTED_EDGE ( 'NONE', *, *, #92500, .T. ) ;
#44021 = CARTESIAN_POINT ( 'NONE',  ( -8.750000000000005329, 12.50000000000000000, 5.802370205355744659 ) ) ;
#44022 = ORIENTED_EDGE ( 'NONE', *, *, #42527, .F. ) ;
#44023 = EDGE_LOOP ( 'NONE', ( #27014, #113373, #10610, #94292 ) ) ;
#44024 = ADVANCED_FACE ( 'NONE', ( #31903 ), #70138, .T. ) ;
#44025 = ORIENTED_EDGE ( 'NONE', *, *, #48495, .F. ) ;
#44026 = DIRECTION ( 'NONE',  ( -0.000000000000000000, 1.000000000000000000, -0.000000000000000000 ) ) ;
#44027 = ORIENTED_EDGE ( 'NONE', *, *, #46477, .T. ) ;
#44028 = VERTEX_POINT ( 'NONE', #101930 ) ;
#44029 = VERTEX_POINT ( 'NONE', #3090 ) ;
#44030 = EDGE_CURVE ( 'NONE', #25747, #63089, #40908, .T. ) ;
#44031 = DIRECTION ( 'NONE',  ( 0.000000000000000000, 0.000000000000000000, 1.000000000000000000 ) ) ;
#44032 = DIRECTION ( 'NONE',  ( 0.000000000000000000, 0.000000000000000000, 1.000000000000000000 ) ) ;
#44033 = DIRECTION ( 'NONE',  ( -0.000000000000000000, -1.000000000000000000, -0.000000000000000000 ) ) ;
#44034 = CARTESIAN_POINT ( 'NONE',  ( -8.750000000000012434, 2.500000000000000000, -5.802370205355744659 ) ) ;
#44035 = CONICAL_SURFACE ( 'NONE', #52332, 0.1000000000000002554, 0.003490658503988666988 ) ;
#44036 = DIRECTION ( 'NONE',  ( 0.000000000000000000, -0.000000000000000000, 1.000000000000000000 ) ) ;
#44037 = PLANE ( 'NONE',  #45049 ) ;
#44038 = ORIENTED_EDGE ( 'NONE', *, *, #36256, .F. ) ;
#44039 = DIRECTION ( 'NONE',  ( 0.000000000000000000, -0.000000000000000000, 1.000000000000000000 ) ) ;
#44040 = ORIENTED_EDGE ( 'NONE', *, *, #104818, .F. ) ;
#44041 = CARTESIAN_POINT ( 'NONE',  ( -9.550000000000006040, 2.500000000000000000, 2.165063509461097713 ) ) ;
#44042 = ORIENTED_EDGE ( 'NONE', *, *, #112270, .T. ) ;
#44043 = EDGE_LOOP ( 'NONE', ( #20200, #75284, #28800, #91552 ) ) ;
#44044 = DIRECTION ( 'NONE',  ( 0.000000000000000000, -0.9999939076577903929, 0.003490651415223739937 ) ) ;
#44045 = CARTESIAN_POINT ( 'NONE',  ( 0.8499999999999553468, 2.500000000000000000, -2.757883832488654097 ) ) ;
#44046 = DIRECTION ( 'NONE',  ( -0.000000000000000000, 1.000000000000000000, -0.000000000000000000 ) ) ;
#44047 = VERTEX_POINT ( 'NONE', #91455 ) ;
#44048 = EDGE_LOOP ( 'NONE', ( #1563, #13483, #68018, #117687 ) ) ;
#44049 = FACE_OUTER_BOUND ( 'NONE', #44727, .T. ) ;
#44050 = CARTESIAN_POINT ( 'NONE',  ( 2.500000000000002220, -1.500000000000000000, -9.999999999999998224 ) ) ;
#44051 = DIRECTION ( 'NONE',  ( -0.000000000000000000, -1.000000000000000000, -0.000000000000000000 ) ) ;
#44052 = CARTESIAN_POINT ( 'NONE',  ( 8.749999999999921840, 12.50000000000000000, -5.867463478539787225 ) ) ;
#44053 = FACE_OUTER_BOUND ( 'NONE', #86400, .T. ) ;
#44054 = EDGE_CURVE ( 'NONE', #6303, #97052, #13677, .T. ) ;
#44055 = EDGE_LOOP ( 'NONE', ( #24621, #53521, #112740, #48278 ) ) ;
#44056 = EDGE_LOOP ( 'NONE', ( #110938, #94469 ) ) ;
#44057 = CARTESIAN_POINT ( 'NONE',  ( 187.4609375001707008, 0.000000000000000000, 7.632341765625000107 ) ) ;
#44058 = CONICAL_SURFACE ( 'NONE', #79649, 0.1000000000000002554, 0.003490658503988666988 ) ;
#44060 = EDGE_CURVE ( 'NONE', #123049, #109667, #120304, .T. ) ;
#44059 = FACE_OUTER_BOUND ( 'NONE', #73458, .T. ) ;
#44061 = AXIS2_PLACEMENT_3D ( 'NONE', #109199, #111119, #101337 ) ;
#44062 = EDGE_CURVE ( 'NONE', #36337, #126006, #30437, .T. ) ;
#44063 = CARTESIAN_POINT ( 'NONE',  ( 185.3385416670080872, 6.551208109652274736, 3.782341765625001351 ) ) ;
#44064 = CARTESIAN_POINT ( 'NONE',  ( 13.09999999999990195, 2.500000000000000000, -3.883716857408426648 ) ) ;
#44065 = DIRECTION ( 'NONE',  ( 0.000000000000000000, 1.000000000000000000, 0.000000000000000000 ) ) ;
#44066 = DIRECTION ( 'NONE',  ( -0.000000000000000000, 1.000000000000000000, -0.000000000000000000 ) ) ;
#44067 = EDGE_CURVE ( 'NONE', #51768, #13612, #49222, .T. ) ;
#44068 = LINE ( 'NONE', #122633, #122848 ) ;
#44069 = EDGE_LOOP ( 'NONE', ( #117088, #6917 ) ) ;
#44070 = AXIS2_PLACEMENT_3D ( 'NONE', #109767, #111025, #39760 ) ;
#44071 = DIRECTION ( 'NONE',  ( -0.000000000000000000, -1.000000000000000000, -0.000000000000000000 ) ) ;
#44072 = FACE_OUTER_BOUND ( 'NONE', #123039, .T. ) ;
#44073 = CARTESIAN_POINT ( 'NONE',  ( 4.599999999999939249, 2.500000000000000000, -3.537306695894649966 ) ) ;
#44074 = EDGE_CURVE ( 'NONE', #4260, #118169, #120285, .T. ) ;
#44075 = ORIENTED_EDGE ( 'NONE', *, *, #32174, .F. ) ;
#44076 = EDGE_CURVE ( 'NONE', #98404, #85026, #22124, .T. ) ;
#44077 = CARTESIAN_POINT ( 'NONE',  ( -13.54999999999999005, 12.50000000000000000, -1.753560074763286458 ) ) ;
#44078 = CIRCLE ( 'NONE', #64986, 0.06509327318403743123 ) ;
#44079 = EDGE_LOOP ( 'NONE', ( #12797, #84608 ) ) ;
#44080 = B_SPLINE_CURVE_WITH_KNOTS ( 'NONE', 3,
 ( #47520, #87423, #127368, #37698, #77599, #67789, #97890, #91300, #110926, #109660, #59935, #71026 ),
 .UNSPECIFIED., .F., .F.,
 ( 4, 2, 2, 2, 2, 4 ),
 ( 0.000000000000000000, 0.001866281188413360234, 0.003732562376826720468, 0.005598843565240080485, 0.006531984159446760710, 0.007465124753653440935 ),
 .UNSPECIFIED. ) ;
#44081 = DIRECTION ( 'NONE',  ( 0.000000000000000000, 0.000000000000000000, -1.000000000000000000 ) ) ;
#44082 = VERTEX_POINT ( 'NONE', #100618 ) ;
#44083 = CARTESIAN_POINT ( 'NONE',  ( -8.749999999999971578, 2.500000000000000000, 6.495190528383297135 ) ) ;
#44084 = DIRECTION ( 'NONE',  ( -0.000000000000000000, -1.000000000000000000, -0.000000000000000000 ) ) ;
#44085 = DIRECTION ( 'NONE',  ( 0.000000000000000000, 0.000000000000000000, -1.000000000000000000 ) ) ;
#44086 = AXIS2_PLACEMENT_3D ( 'NONE', #65326, #45713, #116364 ) ;
#44087 = ORIENTED_EDGE ( 'NONE', *, *, #106889, .T. ) ;
#44088 = DIRECTION ( 'NONE',  ( -4.274815082592931898E-19, -0.9999939076577903929, -0.003490651415223739937 ) ) ;
#44089 = CARTESIAN_POINT ( 'NONE',  ( 8.549999999999924327, 12.50000000000000000, -6.906693963081115051 ) ) ;
#44090 = CIRCLE ( 'NONE', #48298, 0.06509327318403745899 ) ;
#44091 = ORIENTED_EDGE ( 'NONE', *, *, #33166, .F. ) ;
#44092 = DIRECTION ( 'NONE',  ( -0.000000000000000000, -1.000000000000000000, -0.000000000000000000 ) ) ;
#44093 = ORIENTED_EDGE ( 'NONE', *, *, #112351, .T. ) ;
#44094 = ORIENTED_EDGE ( 'NONE', *, *, #55033, .T. ) ;
#44095 = DIRECTION ( 'NONE',  ( 0.000000000000000000, 1.000000000000000000, 0.000000000000000000 ) ) ;
#44096 = DIRECTION ( 'NONE',  ( -0.000000000000000000, -1.000000000000000000, -0.000000000000000000 ) ) ;
#44097 = DIRECTION ( 'NONE',  ( 0.000000000000000000, 0.000000000000000000, 1.000000000000000000 ) ) ;
#44098 = EDGE_LOOP ( 'NONE', ( #67815, #920 ) ) ;
#44099 = CARTESIAN_POINT ( 'NONE',  ( -2.900000000000030109, 12.50000000000000000, 0.7579135962115869374 ) ) ;
#44100 = DIRECTION ( 'NONE',  ( -0.000000000000000000, -1.000000000000000000, -0.000000000000000000 ) ) ;
#44101 = ORIENTED_EDGE ( 'NONE', *, *, #64327, .F. ) ;
#44102 = EDGE_CURVE ( 'NONE', #124893, #45024, #80998, .T. ) ;
#44103 = CARTESIAN_POINT ( 'NONE',  ( -11.05000000000000071, 12.50000000000000000, -6.841600689897075149 ) ) ;
#44104 = FACE_OUTER_BOUND ( 'NONE', #33516, .T. ) ;
#44107 = EDGE_CURVE ( 'NONE', #30037, #56648, #111072, .T. ) ;
#44106 = CARTESIAN_POINT ( 'NONE',  ( 12.49999999999990408, 2.500000000000000000, -3.737306695894649700 ) ) ;
#44105 = VECTOR ( 'NONE', #49199, 1000.000000000000000 ) ;
#44108 = CARTESIAN_POINT ( 'NONE',  ( -12.49999999999999289, 12.50000000000000000, -5.022947341949751454 ) ) ;
#44109 = CARTESIAN_POINT ( 'NONE',  ( -2.900000000000029665, 12.50000000000000000, 4.330127018922196314 ) ) ;
#44110 = VECTOR ( 'NONE', #17272, 1000.000000000000000 ) ;
#44111 = EDGE_CURVE ( 'NONE', #96649, #53518, #122368, .T. ) ;
#44112 = AXIS2_PLACEMENT_3D ( 'NONE', #118222, #28562, #118870 ) ;
#44113 = CARTESIAN_POINT ( 'NONE',  ( 0.8499999999999545697, 12.50000000000000000, 2.792790559304612064 ) ) ;
#44114 = DIRECTION ( 'NONE',  ( 0.000000000000000000, 0.000000000000000000, -1.000000000000000000 ) ) ;
#44115 = ADVANCED_FACE ( 'NONE', ( #124136 ), #63867, .T. ) ;
#44116 = EDGE_CURVE ( 'NONE', #39602, #103467, #28371, .T. ) ;
#44117 = CIRCLE ( 'NONE', #85953, 0.09999999999999982514 ) ;
#44118 = VERTEX_POINT ( 'NONE', #73113 ) ;
#44119 = ORIENTED_EDGE ( 'NONE', *, *, #69206, .F. ) ;
#44121 = ORIENTED_EDGE ( 'NONE', *, *, #3762, .F. ) ;
#44120 = ADVANCED_FACE ( 'NONE', ( #103865 ), #51363, .T. ) ;
#44122 = ORIENTED_EDGE ( 'NONE', *, *, #98033, .F. ) ;
#44123 = CARTESIAN_POINT ( 'NONE',  ( 26.74601813931273853, 2.978655629156508944, 2.722801754518484163 ) ) ;
#44124 = DIRECTION ( 'NONE',  ( 0.000000000000000000, 1.000000000000000000, 0.000000000000000000 ) ) ;
#44125 = DIRECTION ( 'NONE',  ( -0.000000000000000000, -1.000000000000000000, -0.000000000000000000 ) ) ;
#44126 = ORIENTED_EDGE ( 'NONE', *, *, #101129, .F. ) ;
#44127 = FACE_BOUND ( 'NONE', #119524, .T. ) ;
#44128 = CARTESIAN_POINT ( 'NONE',  ( 4.149999999999938183, 12.50000000000000000, 7.122917578226811486 ) ) ;
#44129 = DIRECTION ( 'NONE',  ( 0.000000000000000000, 1.000000000000000000, 0.000000000000000000 ) ) ;
#44130 = ADVANCED_FACE ( 'NONE', ( #65198 ), #105135, .T. ) ;
#44131 = DIRECTION ( 'NONE',  ( 0.000000000000000000, 0.000000000000000000, 1.000000000000000000 ) ) ;
#44132 = EDGE_CURVE ( 'NONE', #129137, #119917, #101524, .T. ) ;
#44133 = DIRECTION ( 'NONE',  ( -0.000000000000000000, 1.000000000000000000, -0.000000000000000000 ) ) ;
#44134 = DIRECTION ( 'NONE',  ( 0.9974916312695811804, -0.05217691604167136454, 0.04783319955355744973 ) ) ;
#44135 = CARTESIAN_POINT ( 'NONE',  ( 1.899999999999949507, 2.500000000000000000, 3.983716857408420964 ) ) ;
#44136 = CARTESIAN_POINT ( 'NONE',  ( 11.44999999999990514, 2.500000000000000000, -6.248780366869526759 ) ) ;
#44137 = CARTESIAN_POINT ( 'NONE',  ( 12.69999999999989981, 2.500000000000000000, -0.2464101615137783419 ) ) ;
#44138 = DIRECTION ( 'NONE',  ( -0.000000000000000000, -1.000000000000000000, -0.000000000000000000 ) ) ;
#44139 = CARTESIAN_POINT ( 'NONE',  ( -7.100000000000018296, 2.500000000000000000, 0.09999999999999761857 ) ) ;
#44140 = EDGE_LOOP ( 'NONE', ( #40686, #2796 ) ) ;
#44141 = CIRCLE ( 'NONE', #12728, 0.06509327318403745899 ) ;
#44142 = VERTEX_POINT ( 'NONE', #23343 ) ;
#44143 = ORIENTED_EDGE ( 'NONE', *, *, #22671, .T. ) ;
#44144 = ORIENTED_EDGE ( 'NONE', *, *, #72496, .T. ) ;
#44145 = ORIENTED_EDGE ( 'NONE', *, *, #102534, .T. ) ;
#44146 = ORIENTED_EDGE ( 'NONE', *, *, #19203, .T. ) ;
#44147 = CARTESIAN_POINT ( 'NONE',  ( 2.500000000000002220, 1.500000000000000444, -9.999999999999998224 ) ) ;
#44148 = EDGE_LOOP ( 'NONE', ( #95281, #71893, #75324, #74533 ) ) ;
#44149 = ORIENTED_EDGE ( 'NONE', *, *, #126202, .T. ) ;
#44150 = CIRCLE ( 'NONE', #119357, 0.1000000000000002554 ) ;
#44151 = AXIS2_PLACEMENT_3D ( 'NONE', #40989, #40334, #21311 ) ;
#44152 = DIRECTION ( 'NONE',  ( 0.000000000000000000, 1.000000000000000000, 0.000000000000000000 ) ) ;
#44153 = CARTESIAN_POINT ( 'NONE',  ( 9.349999999999916156, 2.500000000000000000, 6.248780366869520542 ) ) ;
#44154 = DIRECTION ( 'NONE',  ( 0.000000000000000000, 1.000000000000000000, 0.000000000000000000 ) ) ;
#44155 = DIRECTION ( 'NONE',  ( 0.000000000000000000, 1.000000000000000000, 0.000000000000000000 ) ) ;
#44156 = ORIENTED_EDGE ( 'NONE', *, *, #106463, .T. ) ;
#44157 = LINE ( 'NONE', #127709, #10913 ) ;
#44158 = AXIS2_PLACEMENT_3D ( 'NONE', #124737, #80089, #112133 ) ;
#44159 = CIRCLE ( 'NONE', #56659, 0.1000000000000002554 ) ;
#44160 = EDGE_LOOP ( 'NONE', ( #6944, #79268 ) ) ;
#44161 = ORIENTED_EDGE ( 'NONE', *, *, #48272, .T. ) ;
#44163 = ORIENTED_EDGE ( 'NONE', *, *, #114205, .T. ) ;
#44162 = CARTESIAN_POINT ( 'NONE',  ( -11.24999999999996270, 12.50000000000000000, 6.495190528383297135 ) ) ;
#44164 = PLANE ( 'NONE',  #52539 ) ;
#44165 = ORIENTED_EDGE ( 'NONE', *, *, #68161, .T. ) ;
#44166 = CIRCLE ( 'NONE', #39978, 0.06509327318403745899 ) ;
#44167 = DIRECTION ( 'NONE',  ( 1.000000000000000000, 0.000000000000000000, 0.000000000000000000 ) ) ;
#44168 = EDGE_CURVE ( 'NONE', #119345, #23310, #116093, .T. ) ;
#44169 = FACE_OUTER_BOUND ( 'NONE', #116361, .T. ) ;
#44170 = CARTESIAN_POINT ( 'NONE',  ( -4.350000000000023626, 2.500000000000000000, -1.818653347947325916 ) ) ;
#44171 = CARTESIAN_POINT ( 'NONE',  ( 8.549999999999924327, 2.500000000000000000, 1.918653347947321564 ) ) ;
#44172 = DIRECTION ( 'NONE',  ( 1.000000000000000000, 0.000000000000000000, 0.000000000000000000 ) ) ;
#44173 = ORIENTED_EDGE ( 'NONE', *, *, #80200, .F. ) ;
#44174 = DIRECTION ( 'NONE',  ( 0.000000000000000000, 1.000000000000000000, 0.000000000000000000 ) ) ;
#44175 = EDGE_LOOP ( 'NONE', ( #50268, #50582, #52858, #85813 ) ) ;
#44176 = DIRECTION ( 'NONE',  ( 0.000000000000000000, -0.000000000000000000, 1.000000000000000000 ) ) ;
#44177 = EDGE_LOOP ( 'NONE', ( #88073, #11647 ) ) ;
#44178 = CARTESIAN_POINT ( 'NONE',  ( 0.8499999999999536815, 2.500000000000000000, 6.495190528383297135 ) ) ;
#44179 = CIRCLE ( 'NONE', #25382, 0.09999999999999982514 ) ;
#44180 = AXIS2_PLACEMENT_3D ( 'NONE', #122272, #100046, #109869 ) ;
#44181 = CARTESIAN_POINT ( 'NONE',  ( 13.14999999999989733, 2.500000000000000000, -2.411473670974877859 ) ) ;
#44182 = PLANE ( 'NONE',  #27910 ) ;
#44183 = DIRECTION ( 'NONE',  ( 0.000000000000000000, 0.000000000000000000, 1.000000000000000000 ) ) ;
#44184 = ORIENTED_EDGE ( 'NONE', *, *, #116187, .F. ) ;
#44185 = CARTESIAN_POINT ( 'NONE',  ( -1.850000000000033396, 12.50000000000000000, -6.841600689897077814 ) ) ;
#44186 = DIRECTION ( 'NONE',  ( -0.000000000000000000, 1.000000000000000000, -0.000000000000000000 ) ) ;
#44187 = EDGE_LOOP ( 'NONE', ( #4586, #67011 ) ) ;
#44188 = EDGE_LOOP ( 'NONE', ( #114230, #103848 ) ) ;
#44189 = EDGE_LOOP ( 'NONE', ( #26878, #30303, #96992, #79638 ) ) ;
#44190 = DIRECTION ( 'NONE',  ( 0.000000000000000000, 0.000000000000000000, -1.000000000000000000 ) ) ;
#44191 = CARTESIAN_POINT ( 'NONE',  ( -12.49999999999999289, 2.500000000000000000, 5.022947341949748790 ) ) ;
#44192 = CARTESIAN_POINT ( 'NONE',  ( 185.9427083336747160, -6.551208109652278289, 3.782341765624995134 ) ) ;
#44193 = DIRECTION ( 'NONE',  ( -0.000000000000000000, -1.000000000000000000, -0.000000000000000000 ) ) ;
#44194 = DIRECTION ( 'NONE',  ( 0.000000000000000000, 0.000000000000000000, 1.000000000000000000 ) ) ;
#44195 = FACE_OUTER_BOUND ( 'NONE', #98904, .T. ) ;
#44196 = AXIS2_PLACEMENT_3D ( 'NONE', #115006, #34559, #96029 ) ;
#44197 = CONICAL_SURFACE ( 'NONE', #102684, 0.09999999999999999167, 0.003490658503988666988 ) ;
#44198 = VECTOR ( 'NONE', #85389, 1000.000000000000000 ) ;
#44199 = ORIENTED_EDGE ( 'NONE', *, *, #40725, .T. ) ;
#44200 = DIRECTION ( 'NONE',  ( 0.000000000000000000, 0.000000000000000000, -1.000000000000000000 ) ) ;
#44201 = EDGE_CURVE ( 'NONE', #3627, #61342, #104496, .T. ) ;
#44202 = AXIS2_PLACEMENT_3D ( 'NONE', #12358, #52296, #122337 ) ;
#44203 = AXIS2_PLACEMENT_3D ( 'NONE', #25970, #65881, #36450 ) ;
#44204 = VERTEX_POINT ( 'NONE', #84858 ) ;
#44205 = CIRCLE ( 'NONE', #37953, 0.1000000000000002554 ) ;
#44206 = ADVANCED_FACE ( 'NONE', ( #124791 ), #61919, .T. ) ;
#44207 = LINE ( 'NONE', #65124, #34964 ) ;
#44208 = CARTESIAN_POINT ( 'NONE',  ( -3.950000000000026379, 2.500000000000000000, -1.718653347947326049 ) ) ;
#44209 = CARTESIAN_POINT ( 'NONE',  ( 4.549999999999935874, 12.50000000000000000, 6.430097255199259010 ) ) ;
#44210 = EDGE_CURVE ( 'NONE', #40177, #104598, #35764, .T. ) ;
#44211 = ORIENTED_EDGE ( 'NONE', *, *, #75384, .F. ) ;
#44212 = CARTESIAN_POINT ( 'NONE',  ( -11.44999999999999751, 2.500000000000000000, 1.818653347947321475 ) ) ;
#44213 = DIRECTION ( 'NONE',  ( -0.000000000000000000, -1.000000000000000000, -0.000000000000000000 ) ) ;
#44214 = ADVANCED_FACE ( 'NONE', ( #53481 ), #126659, .T. ) ;
#44215 = ADVANCED_FACE ( 'NONE', ( #115593 ), #99477, .T. ) ;
#44216 = ADVANCED_FACE ( 'NONE', ( #3716 ), #26319, .T. ) ;
#44217 = EDGE_CURVE ( 'NONE', #86499, #58259, #45593, .T. ) ;
#44218 = EDGE_CURVE ( 'NONE', #100973, #50751, #118332, .T. ) ;
#44219 = VERTEX_POINT ( 'NONE', #75668 ) ;
#44220 = FACE_OUTER_BOUND ( 'NONE', #91757, .T. ) ;
#44221 = EDGE_LOOP ( 'NONE', ( #58253, #77717, #68080, #107018 ) ) ;
#44222 = ORIENTED_EDGE ( 'NONE', *, *, #50176, .T. ) ;
#44223 = DIRECTION ( 'NONE',  ( 1.000000000000000000, 0.000000000000000000, 0.000000000000000000 ) ) ;
#44224 = ADVANCED_FACE ( 'NONE', ( #113684 ), #51727, .T. ) ;
#44225 = EDGE_LOOP ( 'NONE', ( #38272, #85977, #93026, #77857 ) ) ;
#44226 = CARTESIAN_POINT ( 'NONE',  ( 16.53754090007008770, 0.4856821978169255649, -6.114873053042312989 ) ) ;
#44227 = PLANE ( 'NONE',  #77692 ) ;
#44228 = DIRECTION ( 'NONE',  ( 0.000000000000000000, 0.000000000000000000, -1.000000000000000000 ) ) ;
#44229 = AXIS2_PLACEMENT_3D ( 'NONE', #104578, #94118, #123560 ) ;
#44230 = EDGE_LOOP ( 'NONE', ( #7450, #83441 ) ) ;
#44231 = AXIS2_PLACEMENT_3D ( 'NONE', #79458, #20533, #60475 ) ;
#44232 = CARTESIAN_POINT ( 'NONE',  ( -9.150000000000005684, 2.500000000000000000, 6.495190528383297135 ) ) ;
#44234 = ORIENTED_EDGE ( 'NONE', *, *, #19158, .T. ) ;
#44233 = CARTESIAN_POINT ( 'NONE',  ( -6.650000000000018119, 2.500000000000000000, -2.165063509461101710 ) ) ;
#44235 = CARTESIAN_POINT ( 'NONE',  ( 7.699999999999923794, 2.500000000000000000, 4.576537180435972019 ) ) ;
#44236 = CARTESIAN_POINT ( 'NONE',  ( 11.24999999999990585, 2.500000000000000000, 2.857883832488649301 ) ) ;
#44237 = VECTOR ( 'NONE', #107982, 1000.000000000000000 ) ;
#44238 = EDGE_LOOP ( 'NONE', ( #37945, #119102, #8784, #48723 ) ) ;
#44239 = CIRCLE ( 'NONE', #27501, 0.06509327318403745899 ) ;
#44240 = CIRCLE ( 'NONE', #113196, 0.06509327318403745899 ) ;
#44241 = ORIENTED_EDGE ( 'NONE', *, *, #96076, .F. ) ;
#44242 = ORIENTED_EDGE ( 'NONE', *, *, #15225, .T. ) ;
#44243 = CARTESIAN_POINT ( 'NONE',  ( -5.650000000000023448, 12.50000000000000000, -2.511473670974877948 ) ) ;
#44244 = CARTESIAN_POINT ( 'NONE',  ( -3.550000000000027356, 2.500000000000000000, 1.718653347947321386 ) ) ;
#44245 = CARTESIAN_POINT ( 'NONE',  ( -13.09999999999999254, 2.500000000000000000, -4.776537180435974861 ) ) ;
#44246 = FACE_BOUND ( 'NONE', #13918, .T. ) ;
#44247 = VERTEX_POINT ( 'NONE', #76336 ) ;
#44248 = CARTESIAN_POINT ( 'NONE',  ( 186.5677083336747160, -4.367472073101514418, -7.564683531250002702 ) ) ;
#44249 = CARTESIAN_POINT ( 'NONE',  ( -1.900000000000034550, 12.50000000000000000, 4.676537180435972552 ) ) ;
#44250 = CARTESIAN_POINT ( 'NONE',  ( 0.7999999999999612976, 2.500000000000000000, 0.09999999999999989453 ) ) ;
#44251 = FACE_BOUND ( 'NONE', #102656, .T. ) ;
#44252 = AXIS2_PLACEMENT_3D ( 'NONE', #108803, #47982, #57140 ) ;
#44253 = DIRECTION ( 'NONE',  ( -0.000000000000000000, -1.000000000000000000, -0.000000000000000000 ) ) ;
#44254 = FACE_OUTER_BOUND ( 'NONE', #82646, .T. ) ;
#44255 = ADVANCED_FACE ( 'NONE', ( #66498 ), #6913, .T. ) ;
#44256 = CARTESIAN_POINT ( 'NONE',  ( -2.050000000000032685, 2.500000000000000000, -6.395190528383301931 ) ) ;
#44257 = AXIS2_PLACEMENT_3D ( 'NONE', #32384, #61167, #101088 ) ;
#44258 = EDGE_CURVE ( 'NONE', #32793, #101221, #60425, .T. ) ;
#44259 = CARTESIAN_POINT ( 'NONE',  ( 1.849999999999950573, 2.500000000000000000, -1.818653347947326138 ) ) ;
#44260 = EDGE_CURVE ( 'NONE', #69086, #20962, #105727, .T. ) ;
#44261 = ORIENTED_EDGE ( 'NONE', *, *, #13337, .F. ) ;
#44262 = AXIS2_PLACEMENT_3D ( 'NONE', #97564, #18359, #58308 ) ;
#44263 = AXIS2_PLACEMENT_3D ( 'NONE', #31166, #120175, #71071 ) ;
#44264 = VERTEX_POINT ( 'NONE', #56665 ) ;
#44265 = ORIENTED_EDGE ( 'NONE', *, *, #83602, .F. ) ;
#44266 = VERTEX_POINT ( 'NONE', #57993 ) ;
#44267 = ORIENTED_EDGE ( 'NONE', *, *, #92410, .T. ) ;
#44268 = CARTESIAN_POINT ( 'NONE',  ( -13.74999999999995381, 2.500000000000000000, 2.065063509461101621 ) ) ;
#44269 = DIRECTION ( 'NONE',  ( -0.000000000000000000, -1.000000000000000000, -0.000000000000000000 ) ) ;
#44271 = EDGE_CURVE ( 'NONE', #126312, #71812, #74429, .T. ) ;
#44270 = ORIENTED_EDGE ( 'NONE', *, *, #42162, .T. ) ;
#44272 = FACE_BOUND ( 'NONE', #12920, .T. ) ;
#44273 = PLANE ( 'NONE',  #77118 ) ;
#44274 = EDGE_CURVE ( 'NONE', #71913, #110789, #107866, .T. ) ;
#44275 = ADVANCED_FACE ( 'NONE', ( #27874 ), #109939, .T. ) ;
#44276 = EDGE_CURVE ( 'NONE', #38503, #48843, #122463, .T. ) ;
#44277 = DIRECTION ( 'NONE',  ( 0.000000000000000000, 0.000000000000000000, -1.000000000000000000 ) ) ;
#44278 = ORIENTED_EDGE ( 'NONE', *, *, #46574, .T. ) ;
#44279 = PLANE ( 'NONE',  #32841 ) ;
#44280 = DIRECTION ( 'NONE',  ( 0.000000000000000000, -0.9999939076577903929, 0.003490651415223739937 ) ) ;
#44281 = DIRECTION ( 'NONE',  ( 0.000000000000000000, 0.000000000000000000, 1.000000000000000000 ) ) ;
#44282 = ORIENTED_EDGE ( 'NONE', *, *, #72073, .F. ) ;
#44283 = CARTESIAN_POINT ( 'NONE',  ( 16.56576425164991306, -1.499999999999999334, 6.084390597445976212 ) ) ;
#44284 = EDGE_CURVE ( 'NONE', #7925, #43068, #38355, .T. ) ;
#44285 = ORIENTED_EDGE ( 'NONE', *, *, #6395, .T. ) ;
#44286 = ORIENTED_EDGE ( 'NONE', *, *, #112824, .T. ) ;
#44287 = CIRCLE ( 'NONE', #92316, 0.06509327318403745899 ) ;
#44288 = ORIENTED_EDGE ( 'NONE', *, *, #28279, .T. ) ;
#44289 = AXIS2_PLACEMENT_3D ( 'NONE', #105862, #15530, #45664 ) ;
#44290 = DIRECTION ( 'NONE',  ( 0.000000000000000000, 1.000000000000000000, 0.000000000000000000 ) ) ;
#44291 = AXIS2_PLACEMENT_3D ( 'NONE', #53215, #44676, #85860 ) ;
#44292 = DIRECTION ( 'NONE',  ( 0.000000000000000000, -0.9999939076577903929, 0.003490651415223739937 ) ) ;
#44293 = DIRECTION ( 'NONE',  ( 0.000000000000000000, 0.000000000000000000, -1.000000000000000000 ) ) ;
#44294 = ORIENTED_EDGE ( 'NONE', *, *, #31119, .F. ) ;
#44295 = DIRECTION ( 'NONE',  ( 0.000000000000000000, 0.000000000000000000, -1.000000000000000000 ) ) ;
#44296 = FACE_OUTER_BOUND ( 'NONE', #25852, .T. ) ;
#44297 = CIRCLE ( 'NONE', #19244, 0.09999999999999982514 ) ;
#44298 = AXIS2_PLACEMENT_3D ( 'NONE', #83459, #87773, #84075 ) ;
#44299 = FACE_OUTER_BOUND ( 'NONE', #98037, .T. ) ;
#44300 = CARTESIAN_POINT ( 'NONE',  ( 185.4062500006828316, -8.891194145520236347, -1.633285867636356693E-15 ) ) ;
#44301 = ORIENTED_EDGE ( 'NONE', *, *, #71009, .T. ) ;
#44302 = CIRCLE ( 'NONE', #67252, 0.1000000000000000472 ) ;
#44303 = CONICAL_SURFACE ( 'NONE', #31800, 0.09999999999999999167, 0.003490658503988666988 ) ;
#44304 = CARTESIAN_POINT ( 'NONE',  ( -9.800000000000006040, 12.50000000000000000, -4.611443907251936203 ) ) ;
#44305 = ADVANCED_FACE ( 'NONE', ( #110142 ), #47252, .T. ) ;
#44306 = EDGE_LOOP ( 'NONE', ( #23478, #104427 ) ) ;
#44307 = FACE_OUTER_BOUND ( 'NONE', #50825, .T. ) ;
#44308 = CIRCLE ( 'NONE', #35907, 0.06509327318403745899 ) ;
#44309 = EDGE_LOOP ( 'NONE', ( #71595, #31269, #125964, #14747 ) ) ;
#44310 = EDGE_LOOP ( 'NONE', ( #74762, #38418, #98445, #57228 ) ) ;
#44311 = CARTESIAN_POINT ( 'NONE',  ( 0.6499999999999561684, 12.50000000000000000, -2.511473670974877948 ) ) ;
#44312 = DIRECTION ( 'NONE',  ( 0.000000000000000000, 0.000000000000000000, 1.000000000000000000 ) ) ;
#44313 = DIRECTION ( 'NONE',  ( -0.000000000000000000, -1.000000000000000000, -0.000000000000000000 ) ) ;
#44314 = CARTESIAN_POINT ( 'NONE',  ( -2.700000000000030820, 2.500000000000000000, 0.3464101615137735735 ) ) ;
#44315 = FACE_OUTER_BOUND ( 'NONE', #47133, .T. ) ;
#44316 = ORIENTED_EDGE ( 'NONE', *, *, #128001, .F. ) ;
#44317 = VERTEX_POINT ( 'NONE', #77604 ) ;
#44318 = CARTESIAN_POINT ( 'NONE',  ( -12.49999999999999289, 2.500000000000000000, -0.7928203230275501223 ) ) ;
#44319 = EDGE_CURVE ( 'NONE', #17717, #107010, #80695, .T. ) ;
#44320 = FACE_BOUND ( 'NONE', #30325, .T. ) ;
#44321 = DIRECTION ( 'NONE',  ( -0.000000000000000000, -1.000000000000000000, -0.000000000000000000 ) ) ;
#44322 = EDGE_LOOP ( 'NONE', ( #31598, #17472, #57035, #68258, #82847, #94300, #64121, #118110 ) ) ;
#44323 = EDGE_LOOP ( 'NONE', ( #13240, #19226 ) ) ;
#44324 = CARTESIAN_POINT ( 'NONE',  ( 1.649999999999948841, 12.50000000000000000, 6.430097255199259010 ) ) ;
#44326 = ORIENTED_EDGE ( 'NONE', *, *, #81890, .F. ) ;
#44325 = AXIS2_PLACEMENT_3D ( 'NONE', #22021, #10249, #1704 ) ;
#44327 = DIRECTION ( 'NONE',  ( 0.000000000000000000, -0.000000000000000000, 1.000000000000000000 ) ) ;
#44328 = AXIS2_PLACEMENT_3D ( 'NONE', #46604, #16481, #49846 ) ;
#44329 = CARTESIAN_POINT ( 'NONE',  ( 9.199999999999915801, 12.50000000000000000, 4.265033745738159077 ) ) ;
#44330 = ORIENTED_EDGE ( 'NONE', *, *, #83085, .F. ) ;
#44331 = DIRECTION ( 'NONE',  ( 0.000000000000000000, 0.000000000000000000, 1.000000000000000000 ) ) ;
#44332 = CARTESIAN_POINT ( 'NONE',  ( 185.5000000000000000, 0.000000000000000000, 7.700000000000000178 ) ) ;
#44333 = DIRECTION ( 'NONE',  ( 0.000000000000000000, 0.000000000000000000, 1.000000000000000000 ) ) ;
#44334 = EDGE_CURVE ( 'NONE', #88750, #95225, #93210, .T. ) ;
#44336 = CONICAL_SURFACE ( 'NONE', #54794, 0.1000000000000002554, 0.003490658503988666988 ) ;
#44335 = DIRECTION ( 'NONE',  ( 0.000000000000000000, 0.000000000000000000, 1.000000000000000000 ) ) ;
#44337 = ORIENTED_EDGE ( 'NONE', *, *, #4604, .F. ) ;
#44338 = AXIS2_PLACEMENT_3D ( 'NONE', #114830, #64449, #14686 ) ;
#44339 = VECTOR ( 'NONE', #45343, 1000.000000000000000 ) ;
#44340 = DIRECTION ( 'NONE',  ( -0.000000000000000000, -1.000000000000000000, -0.000000000000000000 ) ) ;
#44341 = CIRCLE ( 'NONE', #65258, 0.1000000000000002554 ) ;
#44342 = DIRECTION ( 'NONE',  ( -0.000000000000000000, -1.000000000000000000, -0.000000000000000000 ) ) ;
#44343 = VERTEX_POINT ( 'NONE', #120607 ) ;
#44344 = ORIENTED_EDGE ( 'NONE', *, *, #23778, .F. ) ;
#44345 = CARTESIAN_POINT ( 'NONE',  ( 183.9635416670080872, -4.367472073101519747, 7.564683531249999149 ) ) ;
#44346 = FACE_OUTER_BOUND ( 'NONE', #68780, .T. ) ;
#44347 = CARTESIAN_POINT ( 'NONE',  ( 13.94999999999989448, 12.50000000000000000, -2.511473670974877948 ) ) ;
#44348 = CARTESIAN_POINT ( 'NONE',  ( -6.050000000000020250, 12.50000000000000000, -2.511473670974877948 ) ) ;
#44349 = DIRECTION ( 'NONE',  ( 0.000000000000000000, 0.000000000000000000, 1.000000000000000000 ) ) ;
#44350 = AXIS2_PLACEMENT_3D ( 'NONE', #94988, #93059, #34137 ) ;
#44351 = CARTESIAN_POINT ( 'NONE',  ( -0.2000000000000339284, 2.500000000000000000, -0.3464101615137759604 ) ) ;
#44352 = DIRECTION ( 'NONE',  ( -0.000000000000000000, 1.000000000000000000, -0.000000000000000000 ) ) ;
#44353 = CIRCLE ( 'NONE', #56853, 0.06509327318403745899 ) ;
#44354 = CARTESIAN_POINT ( 'NONE',  ( -6.850000000000017408, 2.500000000000000000, -1.718653347947325827 ) ) ;
#44355 = CIRCLE ( 'NONE', #117481, 0.06509327318403745899 ) ;
#44356 = DIRECTION ( 'NONE',  ( 0.000000000000000000, 1.000000000000000000, 0.000000000000000000 ) ) ;
#44357 = CIRCLE ( 'NONE', #23424, 0.06509327318403745899 ) ;
#44358 = CARTESIAN_POINT ( 'NONE',  ( 186.2500000000000000, 9.429780353434619030E-16, -7.700000000000000178 ) ) ;
#44359 = CARTESIAN_POINT ( 'NONE',  ( 5.199999999999935341, 2.500000000000000000, -0.4464101615137783252 ) ) ;
#44360 = ORIENTED_EDGE ( 'NONE', *, *, #124628, .T. ) ;
#44361 = ORIENTED_EDGE ( 'NONE', *, *, #27347, .T. ) ;
#44362 = EDGE_CURVE ( 'NONE', #58785, #103318, #28465, .T. ) ;
#44363 = AXIS2_PLACEMENT_3D ( 'NONE', #52334, #90975, #80525 ) ;
#44364 = ORIENTED_EDGE ( 'NONE', *, *, #117457, .T. ) ;
#44365 = ORIENTED_EDGE ( 'NONE', *, *, #40950, .F. ) ;
#44366 = CARTESIAN_POINT ( 'NONE',  ( 6.449999999999930012, 2.500000000000000000, 1.818653347947321475 ) ) ;
#44367 = CARTESIAN_POINT ( 'NONE',  ( -2.700000000000030376, 2.500000000000000000, 3.983716857408420964 ) ) ;
#44368 = DIRECTION ( 'NONE',  ( 0.000000000000000000, -0.9999939076577903929, 0.003490651415223739937 ) ) ;
#44369 = EDGE_CURVE ( 'NONE', #38578, #118512, #51246, .T. ) ;
#44370 = ORIENTED_EDGE ( 'NONE', *, *, #54823, .F. ) ;
#44371 = CARTESIAN_POINT ( 'NONE',  ( 1.699999999999951994, 2.500000000000000000, -4.330127018922201643 ) ) ;
#44372 = DIRECTION ( 'NONE',  ( -0.000000000000000000, 1.000000000000000000, -0.000000000000000000 ) ) ;
#44374 = ORIENTED_EDGE ( 'NONE', *, *, #88745, .T. ) ;
#44373 = CARTESIAN_POINT ( 'NONE',  ( -10.40000000000000213, 2.500000000000000000, 3.737306695894644371 ) ) ;
#44375 = EDGE_CURVE ( 'NONE', #129537, #105720, #97401, .T. ) ;
#44376 = EDGE_CURVE ( 'NONE', #66886, #48260, #20059, .T. ) ;
#44377 = EDGE_CURVE ( 'NONE', #118758, #110045, #117506, .T. ) ;
#44378 = DIRECTION ( 'NONE',  ( 0.000000000000000000, 0.000000000000000000, 1.000000000000000000 ) ) ;
#44379 = EDGE_CURVE ( 'NONE', #126922, #2437, #42054, .T. ) ;
#44380 = DIRECTION ( 'NONE',  ( -0.000000000000000000, -1.000000000000000000, -0.000000000000000000 ) ) ;
#44381 = ORIENTED_EDGE ( 'NONE', *, *, #41872, .F. ) ;
#44382 = ORIENTED_EDGE ( 'NONE', *, *, #82819, .F. ) ;
#44383 = VERTEX_POINT ( 'NONE', #64255 ) ;
#44384 = EDGE_LOOP ( 'NONE', ( #78967, #5686 ) ) ;
#44385 = DIRECTION ( 'NONE',  ( 0.000000000000000000, 0.000000000000000000, 1.000000000000000000 ) ) ;
#44386 = CIRCLE ( 'NONE', #23458, 0.06509327318403745899 ) ;
#44387 = CIRCLE ( 'NONE', #50653, 0.06509327318403741736 ) ;
#44388 = ADVANCED_FACE ( 'NONE', ( #41424 ), #24345, .T. ) ;
#44389 = PLANE ( 'NONE',  #105242 ) ;
#44390 = DIRECTION ( 'NONE',  ( -4.274815082592931898E-19, -0.9999939076577903929, -0.003490651415223739937 ) ) ;
#44391 = EDGE_CURVE ( 'NONE', #112116, #66867, #112081, .T. ) ;
#44392 = LINE ( 'NONE', #103968, #89545 ) ;
#44395 = ORIENTED_EDGE ( 'NONE', *, *, #26714, .T. ) ;
#44394 = EDGE_CURVE ( 'NONE', #31481, #16149, #45191, .T. ) ;
#44393 = AXIS2_PLACEMENT_3D ( 'NONE', #34932, #24450, #74841 ) ;
#44396 = AXIS2_PLACEMENT_3D ( 'NONE', #92848, #43757, #123566 ) ;
#44397 = AXIS2_PLACEMENT_3D ( 'NONE', #21632, #123669, #52376 ) ;
#44398 = CARTESIAN_POINT ( 'NONE',  ( -8.550000000000009592, 2.500000000000000000, 6.841600689897072485 ) ) ;
#44400 = ORIENTED_EDGE ( 'NONE', *, *, #14737, .T. ) ;
#44399 = AXIS2_PLACEMENT_3D ( 'NONE', #8707, #127234, #48668 ) ;
#44401 = DIRECTION ( 'NONE',  ( 0.000000000000000000, -0.9999939076577903929, 0.003490651415223739937 ) ) ;
#44402 = CARTESIAN_POINT ( 'NONE',  ( 187.5000000000000000, 0.000000000000000000, -8.699999999999999289 ) ) ;
#44403 = CIRCLE ( 'NONE', #61127, 0.1000000000000002554 ) ;
#44404 = LINE ( 'NONE', #111192, #79806 ) ;
#44405 = CARTESIAN_POINT ( 'NONE',  ( 18.87984495337918744, -0.5408627091910198637, 4.542689527608487765 ) ) ;
#44406 = CIRCLE ( 'NONE', #10926, 0.06509327318403745899 ) ;
#44407 = ORIENTED_EDGE ( 'NONE', *, *, #121339, .F. ) ;
#44408 = ORIENTED_EDGE ( 'NONE', *, *, #31695, .F. ) ;
#44409 = ORIENTED_EDGE ( 'NONE', *, *, #12303, .F. ) ;
#44410 = DIRECTION ( 'NONE',  ( 0.000000000000000000, 1.000000000000000000, 0.000000000000000000 ) ) ;
#44411 = DIRECTION ( 'NONE',  ( 0.000000000000000000, 0.000000000000000000, -1.000000000000000000 ) ) ;
#44412 = DIRECTION ( 'NONE',  ( 0.000000000000000000, 1.000000000000000000, 0.000000000000000000 ) ) ;
#44413 = FACE_BOUND ( 'NONE', #41526, .T. ) ;
#44414 = DIRECTION ( 'NONE',  ( 0.000000000000000000, 0.000000000000000000, 1.000000000000000000 ) ) ;
#44415 = FACE_OUTER_BOUND ( 'NONE', #23402, .T. ) ;
#44416 = CARTESIAN_POINT ( 'NONE',  ( -13.09999999999999254, 2.500000000000000000, -0.2464101615137741230 ) ) ;
#44417 = CONICAL_SURFACE ( 'NONE', #84119, 0.1000000000000002554, 0.003490658503988666988 ) ;
#44418 = CARTESIAN_POINT ( 'NONE',  ( 187.2968750003414300, 8.734944146203032389, 5.348610694689227483E-16 ) ) ;
#44419 = DIRECTION ( 'NONE',  ( -0.000000000000000000, 1.000000000000000000, -0.000000000000000000 ) ) ;
#44420 = LINE ( 'NONE', #111208, #13477 ) ;
#44421 = VERTEX_POINT ( 'NONE', #14498 ) ;
#44422 = CIRCLE ( 'NONE', #44512, 0.09999999999999982514 ) ;
#44423 = CIRCLE ( 'NONE', #86263, 0.06509327318403745899 ) ;
#44424 = DIRECTION ( 'NONE',  ( 0.000000000000000000, 1.000000000000000000, 0.000000000000000000 ) ) ;
#44425 = EDGE_LOOP ( 'NONE', ( #15608, #20655, #128349, #97427 ) ) ;
#44426 = ORIENTED_EDGE ( 'NONE', *, *, #49906, .T. ) ;
#44427 = ORIENTED_EDGE ( 'NONE', *, *, #30011, .T. ) ;
#44428 = ORIENTED_EDGE ( 'NONE', *, *, #49867, .F. ) ;
#44429 = LINE ( 'NONE', #122999, #52762 ) ;
#44430 = EDGE_CURVE ( 'NONE', #21815, #85672, #13768, .T. ) ;
#44431 = FACE_BOUND ( 'NONE', #87675, .T. ) ;
#44432 = AXIS2_PLACEMENT_3D ( 'NONE', #44903, #105749, #5588 ) ;
#44433 = CARTESIAN_POINT ( 'NONE',  ( -5.400000000000023448, 2.500000000000000000, -5.022947341949754119 ) ) ;
#44434 = CONICAL_SURFACE ( 'NONE', #4697, 0.1000000000000000472, 0.003490658503988666988 ) ;
#44435 = EDGE_CURVE ( 'NONE', #50468, #31778, #38952, .T. ) ;
#44436 = AXIS2_PLACEMENT_3D ( 'NONE', #38863, #80699, #11936 ) ;
#44437 = AXIS2_PLACEMENT_3D ( 'NONE', #117426, #67707, #107651 ) ;
#44438 = EDGE_CURVE ( 'NONE', #125357, #103547, #36790, .T. ) ;
#44439 =( BOUNDED_SURFACE ( )  B_SPLINE_SURFACE ( 1, 2, ( 
 ( #3732, #51564, #23360, #53495, #91470, #102571, #71845, #113042, #83599, #12255, #74418, #111764, #12887, #52196, #93410, #122238, #101305, #123501, #103234, #72493, #121565, #52840, #13547, #31917, #43051, #4350, #92775, #73751, #3105, #124153, #54130, #41752, #2428, #22116, #62024, #42383, #63952, #122877, #94055, #43691, #103877, #33221, #33838, #113699, #14183, #44300, #34511, #15477, #65876, #14815, #104510, #6289, #75685, #54756, #126744, #27236, #94688, #55422, #16108, #85520, #114963, #46895, #64585, #26604, #84873, #76355, #125444, #56680, #46237, #107078, #86139, #106447, #37716, #37078, #116895, #124809, #56046, #117528, #35154, #97272, #116259, #75060, #25290, #67138, #35781 ),
 ( #77621, #95346, #25965, #17402, #65219, #6928, #105149, #16754, #7596, #36446, #5012, #44964, #5652, #96607, #95990, #45613, #105809, #126079, #86805, #76990, #115610, #66513, #57350, #47539, #87441, #127388, #9548, #109681, #67809, #78299, #88067, #60596, #98540, #119482, #69747, #128025, #118204, #10795, #20015, #10189, #90014, #59962, #68447, #99864, #28541, #50128, #50758, #58008, #108380, #80223, #79576, #18709, #29829, #8875, #38376, #97911, #70396, #89393, #346, #78941, #40962, #128706, #109010, #40301, #39035, #58650, #48835, #69094, #120143, #88746, #118845, #29202, #20658, #30495, #110319, #19343, #59308, #90674, #100491, #48177, #99219, #1007, #80868, #18058, #49487 ) ),
 .UNSPECIFIED., .F., .F., .F. ) 
 B_SPLINE_SURFACE_WITH_KNOTS ( ( 2, 2 ),
 ( 3, 2, 2, 2, 2, 2, 2, 2, 2, 2, 2, 2, 2, 2, 2, 2, 2, 2, 2, 2, 2, 2, 2, 2, 2, 2, 2, 2, 2, 2, 2, 2, 2, 2, 2, 2, 2, 2, 2, 2, 2, 2, 3 ),
 ( 0.000000000000000000, 1.000000000000000000 ),
 ( 0.000000000000000000, 0.02380952380952380820, 0.04761904761904761640, 0.07142857142857142461, 0.09523809523809523281, 0.1190476190476190410, 0.1428571428571428492, 0.1666666666666666574, 0.1904761904761904656, 0.2142857142857142738, 0.2380952380952380820, 0.2619047619047619180, 0.2857142857142856984, 0.3095238095238095344, 0.3333333333333333148, 0.3571428571428571508, 0.3809523809523809312, 0.4047619047619047672, 0.4285714285714285476, 0.4523809523809523836, 0.4761904761904761640, 0.5000000000000000000, 0.5238095238095238360, 0.5476190476190476719, 0.5714285714285713969, 0.5952380952380952328, 0.6190476190476190688, 0.6428571428571429047, 0.6666666666666666297, 0.6904761904761904656, 0.7142857142857143016, 0.7380952380952381375, 0.7619047619047618625, 0.7857142857142856984, 0.8095238095238095344, 0.8333333333333333703, 0.8571428571428570953, 0.8809523809523809312, 0.9047619047619047672, 0.9285714285714286031, 0.9523809523809523281, 0.9761904761904761640, 1.000000000000000000 ),
 .UNSPECIFIED. ) 
 GEOMETRIC_REPRESENTATION_ITEM ( )  RATIONAL_B_SPLINE_SURFACE ( (
 ( 1.000000000000000000, 0.8660254037844387076, 1.000000000000000000, 0.8660254037844387076, 1.000000000000000000, 0.8660254037844387076, 1.000000000000000000, 0.8660254037844387076, 1.000000000000000000, 0.8660254037844387076, 1.000000000000000000, 0.8660254037844387076, 1.000000000000000000, 0.8660254037844387076, 1.000000000000000000, 0.8660254037844387076, 1.000000000000000000, 0.8660254037844387076, 1.000000000000000000, 0.8660254037844387076, 1.000000000000000000, 0.8660254037844387076, 1.000000000000000000, 0.8660254037844387076, 1.000000000000000000, 0.8660254037844387076, 1.000000000000000000, 0.8660254037844387076, 1.000000000000000000, 0.8660254037844387076, 1.000000000000000000, 0.8660254037844387076, 1.000000000000000000, 0.8660254037844387076, 1.000000000000000000, 0.8660254037844387076, 1.000000000000000000, 0.8660254037844387076, 1.000000000000000000, 0.8660254037844387076, 1.000000000000000000, 0.8660254037844387076, 1.000000000000000000, 0.8660254037844387076, 1.000000000000000000, 0.8660254037844387076, 1.000000000000000000, 0.8660254037844387076, 1.000000000000000000, 0.8660254037844387076, 1.000000000000000000, 0.8660254037844387076, 1.000000000000000000, 0.8660254037844387076, 1.000000000000000000, 0.8660254037844387076, 1.000000000000000000, 0.8660254037844387076, 1.000000000000000000, 0.8660254037844387076, 1.000000000000000000, 0.8660254037844387076, 1.000000000000000000, 0.8660254037844387076, 1.000000000000000000, 0.8660254037844387076, 1.000000000000000000, 0.8660254037844387076, 1.000000000000000000, 0.8660254037844387076, 1.000000000000000000, 0.8660254037844387076, 1.000000000000000000, 0.8660254037844387076, 1.000000000000000000, 0.8660254037844387076, 1.000000000000000000, 0.8660254037844387076, 1.000000000000000000, 0.8660254037844387076, 1.000000000000000000, 0.8660254037844387076, 1.000000000000000000, 0.8660254037844387076, 1.000000000000000000),
 ( 1.000000000000000000, 0.8660254037844387076, 1.000000000000000000, 0.8660254037844387076, 1.000000000000000000, 0.8660254037844387076, 1.000000000000000000, 0.8660254037844387076, 1.000000000000000000, 0.8660254037844387076, 1.000000000000000000, 0.8660254037844387076, 1.000000000000000000, 0.8660254037844387076, 1.000000000000000000, 0.8660254037844387076, 1.000000000000000000, 0.8660254037844387076, 1.000000000000000000, 0.8660254037844387076, 1.000000000000000000, 0.8660254037844387076, 1.000000000000000000, 0.8660254037844387076, 1.000000000000000000, 0.8660254037844387076, 1.000000000000000000, 0.8660254037844387076, 1.000000000000000000, 0.8660254037844387076, 1.000000000000000000, 0.8660254037844387076, 1.000000000000000000, 0.8660254037844387076, 1.000000000000000000, 0.8660254037844387076, 1.000000000000000000, 0.8660254037844387076, 1.000000000000000000, 0.8660254037844387076, 1.000000000000000000, 0.8660254037844387076, 1.000000000000000000, 0.8660254037844387076, 1.000000000000000000, 0.8660254037844387076, 1.000000000000000000, 0.8660254037844387076, 1.000000000000000000, 0.8660254037844387076, 1.000000000000000000, 0.8660254037844387076, 1.000000000000000000, 0.8660254037844387076, 1.000000000000000000, 0.8660254037844387076, 1.000000000000000000, 0.8660254037844387076, 1.000000000000000000, 0.8660254037844387076, 1.000000000000000000, 0.8660254037844387076, 1.000000000000000000, 0.8660254037844387076, 1.000000000000000000, 0.8660254037844387076, 1.000000000000000000, 0.8660254037844387076, 1.000000000000000000, 0.8660254037844387076, 1.000000000000000000, 0.8660254037844387076, 1.000000000000000000, 0.8660254037844387076, 1.000000000000000000, 0.8660254037844387076, 1.000000000000000000, 0.8660254037844387076, 1.000000000000000000, 0.8660254037844387076, 1.000000000000000000, 0.8660254037844387076, 1.000000000000000000, 0.8660254037844387076, 1.000000000000000000) ) ) 
 REPRESENTATION_ITEM ( '' )  SURFACE ( )  );
#44440 = ORIENTED_EDGE ( 'NONE', *, *, #129115, .F. ) ;
#44441 = CARTESIAN_POINT ( 'NONE',  ( -1.250000000000001110, 12.50000000000000000, -6.495190528383302464 ) ) ;
#44442 = CARTESIAN_POINT ( 'NONE',  ( 5.199999999999937117, 2.500000000000000000, -4.776537180435978414 ) ) ;
#44443 = ORIENTED_EDGE ( 'NONE', *, *, #96639, .F. ) ;
#44445 = DIRECTION ( 'NONE',  ( 0.000000000000000000, 1.000000000000000000, 0.000000000000000000 ) ) ;
#44444 = AXIS2_PLACEMENT_3D ( 'NONE', #52306, #31392, #73876 ) ;
#44446 = CARTESIAN_POINT ( 'NONE',  ( 5.799999999999933209, 2.500000000000000000, -0.1000000000000023925 ) ) ;
#44447 = EDGE_CURVE ( 'NONE', #20499, #49010, #86933, .T. ) ;
#44448 = AXIS2_PLACEMENT_3D ( 'NONE', #70675, #30775, #20936 ) ;
#44449 = AXIS2_PLACEMENT_3D ( 'NONE', #71340, #113200, #92272 ) ;
#44450 = VERTEX_POINT ( 'NONE', #121253 ) ;
#44451 = FACE_OUTER_BOUND ( 'NONE', #20298, .T. ) ;
#44452 = DIRECTION ( 'NONE',  ( 0.000000000000000000, 1.000000000000000000, 0.000000000000000000 ) ) ;
#44453 = CIRCLE ( 'NONE', #42415, 0.1000000000000002554 ) ;
#44454 = VERTEX_POINT ( 'NONE', #3408 ) ;
#44455 = CARTESIAN_POINT ( 'NONE',  ( 184.5000000000000000, -7.430520870378829024, -1.418378131116527108 ) ) ;
#44456 = DIRECTION ( 'NONE',  ( 0.000000000000000000, 0.000000000000000000, 1.000000000000000000 ) ) ;
#44457 = DIRECTION ( 'NONE',  ( -0.000000000000000000, -1.000000000000000000, -0.000000000000000000 ) ) ;
#44458 = ORIENTED_EDGE ( 'NONE', *, *, #13821, .F. ) ;
#44459 = ORIENTED_EDGE ( 'NONE', *, *, #115427, .T. ) ;
#44460 = LINE ( 'NONE', #84387, #105800 ) ;
#44461 = ADVANCED_FACE ( 'NONE', ( #31588 ), #13213, .T. ) ;
#44462 = ORIENTED_EDGE ( 'NONE', *, *, #9782, .T. ) ;
#44463 = DIRECTION ( 'NONE',  ( -4.274815082592931898E-19, -0.9999939076577903929, -0.003490651415223739937 ) ) ;
#44464 = DIRECTION ( 'NONE',  ( 0.000000000000000000, 1.000000000000000000, 0.000000000000000000 ) ) ;
#44465 = EDGE_LOOP ( 'NONE', ( #10052, #84219 ) ) ;
#44466 = CARTESIAN_POINT ( 'NONE',  ( -3.750000000000029310, 12.50000000000000000, -7.188010851410854052 ) ) ;
#44467 = DIRECTION ( 'NONE',  ( 0.000000000000000000, 1.000000000000000000, 0.000000000000000000 ) ) ;
#44468 = CARTESIAN_POINT ( 'NONE',  ( -7.900000000000011013, 2.500000000000000000, 4.330127018922196314 ) ) ;
#44469 = DIRECTION ( 'NONE',  ( -0.000000000000000000, 1.000000000000000000, -0.000000000000000000 ) ) ;
#44470 = DIRECTION ( 'NONE',  ( -0.000000000000000000, 1.000000000000000000, -0.000000000000000000 ) ) ;
#44471 = ORIENTED_EDGE ( 'NONE', *, *, #119329, .F. ) ;
#44472 = ORIENTED_EDGE ( 'NONE', *, *, #60242, .F. ) ;
#44473 = FACE_OUTER_BOUND ( 'NONE', #46088, .T. ) ;
#44474 = ADVANCED_FACE ( 'NONE', ( #122548 ), #124600, .T. ) ;
#44475 = CIRCLE ( 'NONE', #92502, 0.06509327318403745899 ) ;
#44476 = CARTESIAN_POINT ( 'NONE',  ( 107.6591838055444441, 5.855766388782936538, -5.000000000000004441 ) ) ;
#44477 = CIRCLE ( 'NONE', #119689, 0.06509327318403745899 ) ;
#44479 = CARTESIAN_POINT ( 'NONE',  ( -1.900000000000034994, 2.500000000000000000, -4.776537180435978414 ) ) ;
#44478 = VECTOR ( 'NONE', #123391, 1000.000000000000000 ) ;
#44481 = ORIENTED_EDGE ( 'NONE', *, *, #109507, .F. ) ;
#44480 = ORIENTED_EDGE ( 'NONE', *, *, #53436, .T. ) ;
#44482 = ORIENTED_EDGE ( 'NONE', *, *, #106607, .F. ) ;
#44483 = CARTESIAN_POINT ( 'NONE',  ( -0.8500000000000382805, 2.500000000000000000, -5.802370205355749988 ) ) ;
#44484 = DIRECTION ( 'NONE',  ( 0.000000000000000000, 0.000000000000000000, 1.000000000000000000 ) ) ;
#44486 = LINE ( 'NONE', #113882, #87362 ) ;
#44485 = VECTOR ( 'NONE', #48399, 1000.000000000000000 ) ;
#44487 = FACE_OUTER_BOUND ( 'NONE', #97991, .T. ) ;
#44488 = DIRECTION ( 'NONE',  ( 0.000000000000000000, 1.000000000000000000, 0.000000000000000000 ) ) ;
#44489 = CARTESIAN_POINT ( 'NONE',  ( 21.25101288990114412, -0.2446430927199611527, 4.189229928197906183 ) ) ;
#44490 = CONICAL_SURFACE ( 'NONE', #48714, 0.1000000000000002554, 0.003490658503988666988 ) ;
#44491 = LINE ( 'NONE', #83774, #101455 ) ;
#44492 = DIRECTION ( 'NONE',  ( 0.000000000000000000, 1.000000000000000000, 0.000000000000000000 ) ) ;
#44493 = AXIS2_PLACEMENT_3D ( 'NONE', #39527, #8720, #29677 ) ;
#44494 = EDGE_CURVE ( 'NONE', #108166, #11311, #91148, .T. ) ;
#44495 = DIRECTION ( 'NONE',  ( -0.000000000000000000, 1.000000000000000000, -0.000000000000000000 ) ) ;
#44496 = AXIS2_PLACEMENT_3D ( 'NONE', #47591, #9591, #78993 ) ;
#44497 = ORIENTED_EDGE ( 'NONE', *, *, #39596, .T. ) ;
#44498 = DIRECTION ( 'NONE',  ( -4.274815082592931898E-19, -0.9999939076577903929, -0.003490651415223739937 ) ) ;
#44499 = ORIENTED_EDGE ( 'NONE', *, *, #71145, .T. ) ;
#44500 = ADVANCED_FACE ( 'NONE', ( #43351 ), #101626, .T. ) ;
#44501 = VERTEX_POINT ( 'NONE', #83272 ) ;
#44502 = DIRECTION ( 'NONE',  ( 0.000000000000000000, 1.000000000000000000, 0.000000000000000000 ) ) ;
#44503 = CARTESIAN_POINT ( 'NONE',  ( 9.599999999999917932, 2.500000000000000000, -0.6928203230275541413 ) ) ;
#44504 = CARTESIAN_POINT ( 'NONE',  ( -12.29999999999999716, 12.50000000000000000, 0.3464101615137776813 ) ) ;
#44505 = AXIS2_PLACEMENT_3D ( 'NONE', #11398, #101727, #40222 ) ;
#44506 = LINE ( 'NONE', #15016, #48366 ) ;
#44507 = DIRECTION ( 'NONE',  ( 0.000000000000000000, 0.000000000000000000, 1.000000000000000000 ) ) ;
#44508 = CARTESIAN_POINT ( 'NONE',  ( -12.09999999999999609, 2.500000000000000000, -5.022947341949751454 ) ) ;
#44509 = CARTESIAN_POINT ( 'NONE',  ( 9.799999999999915445, 2.500000000000000000, 4.083716857408421497 ) ) ;
#44510 = EDGE_LOOP ( 'NONE', ( #69045, #3420, #85709, #22323 ) ) ;
#44511 = CARTESIAN_POINT ( 'NONE',  ( -3.550000000000028244, 12.50000000000000000, -1.818653347947326138 ) ) ;
#44512 = AXIS2_PLACEMENT_3D ( 'NONE', #13298, #32343, #14586 ) ;
#44514 = CONICAL_SURFACE ( 'NONE', #67474, 0.1000000000000000056, 0.003490658503988666988 ) ;
#44513 = CARTESIAN_POINT ( 'NONE',  ( 4.599999999999935696, 2.500000000000000000, 5.022947341949748790 ) ) ;
#44515 = ORIENTED_EDGE ( 'NONE', *, *, #114546, .T. ) ;
#44516 = AXIS2_PLACEMENT_3D ( 'NONE', #48476, #10, #98209 ) ;
#44517 = VERTEX_POINT ( 'NONE', #21772 ) ;
#44518 = EDGE_CURVE ( 'NONE', #57241, #31023, #23054, .T. ) ;
#44519 = ORIENTED_EDGE ( 'NONE', *, *, #110981, .F. ) ;
#44520 = ORIENTED_EDGE ( 'NONE', *, *, #106521, .F. ) ;
#44521 = CIRCLE ( 'NONE', #105153, 0.1000000000000000472 ) ;
#44522 = DIRECTION ( 'NONE',  ( -0.000000000000000000, 1.000000000000000000, -0.000000000000000000 ) ) ;
#44523 = CARTESIAN_POINT ( 'NONE',  ( -6.900000000000019007, 2.500000000000000000, -4.676537180435978769 ) ) ;
#44524 = CONICAL_SURFACE ( 'NONE', #117656, 0.1000000000000002554, 0.003490658503988666988 ) ;
#44526 = EDGE_CURVE ( 'NONE', #47712, #95333, #32891, .T. ) ;
#44525 = AXIS2_PLACEMENT_3D ( 'NONE', #89066, #90323, #59627 ) ;
#44527 = DIRECTION ( 'NONE',  ( 0.000000000000000000, 0.000000000000000000, 1.000000000000000000 ) ) ;
#44528 = AXIS2_PLACEMENT_3D ( 'NONE', #55813, #36829, #96359 ) ;
#44529 = DIRECTION ( 'NONE',  ( 0.000000000000000000, 0.000000000000000000, 1.000000000000000000 ) ) ;
#44530 = FACE_OUTER_BOUND ( 'NONE', #46599, .T. ) ;
#44531 = EDGE_LOOP ( 'NONE', ( #128185, #30799 ) ) ;
#44532 = DIRECTION ( 'NONE',  ( 0.000000000000000000, -0.9999939076577903929, 0.003490651415223739937 ) ) ;
#44533 = EDGE_CURVE ( 'NONE', #84391, #97166, #57795, .T. ) ;
#44534 = EDGE_CURVE ( 'NONE', #24701, #96497, #7605, .T. ) ;
#44535 = EDGE_CURVE ( 'NONE', #63642, #12902, #43994, .T. ) ;
#44536 = DIRECTION ( 'NONE',  ( -0.000000000000000000, -1.000000000000000000, -0.000000000000000000 ) ) ;
#44537 = ADVANCED_FACE ( 'NONE', ( #116571 ), #99574, .T. ) ;
#44538 = AXIS2_PLACEMENT_3D ( 'NONE', #125545, #97379, #34622 ) ;
#44539 = CARTESIAN_POINT ( 'NONE',  ( -0.2000000000000399791, 2.500000000000000000, -4.676537180435977881 ) ) ;
#44540 = ORIENTED_EDGE ( 'NONE', *, *, #82226, .T. ) ;
#44541 = VECTOR ( 'NONE', #1829, 1000.000000000000000 ) ;
#44542 = VECTOR ( 'NONE', #127576, 1000.000000000000000 ) ;
#44543 = VECTOR ( 'NONE', #117057, 1000.000000000000000 ) ;
#44544 = VERTEX_POINT ( 'NONE', #16419 ) ;
#44546 = EDGE_LOOP ( 'NONE', ( #129006, #8555, #111545, #110129 ) ) ;
#44545 = EDGE_CURVE ( 'NONE', #117445, #106877, #84970, .T. ) ;
#44547 = CARTESIAN_POINT ( 'NONE',  ( 4.549999999999937650, 12.50000000000000000, 2.165063509461097713 ) ) ;
#44548 = EDGE_CURVE ( 'NONE', #88347, #67282, #126755, .T. ) ;
#44549 = EDGE_CURVE ( 'NONE', #77475, #113921, #34829, .T. ) ;
#44550 = LINE ( 'NONE', #88815, #61357 ) ;
#44551 = FACE_OUTER_BOUND ( 'NONE', #48417, .T. ) ;
#44552 = EDGE_CURVE ( 'NONE', #125704, #82981, #125737, .T. ) ;
#44553 = EDGE_CURVE ( 'NONE', #7894, #82797, #101714, .T. ) ;
#44554 = AXIS2_PLACEMENT_3D ( 'NONE', #30630, #69899, #122227 ) ;
#44555 = ORIENTED_EDGE ( 'NONE', *, *, #81783, .F. ) ;
#44556 = CARTESIAN_POINT ( 'NONE',  ( -9.350000000000004974, 12.50000000000000000, 6.148780366869520897 ) ) ;
#44557 = CARTESIAN_POINT ( 'NONE',  ( -14.39999999999998614, 12.50000000000000000, -0.2813168883297386680 ) ) ;
#44558 = DIRECTION ( 'NONE',  ( -0.000000000000000000, 1.000000000000000000, -0.000000000000000000 ) ) ;
#44559 = CYLINDRICAL_SURFACE ( 'NONE', #100578, 7.700000000000000178 ) ;
#44560 = FACE_OUTER_BOUND ( 'NONE', #73271, .T. ) ;
#44561 = ADVANCED_FACE ( 'NONE', ( #75359 ), #127059, .T. ) ;
#44562 = EDGE_LOOP ( 'NONE', ( #106665, #18701 ) ) ;
#44563 = DIRECTION ( 'NONE',  ( 0.000000000000000000, 0.000000000000000000, 1.000000000000000000 ) ) ;
#44564 = VERTEX_POINT ( 'NONE', #37393 ) ;
#44565 = CIRCLE ( 'NONE', #69602, 0.06509327318403741736 ) ;
#44566 = ORIENTED_EDGE ( 'NONE', *, *, #32112, .F. ) ;
#44567 = AXIS2_PLACEMENT_3D ( 'NONE', #99220, #8876, #48178 ) ;
#44568 = CARTESIAN_POINT ( 'NONE',  ( -5.850000000000021849, 2.500000000000000000, -5.702370205355749455 ) ) ;
#44569 = CARTESIAN_POINT ( 'NONE',  ( -13.54999999999999005, 2.500000000000000000, -1.718653347947323828 ) ) ;
#44570 = DIRECTION ( 'NONE',  ( -0.000000000000000000, 1.000000000000000000, -0.000000000000000000 ) ) ;
#44571 = DIRECTION ( 'NONE',  ( 0.000000000000000000, -0.9999939076577903929, 0.003490651415223739937 ) ) ;
#44572 = CARTESIAN_POINT ( 'NONE',  ( 11.69999999999990870, 2.500000000000000000, 4.430127018922196847 ) ) ;
#44573 = ORIENTED_EDGE ( 'NONE', *, *, #116215, .F. ) ;
#44574 = CONICAL_SURFACE ( 'NONE', #52898, 0.1000000000000000472, 0.003490658503988666988 ) ;
#44575 = AXIS2_PLACEMENT_3D ( 'NONE', #10345, #117696, #58809 ) ;
#44576 = CIRCLE ( 'NONE', #21589, 0.06509327318403745899 ) ;
#44577 = ORIENTED_EDGE ( 'NONE', *, *, #98487, .T. ) ;
#44578 = CARTESIAN_POINT ( 'NONE',  ( -11.05000000000000071, 2.500000000000000000, -2.511473670974873951 ) ) ;
#44579 = DIRECTION ( 'NONE',  ( 0.000000000000000000, 1.000000000000000000, 0.000000000000000000 ) ) ;
#44580 = CARTESIAN_POINT ( 'NONE',  ( -11.84999999999999609, 12.50000000000000000, 2.576566944158910744 ) ) ;
#44581 = CARTESIAN_POINT ( 'NONE',  ( -6.650000000000018119, 12.50000000000000000, -6.430097255199264339 ) ) ;
#44582 = ORIENTED_EDGE ( 'NONE', *, *, #64602, .F. ) ;
#44584 = DIRECTION ( 'NONE',  ( -0.000000000000000000, -1.000000000000000000, -0.000000000000000000 ) ) ;
#44583 = AXIS2_PLACEMENT_3D ( 'NONE', #39419, #40043, #89776 ) ;
#44585 = AXIS2_PLACEMENT_3D ( 'NONE', #98446, #17962, #57910 ) ;
#44586 = CARTESIAN_POINT ( 'NONE',  ( 7.099999999999928590, 2.500000000000000000, -5.022947341949754119 ) ) ;
#44587 = EDGE_LOOP ( 'NONE', ( #79892, #18899, #98009, #79391 ) ) ;
#44588 = AXIS2_PLACEMENT_3D ( 'NONE', #106174, #6633, #107455 ) ;
#44589 = DIRECTION ( 'NONE',  ( 0.000000000000000000, 0.000000000000000000, 1.000000000000000000 ) ) ;
#44590 = ORIENTED_EDGE ( 'NONE', *, *, #29024, .F. ) ;
#44591 = DIRECTION ( 'NONE',  ( 0.000000000000000000, 1.000000000000000000, 0.000000000000000000 ) ) ;
#44592 = EDGE_CURVE ( 'NONE', #92201, #71646, #105911, .T. ) ;
#44593 = ORIENTED_EDGE ( 'NONE', *, *, #86452, .T. ) ;
#44594 = CARTESIAN_POINT ( 'NONE',  ( -5.850000000000018296, 12.50000000000000000, 5.737276932171707422 ) ) ;
#44595 = DIRECTION ( 'NONE',  ( 0.000000000000000000, 0.000000000000000000, 1.000000000000000000 ) ) ;
#44596 = EDGE_CURVE ( 'NONE', #109510, #54407, #107406, .T. ) ;
#44597 = ORIENTED_EDGE ( 'NONE', *, *, #113243, .T. ) ;
#44598 = EDGE_LOOP ( 'NONE', ( #98000, #48456, #127765, #101581 ) ) ;
#44599 = CARTESIAN_POINT ( 'NONE',  ( 186.6302083336747160, -4.367472073101514418, -7.564683531250002702 ) ) ;
#44600 = CONICAL_SURFACE ( 'NONE', #128246, 0.09999999999999982514, 0.003490658503988666988 ) ;
#44601 = DIRECTION ( 'NONE',  ( 0.000000000000000000, 1.000000000000000000, 0.000000000000000000 ) ) ;
#44602 = DIRECTION ( 'NONE',  ( 0.000000000000000000, 0.000000000000000000, 1.000000000000000000 ) ) ;
#44603 = EDGE_CURVE ( 'NONE', #9421, #81291, #15136, .T. ) ;
#44604 = CARTESIAN_POINT ( 'NONE',  ( -7.900000000000014566, 2.500000000000000000, -0.5928203230275541635 ) ) ;
#44605 = DIRECTION ( 'NONE',  ( 0.000000000000000000, 0.000000000000000000, -1.000000000000000000 ) ) ;
#44606 = CARTESIAN_POINT ( 'NONE',  ( -9.800000000000006040, 12.50000000000000000, -4.676537180435974328 ) ) ;
#44607 = DIRECTION ( 'NONE',  ( 0.000000000000000000, 0.000000000000000000, 1.000000000000000000 ) ) ;
#44608 = AXIS2_PLACEMENT_3D ( 'NONE', #25378, #74499, #103321 ) ;
#44609 = CIRCLE ( 'NONE', #59208, 0.09999999999999999167 ) ;
#44610 = CONICAL_SURFACE ( 'NONE', #109453, 0.1000000000000002554, 0.003490658503988666988 ) ;
#44611 = ORIENTED_EDGE ( 'NONE', *, *, #56966, .F. ) ;
#44612 = ORIENTED_EDGE ( 'NONE', *, *, #32226, .T. ) ;
#44613 = CARTESIAN_POINT ( 'NONE',  ( 6.899999999999926636, 2.500000000000000000, -0.3464101615137782364 ) ) ;
#44614 = CARTESIAN_POINT ( 'NONE',  ( 10.64999999999990976, 2.500000000000000000, 1.718653347947321386 ) ) ;
#44615 = CARTESIAN_POINT ( 'NONE',  ( 0.8499999999999536815, 2.500000000000000000, 5.702370205355745014 ) ) ;
#44616 = CARTESIAN_POINT ( 'NONE',  ( 14.34999999999989306, 2.500000000000000000, -1.818653347947326138 ) ) ;
#44618 = ORIENTED_EDGE ( 'NONE', *, *, #39649, .T. ) ;
#44617 = EDGE_LOOP ( 'NONE', ( #96574, #75434, #41955, #51826 ) ) ;
#44619 = DIRECTION ( 'NONE',  ( 0.000000000000000000, 0.000000000000000000, -1.000000000000000000 ) ) ;
#44620 = ORIENTED_EDGE ( 'NONE', *, *, #2856, .F. ) ;
#44621 = FACE_OUTER_BOUND ( 'NONE', #105196, .T. ) ;
#44622 = CARTESIAN_POINT ( 'NONE',  ( 4.599999999999939249, 2.500000000000000000, -3.637306695894650055 ) ) ;
#44623 = VERTEX_POINT ( 'NONE', #66186 ) ;
#44625 = DIRECTION ( 'NONE',  ( 0.000000000000000000, 0.000000000000000000, 1.000000000000000000 ) ) ;
#44624 = CONICAL_SURFACE ( 'NONE', #15353, 0.1000000000000002554, 0.003490658503988666988 ) ;
#44626 = DIRECTION ( 'NONE',  ( -4.274815082592931898E-19, -0.9999939076577903929, -0.003490651415223739937 ) ) ;
#44627 = CONICAL_SURFACE ( 'NONE', #57137, 0.1000000000000002554, 0.003490658503988666988 ) ;
#44628 = CARTESIAN_POINT ( 'NONE',  ( -8.100000000000013856, 2.500000000000000000, -4.676537180435977881 ) ) ;
#44629 = CARTESIAN_POINT ( 'NONE',  ( 11.84999999999990372, 2.500000000000000000, 2.511473670974873507 ) ) ;
#44630 = LINE ( 'NONE', #26285, #85034 ) ;
#44631 = DIRECTION ( 'NONE',  ( 0.000000000000000000, 0.000000000000000000, 1.000000000000000000 ) ) ;
#44632 = CARTESIAN_POINT ( 'NONE',  ( 12.29999999999990479, 2.500000000000000000, -4.083716857408426826 ) ) ;
#44633 = FACE_OUTER_BOUND ( 'NONE', #57446, .T. ) ;
#44634 = CIRCLE ( 'NONE', #84339, 0.09999999999999982514 ) ;
#44635 = CARTESIAN_POINT ( 'NONE',  ( 3.349999999999943689, 2.500000000000000000, 1.472243186433545459 ) ) ;
#44636 = EDGE_CURVE ( 'NONE', #36792, #98705, #4667, .T. ) ;
#44637 = ORIENTED_EDGE ( 'NONE', *, *, #39944, .T. ) ;
#44638 = VERTEX_POINT ( 'NONE', #114642 ) ;
#44639 = VERTEX_POINT ( 'NONE', #105480 ) ;
#44640 = CARTESIAN_POINT ( 'NONE',  ( 2.499999999999947153, 2.500000000000000000, -3.637306695894650055 ) ) ;
#44642 = EDGE_LOOP ( 'NONE', ( #94963, #63663, #101066, #79580 ) ) ;
#44641 = CONICAL_SURFACE ( 'NONE', #82203, 0.09999999999999982514, 0.003490658503988666988 ) ;
#44643 = AXIS2_PLACEMENT_3D ( 'NONE', #95873, #44846, #5540 ) ;
#44644 = CONICAL_SURFACE ( 'NONE', #84346, 0.09999999999999982514, 0.003490658503988666988 ) ;
#44645 = DIRECTION ( 'NONE',  ( 0.000000000000000000, 1.000000000000000000, 0.000000000000000000 ) ) ;
#44647 = ORIENTED_EDGE ( 'NONE', *, *, #44548, .F. ) ;
#44646 = ORIENTED_EDGE ( 'NONE', *, *, #104659, .F. ) ;
#44648 = ORIENTED_EDGE ( 'NONE', *, *, #99079, .F. ) ;
#44649 = AXIS2_PLACEMENT_3D ( 'NONE', #40933, #12713, #31106 ) ;
#44650 = ADVANCED_FACE ( 'NONE', ( #64893 ), #96935, .T. ) ;
#44651 = DIRECTION ( 'NONE',  ( 0.000000000000000000, 0.000000000000000000, -1.000000000000000000 ) ) ;
#44652 = CIRCLE ( 'NONE', #11273, 0.06509327318403745899 ) ;
#44653 = CARTESIAN_POINT ( 'NONE',  ( 11.84999999999990372, 2.500000000000000000, -6.941600689897078347 ) ) ;
#44654 = DIRECTION ( 'NONE',  ( 0.000000000000000000, 0.000000000000000000, 1.000000000000000000 ) ) ;
#44655 = CARTESIAN_POINT ( 'NONE',  ( -12.49999999999999289, 2.500000000000000000, 5.122947341949749323 ) ) ;
#44656 = ADVANCED_FACE ( 'NONE', ( #95020 ), #89180, .T. ) ;
#44657 = CARTESIAN_POINT ( 'NONE',  ( -11.69999999999999929, 12.50000000000000000, 1.734723475976807094E-15 ) ) ;
#44658 = VERTEX_POINT ( 'NONE', #45926 ) ;
#44659 = FACE_OUTER_BOUND ( 'NONE', #72700, .T. ) ;
#44660 = ORIENTED_EDGE ( 'NONE', *, *, #116543, .F. ) ;
#44661 = VERTEX_POINT ( 'NONE', #36099 ) ;
#44662 = ORIENTED_EDGE ( 'NONE', *, *, #84342, .T. ) ;
#44663 = CARTESIAN_POINT ( 'NONE',  ( 10.64999999999991331, 2.500000000000000000, 6.841600689897072485 ) ) ;
#44664 = VECTOR ( 'NONE', #16928, 1000.000000000000000 ) ;
#44665 = VECTOR ( 'NONE', #39814, 1000.000000000000000 ) ;
#44666 = EDGE_LOOP ( 'NONE', ( #123151, #78634 ) ) ;
#44667 = EDGE_CURVE ( 'NONE', #77344, #68306, #76012, .T. ) ;
#44668 = VERTEX_POINT ( 'NONE', #106120 ) ;
#44669 = ORIENTED_EDGE ( 'NONE', *, *, #45921, .T. ) ;
#44670 = LINE ( 'NONE', #92470, #31923 ) ;
#44672 = DIRECTION ( 'NONE',  ( 0.000000000000000000, 0.000000000000000000, 1.000000000000000000 ) ) ;
#44671 = VECTOR ( 'NONE', #34927, 1000.000000000000000 ) ;
#44673 = AXIS2_PLACEMENT_3D ( 'NONE', #13597, #73810, #64640 ) ;
#44674 = CARTESIAN_POINT ( 'NONE',  ( -6.850000000000013856, 2.500000000000000000, 2.411473670974873862 ) ) ;
#44676 = DIRECTION ( 'NONE',  ( 0.000000000000000000, 1.000000000000000000, 0.000000000000000000 ) ) ;
#44675 = CONICAL_SURFACE ( 'NONE', #92691, 0.1000000000000002554, 0.003490658503988666988 ) ;
#44677 = FACE_OUTER_BOUND ( 'NONE', #93386, .T. ) ;
#44678 = AXIS2_PLACEMENT_3D ( 'NONE', #50138, #47552, #109018 ) ;
#44679 = AXIS2_PLACEMENT_3D ( 'NONE', #50640, #895, #80757 ) ;
#44680 = ORIENTED_EDGE ( 'NONE', *, *, #58774, .F. ) ;
#44681 = CARTESIAN_POINT ( 'NONE',  ( 10.59999999999990905, 2.500000000000000000, 4.776537180435972196 ) ) ;
#44683 = ORIENTED_EDGE ( 'NONE', *, *, #55364, .T. ) ;
#44682 = AXIS2_PLACEMENT_3D ( 'NONE', #4067, #3430, #112753 ) ;
#44684 = DIRECTION ( 'NONE',  ( 0.000000000000000000, 0.000000000000000000, 1.000000000000000000 ) ) ;
#44685 = AXIS2_PLACEMENT_3D ( 'NONE', #46688, #114772, #74864 ) ;
#44686 = ORIENTED_EDGE ( 'NONE', *, *, #81778, .F. ) ;
#44687 = FACE_OUTER_BOUND ( 'NONE', #68907, .T. ) ;
#44688 = ORIENTED_EDGE ( 'NONE', *, *, #111340, .T. ) ;
#44689 = CONICAL_SURFACE ( 'NONE', #57202, 0.1000000000000002554, 0.003490658503988666988 ) ;
#44690 = ORIENTED_EDGE ( 'NONE', *, *, #7085, .F. ) ;
#44691 = DIRECTION ( 'NONE',  ( 0.000000000000000000, -0.9999939076577903929, 0.003490651415223739937 ) ) ;
#44692 = DIRECTION ( 'NONE',  ( 0.000000000000000000, 1.000000000000000000, 0.000000000000000000 ) ) ;
#44693 = ADVANCED_FACE ( 'NONE', ( #56367 ), #101508, .T. ) ;
#44694 = DIRECTION ( 'NONE',  ( 0.000000000000000000, 0.000000000000000000, -1.000000000000000000 ) ) ;
#44695 = ORIENTED_EDGE ( 'NONE', *, *, #61142, .F. ) ;
#44696 = DIRECTION ( 'NONE',  ( -0.000000000000000000, 1.000000000000000000, -0.000000000000000000 ) ) ;
#44697 = ORIENTED_EDGE ( 'NONE', *, *, #128910, .T. ) ;
#44698 = CARTESIAN_POINT ( 'NONE',  ( 9.349999999999916156, 12.50000000000000000, 6.148780366869520009 ) ) ;
#44699 = DIRECTION ( 'NONE',  ( -0.000000000000000000, -1.000000000000000000, -0.000000000000000000 ) ) ;
#44700 = APPLICATION_CONTEXT ( 'automotive_design' ) ;
#44701 = ADVANCED_FACE ( 'NONE', ( #669 ), #128925, .T. ) ;
#44702 = DIRECTION ( 'NONE',  ( 0.000000000000000000, 1.000000000000000000, 0.000000000000000000 ) ) ;
#44703 = CARTESIAN_POINT ( 'NONE',  ( 13.14999999999990088, 2.500000000000000000, 2.611473670974873151 ) ) ;
#44704 = ADVANCED_FACE ( 'NONE', ( #8539 ), #48488, .T. ) ;
#44705 = VECTOR ( 'NONE', #62924, 1000.000000000000000 ) ;
#44706 = DIRECTION ( 'NONE',  ( 0.000000000000000000, 0.000000000000000000, 1.000000000000000000 ) ) ;
#44707 = ORIENTED_EDGE ( 'NONE', *, *, #57727, .T. ) ;
#44708 = ORIENTED_EDGE ( 'NONE', *, *, #89209, .T. ) ;
#44709 = EDGE_CURVE ( 'NONE', #10341, #114322, #95447, .T. ) ;
#44710 = EDGE_CURVE ( 'NONE', #89261, #118121, #1348, .T. ) ;
#44711 = EDGE_CURVE ( 'NONE', #91607, #75694, #28206, .T. ) ;
#44712 = CONICAL_SURFACE ( 'NONE', #46766, 0.1000000000000002554, 0.003490658503988666988 ) ;
#44713 = ORIENTED_EDGE ( 'NONE', *, *, #65849, .T. ) ;
#44714 = AXIS2_PLACEMENT_3D ( 'NONE', #123169, #25588, #45898 ) ;
#44715 = DIRECTION ( 'NONE',  ( 0.000000000000000000, 0.000000000000000000, 1.000000000000000000 ) ) ;
#44716 = CARTESIAN_POINT ( 'NONE',  ( -8.350000000000013856, 2.500000000000000000, -7.188010851410848723 ) ) ;
#44717 = AXIS2_PLACEMENT_3D ( 'NONE', #67753, #67076, #49420 ) ;
#44718 = ADVANCED_FACE ( 'NONE', ( #70064 ), #50416, .T. ) ;
#44719 = B_SPLINE_CURVE_WITH_KNOTS ( 'NONE', 3,
 ( #55640, #54988, #5241, #45188 ),
 .UNSPECIFIED., .F., .F.,
 ( 4, 4 ),
 ( 0.002015733555955073232, 0.002984807578930272990 ),
 .UNSPECIFIED. ) ;
#44720 = CARTESIAN_POINT ( 'NONE',  ( 185.3802083336747160, 4.367472073101515306, 7.564683531250000925 ) ) ;
#44721 = DIRECTION ( 'NONE',  ( -4.274815082592931898E-19, -0.9999939076577903929, -0.003490651415223739937 ) ) ;
#44722 = CARTESIAN_POINT ( 'NONE',  ( 15.39999999999989022, 2.500000000000000000, 0.09999999999999761857 ) ) ;
#44723 = LINE ( 'NONE', #96368, #125578 ) ;
#44724 = AXIS2_PLACEMENT_3D ( 'NONE', #38496, #99333, #67924 ) ;
#44726 = CIRCLE ( 'NONE', #19582, 0.06509327318403745899 ) ;
#44725 = FACE_OUTER_BOUND ( 'NONE', #55503, .T. ) ;
#44727 = EDGE_LOOP ( 'NONE', ( #17263, #7756, #36937, #123371 ) ) ;
#44728 = EDGE_CURVE ( 'NONE', #10571, #49210, #32779, .T. ) ;
#44729 = AXIS2_PLACEMENT_3D ( 'NONE', #60598, #80870, #90676 ) ;
#44730 = CONICAL_SURFACE ( 'NONE', #117856, 0.09999999999999982514, 0.003490658503988666988 ) ;
#44731 = DIRECTION ( 'NONE',  ( -4.274815082592931898E-19, -0.9999939076577903929, -0.003490651415223739937 ) ) ;
#44732 = CARTESIAN_POINT ( 'NONE',  ( 2.899999999999946620, 2.500000000000000000, 0.6928203230275494784 ) ) ;
#44733 = ORIENTED_EDGE ( 'NONE', *, *, #80516, .T. ) ;
#44734 = AXIS2_PLACEMENT_3D ( 'NONE', #37072, #95337, #67127 ) ;
#44735 = DIRECTION ( 'NONE',  ( 0.000000000000000000, 0.000000000000000000, 1.000000000000000000 ) ) ;
#44736 = ORIENTED_EDGE ( 'NONE', *, *, #41797, .F. ) ;
#44737 = AXIS2_PLACEMENT_3D ( 'NONE', #57125, #64997, #55838 ) ;
#44738 = AXIS2_PLACEMENT_3D ( 'NONE', #101023, #31024, #62403 ) ;
#44739 = CONICAL_SURFACE ( 'NONE', #55197, 0.09999999999999999167, 0.003490658503988666988 ) ;
#44740 = CARTESIAN_POINT ( 'NONE',  ( -8.150000000000009237, 2.500000000000000000, 6.841600689897072485 ) ) ;
#44742 = ORIENTED_EDGE ( 'NONE', *, *, #102682, .T. ) ;
#44741 = VECTOR ( 'NONE', #96429, 1000.000000000000000 ) ;
#44743 = DIRECTION ( 'NONE',  ( -0.000000000000000000, 1.000000000000000000, -0.000000000000000000 ) ) ;
#44744 = DIRECTION ( 'NONE',  ( 0.000000000000000000, 0.000000000000000000, 1.000000000000000000 ) ) ;
#44745 = CARTESIAN_POINT ( 'NONE',  ( 1.249999999999986899, 2.500000000000000000, 6.595190528383296780 ) ) ;
#44746 = CIRCLE ( 'NONE', #61480, 0.1000000000000000472 ) ;
#44747 = ORIENTED_EDGE ( 'NONE', *, *, #103053, .T. ) ;
#44748 = CARTESIAN_POINT ( 'NONE',  ( 185.5729166673494603, 4.445597072760072876, -7.700000000000080114 ) ) ;
#44749 = PLANE ( 'NONE',  #26564 ) ;
#44750 = EDGE_LOOP ( 'NONE', ( #63325, #123806, #29221, #82616 ) ) ;
#44751 = DIRECTION ( 'NONE',  ( 0.000000000000000000, -0.000000000000000000, 1.000000000000000000 ) ) ;
#44753 = EDGE_LOOP ( 'NONE', ( #128439, #95386, #39981, #33645 ) ) ;
#44752 = ADVANCED_FACE ( 'NONE', ( #89062 ), #59625, .T. ) ;
#44754 = ORIENTED_EDGE ( 'NONE', *, *, #37209, .T. ) ;
#44755 = DIRECTION ( 'NONE',  ( 0.000000000000000000, 0.000000000000000000, -1.000000000000000000 ) ) ;
#44756 = CARTESIAN_POINT ( 'NONE',  ( -11.05000000000000071, 2.500000000000000000, 2.611473670974873151 ) ) ;
#44757 = VECTOR ( 'NONE', #124534, 1000.000000000000000 ) ;
#44758 = CIRCLE ( 'NONE', #128295, 0.06509327318403745899 ) ;
#44759 = AXIS2_PLACEMENT_3D ( 'NONE', #78452, #118346, #117036 ) ;
#44760 = ORIENTED_EDGE ( 'NONE', *, *, #96587, .F. ) ;
#44761 = CARTESIAN_POINT ( 'NONE',  ( 12.49999999999993605, 2.500000000000000000, -2.276824562219559311E-15 ) ) ;
#44762 = CARTESIAN_POINT ( 'NONE',  ( 6.649999999999928413, 12.50000000000000000, 1.472243186433545459 ) ) ;
#44763 = EDGE_LOOP ( 'NONE', ( #1128, #65971, #46773, #22802 ) ) ;
#44764 = ADVANCED_FACE ( 'NONE', ( #99536 ), #87030, .T. ) ;
#44765 = DIRECTION ( 'NONE',  ( 0.000000000000000000, 1.000000000000000000, 0.000000000000000000 ) ) ;
#44766 = DIRECTION ( 'NONE',  ( 0.000000000000000000, 1.000000000000000000, 0.000000000000000000 ) ) ;
#44767 = AXIS2_PLACEMENT_3D ( 'NONE', #49531, #29250, #119531 ) ;
#44768 = AXIS2_PLACEMENT_3D ( 'NONE', #80359, #120279, #129478 ) ;
#44769 = VECTOR ( 'NONE', #57704, 1000.000000000000000 ) ;
#44770 = CARTESIAN_POINT ( 'NONE',  ( 3.349999999999943689, 12.50000000000000000, 2.165063509461097713 ) ) ;
#44771 = DIRECTION ( 'NONE',  ( 0.000000000000000000, 0.000000000000000000, 1.000000000000000000 ) ) ;
#44772 = DIRECTION ( 'NONE',  ( 0.000000000000000000, -0.9999939076577903929, 0.003490651415223739937 ) ) ;
#44773 = CARTESIAN_POINT ( 'NONE',  ( -12.29999999999999538, 2.500000000000000000, -4.776537180435975749 ) ) ;
#44774 = CARTESIAN_POINT ( 'NONE',  ( 185.2395833340161460, 4.445597072760175905, 7.699999999999896261 ) ) ;
#44775 = AXIS2_PLACEMENT_3D ( 'NONE', #49724, #89627, #39902 ) ;
#44776 = CIRCLE ( 'NONE', #88590, 0.06509327318403745899 ) ;
#44777 = VECTOR ( 'NONE', #89682, 1000.000000000000000 ) ;
#44778 = ORIENTED_EDGE ( 'NONE', *, *, #88566, .T. ) ;
#44779 = ORIENTED_EDGE ( 'NONE', *, *, #117960, .T. ) ;
#44780 = ORIENTED_EDGE ( 'NONE', *, *, #62853, .F. ) ;
#44781 = ORIENTED_EDGE ( 'NONE', *, *, #50314, .F. ) ;
#44782 = FACE_OUTER_BOUND ( 'NONE', #108017, .T. ) ;
#44783 = CARTESIAN_POINT ( 'NONE',  ( -6.850000000000017408, 2.500000000000000000, -6.148780366869526226 ) ) ;
#44784 = CONICAL_SURFACE ( 'NONE', #113740, 0.09999999999999982514, 0.003490658503988666988 ) ;
#44785 = DIRECTION ( 'NONE',  ( -4.274815082592931898E-19, -0.9999939076577903929, -0.003490651415223739937 ) ) ;
#44786 = EDGE_LOOP ( 'NONE', ( #118217, #97615 ) ) ;
#44787 = FACE_BOUND ( 'NONE', #75524, .T. ) ;
#44788 = CARTESIAN_POINT ( 'NONE',  ( 3.949999999999940670, 2.500000000000000000, 1.818653347947321475 ) ) ;
#44789 = CARTESIAN_POINT ( 'NONE',  ( -0.8500000000000382805, 2.500000000000000000, -7.088010851410853519 ) ) ;
#44790 = CARTESIAN_POINT ( 'NONE',  ( -5.650000000000019895, 12.50000000000000000, 2.446380397790835826 ) ) ;
#44791 = DIRECTION ( 'NONE',  ( -4.274815082592931898E-19, -0.9999939076577903929, -0.003490651415223739937 ) ) ;
#44792 = DIRECTION ( 'NONE',  ( 0.000000000000000000, 0.000000000000000000, 1.000000000000000000 ) ) ;
#44793 = CIRCLE ( 'NONE', #117928, 0.06509327318403745899 ) ;
#44794 = DIRECTION ( 'NONE',  ( 0.000000000000000000, 0.000000000000000000, 1.000000000000000000 ) ) ;
#44795 = DIRECTION ( 'NONE',  ( 0.000000000000000000, 0.000000000000000000, -1.000000000000000000 ) ) ;
#44796 = DIRECTION ( 'NONE',  ( -0.000000000000000000, -1.000000000000000000, -0.000000000000000000 ) ) ;
#44797 = CARTESIAN_POINT ( 'NONE',  ( -6.650000000000015454, 12.50000000000000000, 7.253104124594885960 ) ) ;
#44798 = AXIS2_PLACEMENT_3D ( 'NONE', #109952, #9163, #40587 ) ;
#44799 = LINE ( 'NONE', #104971, #79489 ) ;
#44800 = EDGE_CURVE ( 'NONE', #114066, #72352, #59878, .T. ) ;
#44801 = EDGE_LOOP ( 'NONE', ( #114424, #4206 ) ) ;
#44802 = ORIENTED_EDGE ( 'NONE', *, *, #69329, .T. ) ;
#44803 = ORIENTED_EDGE ( 'NONE', *, *, #63, .T. ) ;
#44804 = EDGE_LOOP ( 'NONE', ( #68052, #78239 ) ) ;
#44805 = FACE_OUTER_BOUND ( 'NONE', #7878, .T. ) ;
#44806 = ORIENTED_EDGE ( 'NONE', *, *, #59039, .T. ) ;
#44807 = PLANE ( 'NONE',  #46446 ) ;
#44808 = VERTEX_POINT ( 'NONE', #2587 ) ;
#44809 = ORIENTED_EDGE ( 'NONE', *, *, #24167, .T. ) ;
#44810 = AXIS2_PLACEMENT_3D ( 'NONE', #128839, #70521, #126390 ) ;
#44811 = EDGE_CURVE ( 'NONE', #75790, #79023, #123037, .T. ) ;
#44812 = AXIS2_PLACEMENT_3D ( 'NONE', #117156, #127647, #116531 ) ;
#44813 = CARTESIAN_POINT ( 'NONE',  ( 2.500000000000002220, -1.499999999999999556, 10.00000000000000178 ) ) ;
#44814 = CARTESIAN_POINT ( 'NONE',  ( 5.599999999999933031, 12.50000000000000000, 0.3464101615137735735 ) ) ;
#44815 = LINE ( 'NONE', #54602, #11248 ) ;
#44816 = DIRECTION ( 'NONE',  ( 0.000000000000000000, 1.000000000000000000, 0.000000000000000000 ) ) ;
#44817 = EDGE_CURVE ( 'NONE', #88216, #68655, #105817, .T. ) ;
#44818 = ADVANCED_FACE ( 'NONE', ( #13703 ), #36868, .T. ) ;
#44819 = ORIENTED_EDGE ( 'NONE', *, *, #109597, .T. ) ;
#44820 = ORIENTED_EDGE ( 'NONE', *, *, #80240, .T. ) ;
#44821 = AXIS2_PLACEMENT_3D ( 'NONE', #46818, #40885, #21208 ) ;
#44822 = VERTEX_POINT ( 'NONE', #20960 ) ;
#44824 = ORIENTED_EDGE ( 'NONE', *, *, #50079, .F. ) ;
#44823 = DIRECTION ( 'NONE',  ( 0.000000000000000000, 0.000000000000000000, 1.000000000000000000 ) ) ;
#44825 = ADVANCED_FACE ( 'NONE', ( #51719 ), #22906, .T. ) ;
#44826 = DIRECTION ( 'NONE',  ( -1.000000000000000000, 0.000000000000000000, 0.000000000000000000 ) ) ;
#44827 = VERTEX_POINT ( 'NONE', #1949 ) ;
#44828 = EDGE_CURVE ( 'NONE', #114539, #126729, #53597, .T. ) ;
#44829 = ORIENTED_EDGE ( 'NONE', *, *, #30229, .T. ) ;
#44830 = FACE_OUTER_BOUND ( 'NONE', #10060, .T. ) ;
#44832 = AXIS2_PLACEMENT_3D ( 'NONE', #122503, #61656, #91746 ) ;
#44831 = FACE_OUTER_BOUND ( 'NONE', #3582, .T. ) ;
#44833 = CARTESIAN_POINT ( 'NONE',  ( 11.44999999999990514, 2.500000000000000000, 2.411473670974873862 ) ) ;
#44834 = AXIS2_PLACEMENT_3D ( 'NONE', #30914, #71452, #22386 ) ;
#44835 = DIRECTION ( 'NONE',  ( 0.000000000000000000, 0.000000000000000000, 1.000000000000000000 ) ) ;
#44836 = CARTESIAN_POINT ( 'NONE',  ( 15.19999999999989093, 12.50000000000000000, 0.3464101615137735735 ) ) ;
#44837 = CIRCLE ( 'NONE', #128464, 0.06509327318403745899 ) ;
#44838 = ORIENTED_EDGE ( 'NONE', *, *, #96261, .T. ) ;
#44839 = CONICAL_SURFACE ( 'NONE', #46891, 0.1000000000000002554, 0.003490658503988666988 ) ;
#44840 = FACE_OUTER_BOUND ( 'NONE', #75180, .T. ) ;
#44841 = ORIENTED_EDGE ( 'NONE', *, *, #29178, .T. ) ;
#44842 = DIRECTION ( 'NONE',  ( 0.000000000000000000, 0.000000000000000000, 1.000000000000000000 ) ) ;
#44843 = ORIENTED_EDGE ( 'NONE', *, *, #110048, .T. ) ;
#44844 = CARTESIAN_POINT ( 'NONE',  ( -1.650000000000035660, 2.500000000000000000, 7.088010851410848190 ) ) ;
#44845 = CARTESIAN_POINT ( 'NONE',  ( -10.85000000000000142, 12.50000000000000000, -1.472243186433546125 ) ) ;
#44846 = DIRECTION ( 'NONE',  ( 0.000000000000000000, 1.000000000000000000, 0.000000000000000000 ) ) ;
#44847 = LINE ( 'NONE', #104402, #79123 ) ;
#44848 = ORIENTED_EDGE ( 'NONE', *, *, #471, .F. ) ;
#44849 = CARTESIAN_POINT ( 'NONE',  ( -8.150000000000012790, 2.500000000000000000, 1.718653347947321386 ) ) ;
#44850 = ADVANCED_FACE ( 'NONE', ( #72651 ), #30620, .T. ) ;
#44851 = AXIS2_PLACEMENT_3D ( 'NONE', #90372, #715, #72694 ) ;
#44853 = DIRECTION ( 'NONE',  ( 0.000000000000000000, 0.000000000000000000, -1.000000000000000000 ) ) ;
#44852 = AXIS2_PLACEMENT_3D ( 'NONE', #51613, #91529, #72544 ) ;
#44854 = ORIENTED_EDGE ( 'NONE', *, *, #26705, .F. ) ;
#44855 = ORIENTED_EDGE ( 'NONE', *, *, #82552, .T. ) ;
#44856 = VECTOR ( 'NONE', #61260, 1000.000000000000000 ) ;
#44857 = CONICAL_SURFACE ( 'NONE', #23926, 0.09999999999999982514, 0.003490658503988666988 ) ;
#44858 = EDGE_LOOP ( 'NONE', ( #111450, #30709 ) ) ;
#44859 = CARTESIAN_POINT ( 'NONE',  ( 186.5000000000000000, 0.000000000000000000, 0.000000000000000000 ) ) ;
#44860 = CARTESIAN_POINT ( 'NONE',  ( 2.949999999999945111, 2.500000000000000000, 2.165063509461097713 ) ) ;
#44861 = CARTESIAN_POINT ( 'NONE',  ( 184.4427083336747160, -6.551208109652278289, 3.782341765624995134 ) ) ;
#44862 = CARTESIAN_POINT ( 'NONE',  ( 12.09999999999990550, 2.500000000000000000, -3.637306695894650055 ) ) ;
#44863 = EDGE_CURVE ( 'NONE', #35583, #10701, #122394, .T. ) ;
#44864 = CIRCLE ( 'NONE', #82520, 0.09999999999999982514 ) ;
#44865 = CARTESIAN_POINT ( 'NONE',  ( 2.099999999999950351, 2.500000000000000000, -0.7928203230275542301 ) ) ;
#44866 = VECTOR ( 'NONE', #100171, 1000.000000000000000 ) ;
#44867 = VECTOR ( 'NONE', #14694, 1000.000000000000000 ) ;
#44868 = DIRECTION ( 'NONE',  ( -4.274815082592931898E-19, -0.9999939076577903929, -0.003490651415223739937 ) ) ;
#44869 = EDGE_CURVE ( 'NONE', #66198, #74685, #120488, .T. ) ;
#44870 = ADVANCED_FACE ( 'NONE', ( #60882 ), #16089, .T. ) ;
#44871 = EDGE_CURVE ( 'NONE', #4798, #108744, #91242, .T. ) ;
#44872 = VERTEX_POINT ( 'NONE', #103393 ) ;
#44873 = VECTOR ( 'NONE', #112465, 1000.000000000000000 ) ;
#44874 = DIRECTION ( 'NONE',  ( 0.000000000000000000, 1.000000000000000000, 0.000000000000000000 ) ) ;
#44875 = AXIS2_PLACEMENT_3D ( 'NONE', #30136, #70046, #60245 ) ;
#44876 = ORIENTED_EDGE ( 'NONE', *, *, #111453, .T. ) ;
#44877 = EDGE_CURVE ( 'NONE', #38948, #4566, #85068, .T. ) ;
#44878 = CIRCLE ( 'NONE', #49187, 0.1000000000000002554 ) ;
#44879 = CARTESIAN_POINT ( 'NONE',  ( 3.949999999999942446, 12.50000000000000000, -6.841600689897078702 ) ) ;
#44880 = CARTESIAN_POINT ( 'NONE',  ( 12.09999999999990195, 12.50000000000000000, 0.6277270498435120194 ) ) ;
#44881 = DIRECTION ( 'NONE',  ( 0.000000000000000000, 1.000000000000000000, 0.000000000000000000 ) ) ;
#44882 = ORIENTED_EDGE ( 'NONE', *, *, #102791, .F. ) ;
#44883 = EDGE_CURVE ( 'NONE', #126294, #108784, #1312, .T. ) ;
#44884 = EDGE_CURVE ( 'NONE', #114224, #36786, #82934, .T. ) ;
#44885 = LINE ( 'NONE', #3652, #128696 ) ;
#44886 = CARTESIAN_POINT ( 'NONE',  ( -1.250000000000037526, 2.500000000000000000, -5.802370205355749988 ) ) ;
#44887 = VECTOR ( 'NONE', #6117, 1000.000000000000000 ) ;
#44888 = ORIENTED_EDGE ( 'NONE', *, *, #119266, .F. ) ;
#44889 = DIRECTION ( 'NONE',  ( 0.000000000000000000, 0.000000000000000000, 1.000000000000000000 ) ) ;
#44890 = ORIENTED_EDGE ( 'NONE', *, *, #99237, .T. ) ;
#44891 = ORIENTED_EDGE ( 'NONE', *, *, #106313, .T. ) ;
#44892 = CARTESIAN_POINT ( 'NONE',  ( 7.899999999999924860, 12.50000000000000000, 5.022947341949748790 ) ) ;
#44893 = EDGE_LOOP ( 'NONE', ( #10664, #102302, #22153, #10358 ) ) ;
#44894 = CARTESIAN_POINT ( 'NONE',  ( 11.89999999999990798, 2.500000000000000000, 4.083716857408421497 ) ) ;
#44895 = DIRECTION ( 'NONE',  ( 0.000000000000000000, -1.000000000000000000, 0.000000000000000000 ) ) ;
#44896 = AXIS2_PLACEMENT_3D ( 'NONE', #101927, #22091, #43664 ) ;
#44897 = CARTESIAN_POINT ( 'NONE',  ( -11.89999999999999680, 12.50000000000000000, 0.4115034346978150848 ) ) ;
#44898 = VERTEX_POINT ( 'NONE', #121728 ) ;
#44899 = FACE_BOUND ( 'NONE', #112626, .T. ) ;
#44900 = DIRECTION ( 'NONE',  ( 0.000000000000000000, 0.000000000000000000, 1.000000000000000000 ) ) ;
#44902 = VERTEX_POINT ( 'NONE', #32090 ) ;
#44901 = DIRECTION ( 'NONE',  ( -0.000000000000000000, 1.000000000000000000, -0.000000000000000000 ) ) ;
#44903 = CARTESIAN_POINT ( 'NONE',  ( 13.54999999999990123, 12.50000000000000000, 1.818653347947321475 ) ) ;
#44904 = DIRECTION ( 'NONE',  ( -0.000000000000000000, -1.000000000000000000, -0.000000000000000000 ) ) ;
#44905 = ORIENTED_EDGE ( 'NONE', *, *, #50795, .F. ) ;
#44906 = AXIS2_PLACEMENT_3D ( 'NONE', #32360, #72265, #12665 ) ;
#44907 = ORIENTED_EDGE ( 'NONE', *, *, #68361, .T. ) ;
#44908 = CIRCLE ( 'NONE', #3050, 0.06509327318403745899 ) ;
#44909 = VERTEX_POINT ( 'NONE', #111921 ) ;
#44910 = DIRECTION ( 'NONE',  ( 0.000000000000000000, 0.000000000000000000, 1.000000000000000000 ) ) ;
#44911 = DIRECTION ( 'NONE',  ( 0.000000000000000000, 0.000000000000000000, 1.000000000000000000 ) ) ;
#44912 = DIRECTION ( 'NONE',  ( -4.274815082592931898E-19, -0.9999939076577903929, -0.003490651415223739937 ) ) ;
#44913 = FACE_BOUND ( 'NONE', #3202, .T. ) ;
#44914 = ORIENTED_EDGE ( 'NONE', *, *, #83399, .F. ) ;
#44915 = CARTESIAN_POINT ( 'NONE',  ( 186.7343750003414300, 8.734944146203032389, 5.348610694689227483E-16 ) ) ;
#44916 = DIRECTION ( 'NONE',  ( 0.000000000000000000, 0.000000000000000000, -1.000000000000000000 ) ) ;
#44917 = CARTESIAN_POINT ( 'NONE',  ( -5.650000000000023448, 12.50000000000000000, -6.148780366869526226 ) ) ;
#44918 = ADVANCED_FACE ( 'NONE', ( #23529 ), #118510, .T. ) ;
#44919 = DIRECTION ( 'NONE',  ( -0.000000000000000000, -1.000000000000000000, -0.000000000000000000 ) ) ;
#44920 = AXIS2_PLACEMENT_3D ( 'NONE', #100473, #103044, #11447 ) ;
#44921 = CARTESIAN_POINT ( 'NONE',  ( 9.149999999999915090, 12.50000000000000000, -2.099970236277064473 ) ) ;
#44922 = PLANE ( 'NONE',  #52835 ) ;
#44923 = AXIS2_PLACEMENT_3D ( 'NONE', #87105, #47850, #108685 ) ;
#44924 = CARTESIAN_POINT ( 'NONE',  ( 3.749999999999940492, 12.50000000000000000, 5.802370205355744659 ) ) ;
#44925 = VECTOR ( 'NONE', #15424, 1000.000000000000000 ) ;
#44926 = LINE ( 'NONE', #63916, #24384 ) ;
#44927 = ORIENTED_EDGE ( 'NONE', *, *, #66694, .T. ) ;
#44928 = ORIENTED_EDGE ( 'NONE', *, *, #92994, .F. ) ;
#44929 = VERTEX_POINT ( 'NONE', #121092 ) ;
#44930 = VERTEX_POINT ( 'NONE', #22272 ) ;
#44931 = VERTEX_POINT ( 'NONE', #102724 ) ;
#44932 = DIRECTION ( 'NONE',  ( 0.000000000000000000, 1.000000000000000000, 0.000000000000000000 ) ) ;
#44933 = LINE ( 'NONE', #46208, #111434 ) ;
#44934 = VERTEX_POINT ( 'NONE', #21609 ) ;
#44935 = FACE_BOUND ( 'NONE', #8859, .T. ) ;
#44936 = DIRECTION ( 'NONE',  ( 0.000000000000000000, -0.000000000000000000, 1.000000000000000000 ) ) ;
#44937 = AXIS2_PLACEMENT_3D ( 'NONE', #106651, #106016, #98115 ) ;
#44938 = FACE_OUTER_BOUND ( 'NONE', #109766, .T. ) ;
#44939 = AXIS2_PLACEMENT_3D ( 'NONE', #97961, #19392, #110361 ) ;
#44940 = ORIENTED_EDGE ( 'NONE', *, *, #15050, .T. ) ;
#44941 = VECTOR ( 'NONE', #6286, 1000.000000000000000 ) ;
#44942 = CARTESIAN_POINT ( 'NONE',  ( -2.499999999999996003, 2.500000000000000000, -2.276824562219559311E-15 ) ) ;
#44943 = CARTESIAN_POINT ( 'NONE',  ( 187.0000000000000000, 0.000000000000000000, 7.700000000000000178 ) ) ;
#44944 = DIRECTION ( 'NONE',  ( -0.000000000000000000, -1.000000000000000000, -0.000000000000000000 ) ) ;
#44945 = EDGE_LOOP ( 'NONE', ( #126814, #59824, #28243, #103196 ) ) ;
#44946 = DIRECTION ( 'NONE',  ( 0.000000000000000000, 0.000000000000000000, -1.000000000000000000 ) ) ;
#44947 = CONICAL_SURFACE ( 'NONE', #78412, 0.1000000000000002554, 0.003490658503988666988 ) ;
#44948 = VERTEX_POINT ( 'NONE', #11776 ) ;
#44949 = AXIS2_PLACEMENT_3D ( 'NONE', #56206, #45766, #7101 ) ;
#44950 = CIRCLE ( 'NONE', #105587, 0.06509327318403745899 ) ;
#44951 = VERTEX_POINT ( 'NONE', #7102 ) ;
#44952 = ORIENTED_EDGE ( 'NONE', *, *, #23932, .T. ) ;
#44953 = FACE_OUTER_BOUND ( 'NONE', #46980, .T. ) ;
#44954 = CIRCLE ( 'NONE', #99332, 0.06509327318403745899 ) ;
#44955 = DIRECTION ( 'NONE',  ( 0.000000000000000000, 0.000000000000000000, 1.000000000000000000 ) ) ;
#44956 = DIRECTION ( 'NONE',  ( -0.000000000000000000, -1.000000000000000000, -0.000000000000000000 ) ) ;
#44957 = EDGE_LOOP ( 'NONE', ( #38738, #88450, #3576, #59885 ) ) ;
#44958 = CARTESIAN_POINT ( 'NONE',  ( 8.497934422428871315, 1.499999999999872768, -9.526046680185359605 ) ) ;
#44959 = AXIS2_PLACEMENT_3D ( 'NONE', #13589, #105200, #65917 ) ;
#44961 = ADVANCED_FACE ( 'NONE', ( #47054 ), #24828, .T. ) ;
#44960 = CONICAL_SURFACE ( 'NONE', #86801, 0.1000000000000002554, 0.003490658503988666988 ) ;
#44962 = DIRECTION ( 'NONE',  ( 0.000000000000000000, 0.000000000000000000, 1.000000000000000000 ) ) ;
#44963 = LINE ( 'NONE', #104509, #22367 ) ;
#44964 = CARTESIAN_POINT ( 'NONE',  ( 186.9010416670080303, -4.367472073101519747, 7.564683531249999149 ) ) ;
#44966 = CIRCLE ( 'NONE', #13638, 0.06509327318403745899 ) ;
#44965 = FACE_OUTER_BOUND ( 'NONE', #27111, .T. ) ;
#44967 = ADVANCED_FACE ( 'NONE', ( #26121 ), #116359, .T. ) ;
#44968 = DIRECTION ( 'NONE',  ( 0.000000000000000000, 1.000000000000000000, 0.000000000000000000 ) ) ;
#44969 = ADVANCED_FACE ( 'NONE', ( #35305 ), #47429, .T. ) ;
#44970 = EDGE_LOOP ( 'NONE', ( #34106, #7239 ) ) ;
#44971 = DIRECTION ( 'NONE',  ( -0.000000000000000000, -1.000000000000000000, -0.000000000000000000 ) ) ;
#44972 = ORIENTED_EDGE ( 'NONE', *, *, #125476, .F. ) ;
#44973 = ORIENTED_EDGE ( 'NONE', *, *, #45778, .F. ) ;
#44974 = FACE_OUTER_BOUND ( 'NONE', #43932, .T. ) ;
#44975 = DIRECTION ( 'NONE',  ( -0.000000000000000000, -1.000000000000000000, -0.000000000000000000 ) ) ;
#44976 = EDGE_CURVE ( 'NONE', #44564, #81764, #62103, .T. ) ;
#44977 = EDGE_CURVE ( 'NONE', #56014, #24119, #124783, .T. ) ;
#44978 = DIRECTION ( 'NONE',  ( 0.000000000000000000, 1.000000000000000000, 0.000000000000000000 ) ) ;
#44979 = DIRECTION ( 'NONE',  ( -0.000000000000000000, -1.000000000000000000, -0.000000000000000000 ) ) ;
#44980 = EDGE_CURVE ( 'NONE', #116662, #72184, #1434, .T. ) ;
#44981 = CARTESIAN_POINT ( 'NONE',  ( 184.4999999999999716, -7.141846329728243958, -2.638575396834020648 ) ) ;
#44982 = CIRCLE ( 'NONE', #28248, 0.06509327318403745899 ) ;
#44983 = ORIENTED_EDGE ( 'NONE', *, *, #111642, .T. ) ;
#44984 = ORIENTED_EDGE ( 'NONE', *, *, #19260, .F. ) ;
#44985 = CYLINDRICAL_SURFACE ( 'NONE', #28826, 3.000000000000000000 ) ;
#44986 = CARTESIAN_POINT ( 'NONE',  ( -9.350000000000008527, 2.500000000000000000, -6.841600689897072485 ) ) ;
#44987 = DIRECTION ( 'NONE',  ( 0.000000000000000000, 0.000000000000000000, 1.000000000000000000 ) ) ;
#44988 = ORIENTED_EDGE ( 'NONE', *, *, #102227, .T. ) ;
#44989 = ORIENTED_EDGE ( 'NONE', *, *, #79481, .T. ) ;
#44990 = DIRECTION ( 'NONE',  ( 0.000000000000000000, 1.000000000000000000, 0.000000000000000000 ) ) ;
#44991 = VECTOR ( 'NONE', #16588, 1000.000000000000000 ) ;
#44992 = EDGE_LOOP ( 'NONE', ( #19169, #2003 ) ) ;
#44994 = AXIS2_PLACEMENT_3D ( 'NONE', #14925, #5762, #56794 ) ;
#44993 = DIRECTION ( 'NONE',  ( -4.274815082592931898E-19, -0.9999939076577903929, -0.003490651415223739937 ) ) ;
#44995 = DIRECTION ( 'NONE',  ( -0.000000000000000000, -1.000000000000000000, -0.000000000000000000 ) ) ;
#44996 = EDGE_LOOP ( 'NONE', ( #92052, #83750, #114012, #80946 ) ) ;
#44997 = CARTESIAN_POINT ( 'NONE',  ( 11.84999999999990372, 2.500000000000000000, -6.148780366869526226 ) ) ;
#44998 = DIRECTION ( 'NONE',  ( 0.000000000000000000, 1.000000000000000000, 0.000000000000000000 ) ) ;
#44999 = FACE_OUTER_BOUND ( 'NONE', #16885, .T. ) ;
#45000 = CARTESIAN_POINT ( 'NONE',  ( 184.0000000000000000, 0.000000000000000000, 7.700000000000000178 ) ) ;
#45001 = ORIENTED_EDGE ( 'NONE', *, *, #123570, .T. ) ;
#45002 = CONICAL_SURFACE ( 'NONE', #118143, 0.1000000000000002554, 0.003490658503988666988 ) ;
#45003 = DIRECTION ( 'NONE',  ( -4.274815082592931898E-19, -0.9999939076577903929, -0.003490651415223739937 ) ) ;
#45005 = AXIS2_PLACEMENT_3D ( 'NONE', #93548, #15614, #3872 ) ;
#45004 = CARTESIAN_POINT ( 'NONE',  ( -10.60000000000000142, 2.500000000000000000, 0.3464101615137736845 ) ) ;
#45006 = ORIENTED_EDGE ( 'NONE', *, *, #189, .T. ) ;
#45007 = ORIENTED_EDGE ( 'NONE', *, *, #25304, .F. ) ;
#45008 = ADVANCED_FACE ( 'NONE', ( #24186 ), #18160, .T. ) ;
#45009 = CARTESIAN_POINT ( 'NONE',  ( 185.2968750003414300, 8.734944146203032389, 5.348610694689227483E-16 ) ) ;
#45010 = CARTESIAN_POINT ( 'NONE',  ( 3.349999999999943689, 12.50000000000000000, 1.472243186433545459 ) ) ;
#45011 = DIRECTION ( 'NONE',  ( -0.000000000000000000, -1.000000000000000000, -0.000000000000000000 ) ) ;
#45012 = DIRECTION ( 'NONE',  ( 0.000000000000000000, -0.9999939076577903929, 0.003490651415223739937 ) ) ;
#45013 = DIRECTION ( 'NONE',  ( 0.000000000000000000, 0.000000000000000000, -1.000000000000000000 ) ) ;
#45014 = AXIS2_PLACEMENT_3D ( 'NONE', #31093, #110272, #110902 ) ;
#45015 = CONICAL_SURFACE ( 'NONE', #57624, 0.1000000000000002554, 0.003490658503988666988 ) ;
#45016 = DIRECTION ( 'NONE',  ( 0.000000000000000000, -0.9999939076577903929, 0.003490651415223739937 ) ) ;
#45017 = CARTESIAN_POINT ( 'NONE',  ( -10.20000000000000284, 2.500000000000000000, -0.3464101615137782364 ) ) ;
#45018 = DIRECTION ( 'NONE',  ( 0.000000000000000000, 1.000000000000000000, 0.000000000000000000 ) ) ;
#45019 = FACE_OUTER_BOUND ( 'NONE', #112994, .T. ) ;
#45020 = EDGE_CURVE ( 'NONE', #71750, #41592, #68343, .T. ) ;
#45021 = EDGE_CURVE ( 'NONE', #29207, #109488, #3508, .T. ) ;
#45022 = EDGE_CURVE ( 'NONE', #12498, #67302, #101806, .T. ) ;
#45023 = FACE_OUTER_BOUND ( 'NONE', #21702, .T. ) ;
#45024 = VERTEX_POINT ( 'NONE', #85674 ) ;
#45025 = ORIENTED_EDGE ( 'NONE', *, *, #117108, .T. ) ;
#45027 = VERTEX_POINT ( 'NONE', #104658 ) ;
#45026 = CONICAL_SURFACE ( 'NONE', #84719, 0.09999999999999982514, 0.003490658503988666988 ) ;
#45028 = ADVANCED_FACE ( 'NONE', ( #56835 ), #91330, .T. ) ;
#45029 = VERTEX_POINT ( 'NONE', #36605 ) ;
#45030 = EDGE_CURVE ( 'NONE', #115225, #117649, #72566, .T. ) ;
#45031 = CARTESIAN_POINT ( 'NONE',  ( 6.249999999999965361, 12.50000000000000000, 2.165063509461097713 ) ) ;
#45032 = AXIS2_PLACEMENT_3D ( 'NONE', #14371, #26151, #54318 ) ;
#45033 = DIRECTION ( 'NONE',  ( 0.000000000000000000, 0.000000000000000000, 1.000000000000000000 ) ) ;
#45034 = DIRECTION ( 'NONE',  ( 0.000000000000000000, 0.000000000000000000, 1.000000000000000000 ) ) ;
#45035 = EDGE_CURVE ( 'NONE', #63269, #87633, #106003, .T. ) ;
#45036 = ORIENTED_EDGE ( 'NONE', *, *, #73825, .T. ) ;
#45037 = EDGE_CURVE ( 'NONE', #62174, #70962, #66287, .T. ) ;
#45038 = DIRECTION ( 'NONE',  ( 0.000000000000000000, 0.000000000000000000, -1.000000000000000000 ) ) ;
#45039 = EDGE_CURVE ( 'NONE', #125373, #31532, #124963, .T. ) ;
#45040 = CIRCLE ( 'NONE', #15663, 0.1000000000000000472 ) ;
#45041 = CARTESIAN_POINT ( 'NONE',  ( -2.950000000000030376, 12.50000000000000000, 6.495190528383297135 ) ) ;
#45043 = VERTEX_POINT ( 'NONE', #126251 ) ;
#45042 = FACE_OUTER_BOUND ( 'NONE', #2720, .T. ) ;
#45044 = CIRCLE ( 'NONE', #95115, 0.06509327318403745899 ) ;
#45045 = ADVANCED_FACE ( 'NONE', ( #5809 ), #129015, .T. ) ;
#45046 = CARTESIAN_POINT ( 'NONE',  ( 105.5000000000000142, -1.500000000000000222, 1.322875655532295136 ) ) ;
#45047 = ORIENTED_EDGE ( 'NONE', *, *, #122922, .T. ) ;
#45048 = CONICAL_SURFACE ( 'NONE', #61776, 0.1000000000000002554, 0.003490658503988666988 ) ;
#45049 = AXIS2_PLACEMENT_3D ( 'NONE', #85865, #4721, #36153 ) ;
#45050 = ORIENTED_EDGE ( 'NONE', *, *, #59486, .F. ) ;
#45051 = ORIENTED_EDGE ( 'NONE', *, *, #69665, .F. ) ;
#45052 = VERTEX_POINT ( 'NONE', #105965 ) ;
#45053 = FACE_OUTER_BOUND ( 'NONE', #24559, .T. ) ;
#45054 = AXIS2_PLACEMENT_3D ( 'NONE', #82219, #74330, #4921 ) ;
#45055 = CARTESIAN_POINT ( 'NONE',  ( 1.849999999999951017, 2.500000000000000000, -6.148780366869526226 ) ) ;
#45056 = CARTESIAN_POINT ( 'NONE',  ( 13.34999999999989662, 2.500000000000000000, -2.857883832488653741 ) ) ;
#45057 = CIRCLE ( 'NONE', #57577, 0.1000000000000002554 ) ;
#45058 = FACE_OUTER_BOUND ( 'NONE', #40614, .T. ) ;
#45059 = CIRCLE ( 'NONE', #118200, 0.09999999999999982514 ) ;
#45060 = ORIENTED_EDGE ( 'NONE', *, *, #35369, .F. ) ;
#45061 = CIRCLE ( 'NONE', #61787, 0.1000000000000000056 ) ;
#45063 = AXIS2_PLACEMENT_3D ( 'NONE', #62889, #13117, #3957 ) ;
#45062 = DIRECTION ( 'NONE',  ( 0.000000000000000000, 1.000000000000000000, 0.000000000000000000 ) ) ;
#45064 = ORIENTED_EDGE ( 'NONE', *, *, #54845, .F. ) ;
#45065 = CARTESIAN_POINT ( 'NONE',  ( 35.03103265469133021, -3.271231620378715288, -3.345711933289912121 ) ) ;
#45066 = CARTESIAN_POINT ( 'NONE',  ( 2.500000000000002220, -2.499999999999999556, -8.999999999999998224 ) ) ;
#45067 = DIRECTION ( 'NONE',  ( -0.000000000000000000, -1.000000000000000000, -0.000000000000000000 ) ) ;
#45068 = CARTESIAN_POINT ( 'NONE',  ( 17.34645602450340363, -0.4686430837607939992, 5.377443133677272336 ) ) ;
#45069 = EDGE_LOOP ( 'NONE', ( #24995, #4005, #86959, #21130 ) ) ;
#45070 = ORIENTED_EDGE ( 'NONE', *, *, #53326, .F. ) ;
#45071 = ORIENTED_EDGE ( 'NONE', *, *, #46653, .F. ) ;
#45072 = DIRECTION ( 'NONE',  ( -0.000000000000000000, 1.000000000000000000, -0.000000000000000000 ) ) ;
#45073 = LINE ( 'NONE', #26066, #120884 ) ;
#45074 = CARTESIAN_POINT ( 'NONE',  ( -9.600000000000006750, 2.500000000000000000, -0.7928203230275543412 ) ) ;
#45075 = FACE_BOUND ( 'NONE', #75119, .T. ) ;
#45076 = DIRECTION ( 'NONE',  ( -0.000000000000000000, -1.000000000000000000, -0.000000000000000000 ) ) ;
#45077 = AXIS2_PLACEMENT_3D ( 'NONE', #72152, #2095, #74717 ) ;
#45078 = DIRECTION ( 'NONE',  ( -0.000000000000000000, -1.000000000000000000, -0.000000000000000000 ) ) ;
#45079 = DIRECTION ( 'NONE',  ( -0.000000000000000000, -1.000000000000000000, -0.000000000000000000 ) ) ;
#45080 = ADVANCED_FACE ( 'NONE', ( #35935, #16268, #96138, #119004, #129503, #77150, #48334, #39823, #59474, #128191, #37864, #48998, #127542, #28704, #17569, #38542, #117048, #88905, #99377, #78460, #28054, #18215, #67288, #117689, #88225, #57517, #9697, #77773, #49641, #89543, #69244, #118354, #79728, #107248, #37240, #97424, #109167, #7753, #27381, #29355, #18862, #108542, #47699, #87601, #67962, #58173, #107891, #98070, #39186, #8394, #68607, #58804, #98703, #9040, #128857, #79098, #19510, #64517, #104448, #97210, #94619, #124736, #46835, #14749, #6863, #4944, #86073, #37010, #35086, #25896, #5585, #44899, #55984, #54681, #45546, #76929, #17334, #107008, #84804, #85449, #74994, #105078, #116193, #15408, #86740, #127326, #7527, #114902, #95918, #37659, #106380, #96542, #6226, #77557, #25228, #47470, #126675, #126011, #55355, #46173, #36378, #65145, #125384, #95282, #35715, #116834, #76284, #75616, #27177, #115538, #67070, #65805, #26541, #105745, #16049, #66453, #16688, #56617, #57291, #87375, #24607, #127635, #15067, #106064, #104748, #95602, #87057, #67391, #97524, #5904, #16365, #56306, #75948, #16996, #36039, #7850, #127001, #64839, #115880, #47798, #25548, #65485, #106695, #105425, #6528, #94966, #96228, #114580, #56936, #17672, #26861, #86409, #96877, #36697, #107346, #24929, #55023, #57618, #5272, #45220, #87701, #85124, #7200, #125060, #46487, #37341, #35398, #26221, #74669, #75308, #126352, #115204, #45866, #77250, #15735, #55671, #85764, #76606, #116518, #66131, #47151, #117145, #125685, #66770, #27479, #51032, #90939, #68066, #110576, #107991, #50365, #58267, #30753, #89653, #79200, #120406, #90269, #29446, #100119, #109281, #20263, #119745, #108636, #37966, #80493, #18955, #11067, #60836, #611, #89011, #77878, #88331, #78559, #70649, #98812, #59577, #128298, #58905, #118453, #129600, #28804, #10438, #28152, #9152, #117796, #49098, #40577, #69348, #8488, #60212, #18317, #20906, #98169, #99482, #100739, #48432, #39295, #38641, #68710, #19622, #128953, #119108, #9798, #39918, #49742, #79824, #30106, #70017, #109944, #82428, #33330, #103986, #41217, #42499, #14294, #83702, #122346, #81750, #32693, #123604, #53603, #113150, #63414, #73873, #61495, #83064, #71957, #1268, #43794, #111873, #54240, #24138, #13650, #52304, #81128, #51673, #41853, #33957, #62138, #22865, #91582, #72597, #23482, #103348, #121040, #93518, #1903, #52956, #2537, #31389, #64056, #12996, #71283, #3841, #102678, #62779, #102052, #92886, #111202, #21554, #121676, #101410, #113808, #11729, #32040, #22221, #12371, #3214, #112522, #92212, #43156, #122983, #73234, #35886, #76458, #64694, #55532, #104613, #125543, #106548, #56781, #116998, #16849, #15583, #107191, #14916, #5123, #7045, #25396, #115722, #54865, #67236, #4455, #5752, #17516, #47005, #85622, #45075, #126196, #84976, #26071, #36549, #46338, #75794, #84338, #45715, #124912, #65983, #105267, #34619, #35254, #105918, #24782, #75168, #115065, #27329, #126849, #96721, #16216, #94156, #124271, #116365, #44413, #74526, #65327, #95453, #114432, #56153, #94804, #96090, #86908, #37187, #6384, #86252, #26711, #66621, #77101, #99323, #29298, #7697, #97377, #78406, #8986, #30594, #20112, #39140, #128804, #79048, #118307, #118951, #80329, #47644, #107844, #40415, #128137, #50230, #70494, #90116, #28656, #38487, #48284, #9645, #57465, #87549, #58114, #60060, #18813, #58751, #99965, #79671, #88849, #119585, #29939, #127495, #69860, #98018, #109111, #98652, #37816, #120254, #69192, #68556, #108482, #88174, #19458, #59417, #49589, #77721, #445, #117637, #48939, #27997, #89496, #67915, #129452, #10292, #39775, #18168, #109783, #8346, #110418, #13494, #72438, #61975, #103181, #73076, #12207, #82905, #92059, #3056, #120881, #111712, #31234, #52150, #33170, #112998, #11570, #50863, #23314, #102529, #63252, #61330, #53449, #81601, #42331, #71135, #41700, #101246, #112363, #51512, #43004, #123451, #93362, #111039, #2373, #33791, #82262, #122825, #3686, #100589, #43634, #21390, #83552, #91426, #73703, #20754, #60694, #121509, #1742, #31867, #122186, #22705, #32531, #90778, #10899, #41064, #71794, #1106, #22059, #80969, #101895, #62626, #12835, #52786, #92720, #65819, #36391, #46188, #25912, #66467, #4302, #4960, #44913, #45562, #6879, #23983, #34455, #96559, #54701, #106394, #86753, #44246, #16703, #35729, #25241, #56631, #76300, #105095, #86090, #55371, #95936, #84170, #75013, #124101, #15421, #126025, #116207, #104462, #14139, #26555, #105761, #74364, #24626, #46849, #84819, #5596, #114280, #124752, #64536, #14763, #35103, #103829, #94633, #63902, #114916, #126693, #95296, #65160, #6240, #54081, #37022, #113645, #16060, #94002, #85467, #125399, #75632, #115552, #55998, #108954, #78245, #10138, #128650, #48780, #99810, #58601, #77568, #50084, #28492, #19292, #89970, #59905, #59255, #8824, #107694, #98494, #67085, #68399, #67762, #88695, #88018, #17351, #18009, #118150, #7541, #57954, #27832, #290, #109630, #39624, #38987, #99167, #78894, #9493, #76947, #116850, #97862, #108326, #27188, #37672, #118795, #107024, #49432, #89342, #19959, #47486, #29148, #8189, #57306, #119426, #48133, #97224, #87390, #117472, #79525, #38317, #18660, #29771, #129292, #69044, #69696, #127344, #127970, #102387, #40913, #91916, #41548, #40243, #104771, #52002, #120096, #21234, #31087, #111552, #42175, #101740, #110265, #114604, #60549, #11417, #30442, #61168, #80164, #110896, #2897, #71627, #10744, #62475, #15090, #2227, #12058, #21903, #55053, #122028, #112204, #61829, #94983, #90619, #24947, #22550, #82093, #70990, #32385, #72290, #70341, #20604, #12687, #52628, #92555, #42849, #100446, #50698, #82760, #64859, #124440, #34786, #74693, #101090, #1587, #953, #80818, #81460, #120728, #51368, #91271, #121365, #31712, #67414, #5923, #56964, #6550, #35422, #17691, #25573, #127657, #96902, #46507, #87720, #57638, #126374, #107373, #76631, #117165, #105448, #96247, #15754, #36715, #97548, #7873, #125700, #75327, #56325, #18344, #55690, #45885, #47824, #66150, #26882, #95624, #26244, #115222, #106087, #75976, #77271, #65507, #47174, #106714, #85148, #45240, #85787, #37986, #108012, #77900, #116541, #66789, #17013, #16383, #7218, #28174, #125079, #36061, #117819, #115896, #68084, #58287, #5291, #86435, #87076, #127030, #37359, #27497, #89671, #30773, #39939, #80510, #68734, #120423, #48451, #70670, #38661, #30126, #110593, #108657, #99501, #21575, #78581, #44251, #128324, #119133, #20932, #90961, #70037, #121059, #79841, #98834, #31408, #49768, #632, #71307, #8509, #9820, #111217, #51053, #119771, #49118, #40605, #89030, #109963, #118474, #20284, #88356, #28828, #60235, #81149, #100142, #10458, #50386, #79218, #59598, #98193, #18980, #90289, #60855, #58922, #9177, #100755, #11090, #1283, #128980, #39316, #29466, #41236, #69371, #109303, #19649, #51691, #62799, #124293, #12390, #54258, #94176, #41874, #32709, #2551, #3862, #91603, #103366, #33351, #11750, #4480, #113169, #22235, #13672, #61519, #43811, #123624, #44431, #121696, #53616, #42525, #101427, #104004, #82450, #34639, #84360, #73894, #112546, #74540, #111894, #102072, #14312, #22879, #64075, #83725, #92911, #33976, #113828, #1921, #24156, #62162, #23497, #102698, #81769, #114456, #73251, #32059, #71979, #52324, #3231, #92234, #93537, #122365, #72615, #63432, #13011, #52971, #43170, #83086, #123000, #36570, #7065, #116382, #17536, #64711, #104633, #97397, #94824, #5146, #37835, #6406, #7713, #45095, #86270, #37206, #35278, #26097, #77742, #84992, #56173, #54888, #45734, #77121, #47029, #96106, #86927, #126870, #14936, #117015, #25419, #76482, #66004, #57486, #127513, #47668, #85644, #5773, #15604, #46356, #26730, #126218, #124930, #87569, #75184, #125560, #115083, #35905, #65346, #95469, #27349, #66640, #105292, #67255, #106565, #107214, #24799, #16867, #55552, #75815, #56806, #105934, #115742, #16237, #96738, #67935, #80351, #89514, #48961, #119611, #29962, #60710, #69880, #8363, #88871, #107862, #98676, #28021, #58772, #120276, #19476, #88195, #10312, #18186, #99990, #58134, #49611, #468, #128156, #118974, #41087, #98043, #59438, #20134, #29315, #50884, #30616, #128830, #9666, #38506, #9006, #68578, #79690, #108504, #50247, #90803, #100610, #78434, #99347, #1133, #109806, #60076, #129473, #18834, #39794, #90138, #40438, #48304, #10925, #118327, #39156, #28672, #79067, #69216, #109137, #70512, #110437, #20781, #117654, #31256, #63276, #21416, #12862, #62649, #81621, #14158, #32558, #113018, #54104, #120903, #122208, #94024, #33815, #72462, #31892, #23336, #71816, #52811, #101268, #112387, #71160, #103200, #113669, #111734, #102548, #92081, #61352, #22084, #22730, #11598, #62003, #101918, #103853, #24002, #43656, #92746, #4326, #111062, #63928, #3077, #51540, #91445, #121540, #43028, #80988, #83578, #82931, #122844, #33196, #12231, #73102, #1765, #41726, #52174, #2399, #42359, #73729, #82284, #13519, #53471, #93387, #3706, #123474, #96583, #35754, #106420, #115581, #26582, #14784, #5626, #54731, #75660, #56655, #6905, #35128, #76325, #17377, #84196, #85495, #57328, #126717, #25939, #124778, #124123, #34480, #46210, #116234, #126054, #65844, #74387, #125420, #75034, #105784, #55394, #114308, #114940, #16085, #104486, #25264, #65186, #67106, #76967, #46871, #107054, #66489, #6267, #16724, #44272, #24645, #105126, #45581, #97245, #15446, #56021, #95958, #86115, #86772, #36414, #64559, #37052, #94661, #116871, #4983, #27212, #95320, #44935, #84846, #69071, #27865, #39010, #47515, #39650, #40272, #78920, #118173, #28518, #88718, #110290, #99842, #118822, #29172, #108980, #68427, #80198, #10161, #19318, #60571, #37694, #108350, #78275, #79549, #77592, #49463, #59284, #87415, #127365, #8214, #50106, #98515, #8851, #89994, #29802, #99193, #18685, #9516, #30465, #117497, #57979, #120118, #58629, #311, #20633, #70367, #48810, #128678, #127998, #89370, #129316, #119451, #67783, #7564, #107715, #69726, #109654, #48156, #19985, #59930, #18033, #97886, #88041, #38345, #63119, #72313, #31733, #102412, #12715, #43502, #52650, #112231, #82784, #62499, #93237, #10767, #41574, #103039, #2252, #71020, #122688, #50725, #33043, #40935, #32409, #112875, #110919, #101766, #23856, #80843, #42203, #980, #121395, #73570, #3559, #71654, #22581, #12084, #53318, #23190, #91943, #72948, #82120, #13372, #21256, #61850, #61195, #122056, #83421, #123335, #91294, #120756, #33669, #92587, #113507, #100469, #90649, #111581, #2926, #101117, #21925, #51394, #42872, #1614, #31108, #11442, #81482, #52026, #95165, #36896, #14005, #46069, #4182, #125266, #76173, #74235, #84693, #104337, #25772, #44127, #95803, #65032, #126562, #115409, #35607, #86623, #45428, #64407, #76816, #15287, #6120, #116722, #103703, #104956, #63779, #16576, #75508, #85964, #65696, #56516, #53953, #93875, #6741, #84037, #123966, #34331, #96431, #124624, #44787, #54574, #5472, #105633, #15934, #114162, #46708, #24490, #14644, #25126, #94503, #85339, #116086, #26429, #4827, #34978, #66337, #55872, #106269, #125891, #36255, #74882, #114789, #55246, #67616, #118659, #7407, #59111, #49309, #162, #99684, #37542, #58478, #40114, #99030, #80031, #66967, #68266, #27069, #109494, #18529, #107563, #9360, #17880, #88554, #47356, #98366, #106901, #17205, #108191, #57820, #48641, #38176, #97096, #97732, #8687, #87260, #8059, #48006, #49953, #59776, #119301, #128521, #57165, #127213, #10003, #77452, #39494, #87895, #28363, #127841, #89204, #78106, #38852, #117339, #78764, #27693, #129162, #89843, #29013, #118015, #68915, #108832, #19152, #29644, #79399, #69556, #19833, #13206, #23048, #82625, #11926, #43345, #20476, #62967, #60416, #2749, #10618, #112723, #42049, #31581, #72797, #42715, #111405, #52496, #61699, #102258, #93089, #81956, #121246, #119960, #53158, #2099, #70217, #122541, #91785, #51240, #121886, #32246, #102878, #72158, #112075, #12564, #22423, #3402, #30312, #110136, #100323, #21766, #90477, #92425, #50561, #32886, #823, #51871, #40780, #80689, #71493, #120601, #30950, #101616, #70860, #11283, #110768, #21104, #61031, #62338, #100948, #91142, #1460, #41417, #81329, #4035, #104180, #34161, #45270, #74077, #105474, #56359, #26274, #93719, #114634, #96274, #35453, #25604, #24975, #6583, #43986, #85182, #125111, #66179, #75352, #95014, #65539, #115254, #76003, #123189, #33524, #106113, #45916, #64885, #104803, #15128, #14489, #55082, #16411, #73422, #83885, #113351 ), #15788, .F. ) ;
#45081 = FACE_OUTER_BOUND ( 'NONE', #100463, .T. ) ;
#45082 = CIRCLE ( 'NONE', #11612, 0.06509327318403745899 ) ;
#45083 = FACE_OUTER_BOUND ( 'NONE', #22396, .T. ) ;
#45084 = CARTESIAN_POINT ( 'NONE',  ( 4.349999999999940137, 2.500000000000000000, -2.611473670974877592 ) ) ;
#45085 = VERTEX_POINT ( 'NONE', #5325 ) ;
#45086 = AXIS2_PLACEMENT_3D ( 'NONE', #55882, #34987, #114801 ) ;
#45087 = CIRCLE ( 'NONE', #26202, 0.06509327318403745899 ) ;
#45088 = DIRECTION ( 'NONE',  ( -4.274815082592931898E-19, -0.9999939076577903929, -0.003490651415223739937 ) ) ;
#45089 = ORIENTED_EDGE ( 'NONE', *, *, #124799, .F. ) ;
#45090 = ORIENTED_EDGE ( 'NONE', *, *, #811, .T. ) ;
#45091 = ORIENTED_EDGE ( 'NONE', *, *, #37766, .F. ) ;
#45092 = VERTEX_POINT ( 'NONE', #63623 ) ;
#45093 = EDGE_CURVE ( 'NONE', #74899, #104652, #83266, .T. ) ;
#45094 = CARTESIAN_POINT ( 'NONE',  ( -1.050000000000038236, 2.500000000000000000, -1.818653347947326138 ) ) ;
#45095 = FACE_BOUND ( 'NONE', #86085, .T. ) ;
#45096 = DIRECTION ( 'NONE',  ( -0.000000000000000000, 1.000000000000000000, -0.000000000000000000 ) ) ;
#45097 = AXIS2_PLACEMENT_3D ( 'NONE', #24139, #12372, #81751 ) ;
#45098 = CIRCLE ( 'NONE', #124520, 0.06509327318403745899 ) ;
#45099 = ORIENTED_EDGE ( 'NONE', *, *, #38941, .F. ) ;
#45100 = CARTESIAN_POINT ( 'NONE',  ( 21.24754738303277435, 0.7337760880902300942, 4.182111650399361835 ) ) ;
#45101 = PLANE ( 'NONE',  #68715 ) ;
#45102 = EDGE_LOOP ( 'NONE', ( #105239, #61897 ) ) ;
#45103 = DIRECTION ( 'NONE',  ( 0.000000000000000000, 0.000000000000000000, 1.000000000000000000 ) ) ;
#45104 = CARTESIAN_POINT ( 'NONE',  ( -7.500000000000016875, 2.500000000000000000, -3.737306695894649700 ) ) ;
#45105 = AXIS2_PLACEMENT_3D ( 'NONE', #95788, #46055, #106253 ) ;
#45106 = AXIS2_PLACEMENT_3D ( 'NONE', #85190, #103557, #4045 ) ;
#45107 = EDGE_LOOP ( 'NONE', ( #2739, #116063 ) ) ;
#45108 = PLANE ( 'NONE',  #100881 ) ;
#45109 = LINE ( 'NONE', #76499, #70501 ) ;
#45110 = ORIENTED_EDGE ( 'NONE', *, *, #67084, .T. ) ;
#45111 = EDGE_CURVE ( 'NONE', #117010, #94365, #39132, .T. ) ;
#45112 = CARTESIAN_POINT ( 'NONE',  ( -12.09999999999999432, 12.50000000000000000, 3.637306695894644726 ) ) ;
#45113 = CARTESIAN_POINT ( 'NONE',  ( 187.5000000000000000, 0.000000000000000000, -4.000000000000000000 ) ) ;
#45114 = DIRECTION ( 'NONE',  ( 0.000000000000000000, 1.000000000000000000, 0.000000000000000000 ) ) ;
#45115 = VERTEX_POINT ( 'NONE', #114011 ) ;
#45116 = ORIENTED_EDGE ( 'NONE', *, *, #85385, .F. ) ;
#45117 = DIRECTION ( 'NONE',  ( -0.000000000000000000, -1.000000000000000000, -0.000000000000000000 ) ) ;
#45118 = EDGE_CURVE ( 'NONE', #13831, #97216, #24336, .T. ) ;
#45119 = ORIENTED_EDGE ( 'NONE', *, *, #117058, .T. ) ;
#45120 = DIRECTION ( 'NONE',  ( -0.000000000000000000, -1.000000000000000000, -0.000000000000000000 ) ) ;
#45121 = DIRECTION ( 'NONE',  ( 0.000000000000000000, -0.000000000000000000, 1.000000000000000000 ) ) ;
#45122 = CIRCLE ( 'NONE', #55579, 0.06509327318403745899 ) ;
#45123 = VERTEX_POINT ( 'NONE', #64249 ) ;
#45124 = CIRCLE ( 'NONE', #120340, 0.06509327318403745899 ) ;
#45125 = DIRECTION ( 'NONE',  ( -0.000000000000000000, -1.000000000000000000, -0.000000000000000000 ) ) ;
#45126 = LINE ( 'NONE', #53011, #127766 ) ;
#45127 = CARTESIAN_POINT ( 'NONE',  ( -3.750000000000029310, 2.500000000000000000, -7.288010851410854585 ) ) ;
#45128 = EDGE_CURVE ( 'NONE', #7788, #99762, #13956, .T. ) ;
#45129 = ADVANCED_FACE ( 'NONE', ( #115930 ), #32859, .T. ) ;
#45130 = DIRECTION ( 'NONE',  ( 0.000000000000000000, 0.000000000000000000, -1.000000000000000000 ) ) ;
#45131 = ADVANCED_FACE ( 'NONE', ( #36091 ), #34822, .T. ) ;
#45132 = EDGE_CURVE ( 'NONE', #114231, #90411, #60728, .T. ) ;
#45133 = EDGE_CURVE ( 'NONE', #114688, #101225, #80879, .T. ) ;
#45134 = DIRECTION ( 'NONE',  ( -0.000000000000000000, -1.000000000000000000, -0.000000000000000000 ) ) ;
#45135 = VERTEX_POINT ( 'NONE', #58320 ) ;
#45136 = EDGE_LOOP ( 'NONE', ( #66402, #40754 ) ) ;
#45137 = CARTESIAN_POINT ( 'NONE',  ( -1.250000000000001110, 12.50000000000000000, -2.165063509461101710 ) ) ;
#45138 = CARTESIAN_POINT ( 'NONE',  ( 2.299999999999946976, 12.50000000000000000, 4.676537180435972552 ) ) ;
#45139 = CARTESIAN_POINT ( 'NONE',  ( -1.900000000000035438, 12.50000000000000000, 4.048810130592458201 ) ) ;
#45142 = EDGE_LOOP ( 'NONE', ( #86486, #9528, #81615, #12953 ) ) ;
#45141 = EDGE_LOOP ( 'NONE', ( #22797, #108149 ) ) ;
#45140 = AXIS2_PLACEMENT_3D ( 'NONE', #99134, #70957, #69011 ) ;
#45143 = ORIENTED_EDGE ( 'NONE', *, *, #67973, .T. ) ;
#45144 = EDGE_CURVE ( 'NONE', #57084, #2830, #93391, .T. ) ;
#45145 = DIRECTION ( 'NONE',  ( 0.000000000000000000, 0.000000000000000000, 1.000000000000000000 ) ) ;
#45146 = ADVANCED_FACE ( 'NONE', ( #18368 ), #66378, .T. ) ;
#45147 = AXIS2_PLACEMENT_3D ( 'NONE', #128592, #58549, #27771 ) ;
#45149 = CIRCLE ( 'NONE', #22175, 0.1000000000000000472 ) ;
#45148 = DIRECTION ( 'NONE',  ( -0.000000000000000000, 1.000000000000000000, -0.000000000000000000 ) ) ;
#45150 = EDGE_CURVE ( 'NONE', #49498, #9133, #110109, .T. ) ;
#45151 = DIRECTION ( 'NONE',  ( 0.000000000000000000, 1.000000000000000000, 0.000000000000000000 ) ) ;
#45152 = CARTESIAN_POINT ( 'NONE',  ( 0.000000000000000000, 0.000000000000000000, 0.000000000000000000 ) ) ;
#45153 = DIRECTION ( 'NONE',  ( 0.000000000000000000, 1.000000000000000000, 0.000000000000000000 ) ) ;
#45154 = DIRECTION ( 'NONE',  ( -0.000000000000000000, 1.000000000000000000, -0.000000000000000000 ) ) ;
#45155 = LINE ( 'NONE', #124988, #82011 ) ;
#45156 = CIRCLE ( 'NONE', #107829, 0.1000000000000002554 ) ;
#45157 = CARTESIAN_POINT ( 'NONE',  ( -3.749999999999991118, 12.50000000000000000, -2.230156782645139391 ) ) ;
#45158 = DIRECTION ( 'NONE',  ( 0.000000000000000000, 1.000000000000000000, 0.000000000000000000 ) ) ;
#45159 = CARTESIAN_POINT ( 'NONE',  ( -9.800000000000004263, 2.500000000000000000, 3.983716857408420076 ) ) ;
#45160 = VERTEX_POINT ( 'NONE', #41105 ) ;
#45161 = FACE_OUTER_BOUND ( 'NONE', #128203, .T. ) ;
#45162 = ORIENTED_EDGE ( 'NONE', *, *, #100595, .F. ) ;
#45163 = VERTEX_POINT ( 'NONE', #118500 ) ;
#45164 = CARTESIAN_POINT ( 'NONE',  ( -4.150000000000025224, 12.50000000000000000, 5.802370205355744659 ) ) ;
#45165 = FACE_OUTER_BOUND ( 'NONE', #15422, .T. ) ;
#45166 = CONICAL_SURFACE ( 'NONE', #34715, 0.1000000000000000472, 0.003490658503988666988 ) ;
#45167 = CARTESIAN_POINT ( 'NONE',  ( -13.09999999999999076, 12.50000000000000000, 4.676537180435972552 ) ) ;
#45168 = DIRECTION ( 'NONE',  ( 0.000000000000000000, 0.000000000000000000, -1.000000000000000000 ) ) ;
#45169 = LINE ( 'NONE', #125006, #48599 ) ;
#45170 = FACE_OUTER_BOUND ( 'NONE', #23229, .T. ) ;
#45171 = DIRECTION ( 'NONE',  ( 0.000000000000000000, 1.000000000000000000, 0.000000000000000000 ) ) ;
#45172 = VERTEX_POINT ( 'NONE', #38688 ) ;
#45173 = CARTESIAN_POINT ( 'NONE',  ( -2.900000000000029221, 2.500000000000000000, -4.230127018922201998 ) ) ;
#45174 = VECTOR ( 'NONE', #15627, 1000.000000000000000 ) ;
#45175 = CIRCLE ( 'NONE', #124587, 0.09999999999999999167 ) ;
#45176 = VECTOR ( 'NONE', #104325, 1000.000000000000000 ) ;
#45177 = DIRECTION ( 'NONE',  ( 0.000000000000000000, 0.000000000000000000, -1.000000000000000000 ) ) ;
#45178 = ORIENTED_EDGE ( 'NONE', *, *, #48109, .T. ) ;
#45179 = ORIENTED_EDGE ( 'NONE', *, *, #92304, .F. ) ;
#45180 = VECTOR ( 'NONE', #115223, 1000.000000000000000 ) ;
#45181 = VERTEX_POINT ( 'NONE', #8532 ) ;
#45182 = EDGE_CURVE ( 'NONE', #55240, #127628, #129106, .T. ) ;
#45183 = ORIENTED_EDGE ( 'NONE', *, *, #101211, .F. ) ;
#45184 = DIRECTION ( 'NONE',  ( -0.000000000000000000, 1.000000000000000000, -0.000000000000000000 ) ) ;
#45185 = DIRECTION ( 'NONE',  ( 0.000000000000000000, -0.9999939076577903929, 0.003490651415223739937 ) ) ;
#45186 = CONICAL_SURFACE ( 'NONE', #80790, 0.1000000000000002554, 0.003490658503988666988 ) ;
#45187 = EDGE_CURVE ( 'NONE', #6862, #48547, #49682, .T. ) ;
#45188 = CARTESIAN_POINT ( 'NONE',  ( 16.55874544816221317, -0.4845305829210151960, -6.091953208799018249 ) ) ;
#45189 = DIRECTION ( 'NONE',  ( 0.000000000000000000, -0.9999939076577903929, 0.003490651415223739937 ) ) ;
#45192 = EDGE_CURVE ( 'NONE', #96334, #68282, #57983, .T. ) ;
#45191 = CIRCLE ( 'NONE', #76488, 0.06509327318403745899 ) ;
#45190 = AXIS2_PLACEMENT_3D ( 'NONE', #109352, #40, #40647 ) ;
#45193 = DIRECTION ( 'NONE',  ( 0.000000000000000000, 0.000000000000000000, 1.000000000000000000 ) ) ;
#45194 = ORIENTED_EDGE ( 'NONE', *, *, #74399, .F. ) ;
#45195 = FACE_OUTER_BOUND ( 'NONE', #106717, .T. ) ;
#45196 = DIRECTION ( 'NONE',  ( 0.000000000000000000, -0.9999939076577903929, 0.003490651415223739937 ) ) ;
#45197 = EDGE_CURVE ( 'NONE', #126533, #92856, #126939, .T. ) ;
#45198 = CARTESIAN_POINT ( 'NONE',  ( -10.65000000000000213, 12.50000000000000000, 6.841600689897072485 ) ) ;
#45199 = ORIENTED_EDGE ( 'NONE', *, *, #57727, .F. ) ;
#45200 = ORIENTED_EDGE ( 'NONE', *, *, #86954, .F. ) ;
#45201 = ORIENTED_EDGE ( 'NONE', *, *, #12627, .F. ) ;
#45202 = LINE ( 'NONE', #83816, #88483 ) ;
#45203 = CARTESIAN_POINT ( 'NONE',  ( -10.80000000000000249, 12.50000000000000000, -4.330127018922197202 ) ) ;
#45204 = CARTESIAN_POINT ( 'NONE',  ( -9.150000000000009237, 2.500000000000000000, -2.857883832488653741 ) ) ;
#45205 = VERTEX_POINT ( 'NONE', #47852 ) ;
#45206 = CARTESIAN_POINT ( 'NONE',  ( 4.349999999999941025, 2.500000000000000000, -6.148780366869526226 ) ) ;
#45207 = DIRECTION ( 'NONE',  ( 0.000000000000000000, 0.000000000000000000, -1.000000000000000000 ) ) ;
#45208 = CARTESIAN_POINT ( 'NONE',  ( -2.300000000000033573, 2.500000000000000000, 0.3464101615137735735 ) ) ;
#45209 = DIRECTION ( 'NONE',  ( 0.000000000000000000, 0.000000000000000000, -1.000000000000000000 ) ) ;
#45210 = EDGE_CURVE ( 'NONE', #40173, #16061, #9945, .T. ) ;
#45211 = DIRECTION ( 'NONE',  ( 0.000000000000000000, -0.9999939076577903929, 0.003490651415223739937 ) ) ;
#45212 = EDGE_LOOP ( 'NONE', ( #94853, #23370, #103466, #74771 ) ) ;
#45213 = VECTOR ( 'NONE', #117867, 1000.000000000000000 ) ;
#45214 = DIRECTION ( 'NONE',  ( -0.000000000000000000, 1.000000000000000000, -0.000000000000000000 ) ) ;
#45215 = CONICAL_SURFACE ( 'NONE', #22239, 0.1000000000000000472, 0.003490658503988666988 ) ;
#45216 = ORIENTED_EDGE ( 'NONE', *, *, #42393, .F. ) ;
#45217 = ORIENTED_EDGE ( 'NONE', *, *, #35112, .F. ) ;
#45218 = ORIENTED_EDGE ( 'NONE', *, *, #69944, .T. ) ;
#45219 = CARTESIAN_POINT ( 'NONE',  ( 129.5000000000000000, -1.000000000000025535, 7.634788798650553154 ) ) ;
#45220 = FACE_BOUND ( 'NONE', #50224, .T. ) ;
#45221 = CARTESIAN_POINT ( 'NONE',  ( -9.600000000000008527, 12.50000000000000000, -4.957854068765712441 ) ) ;
#45222 = CARTESIAN_POINT ( 'NONE',  ( -1.050000000000038236, 12.50000000000000000, -6.083687093685488989 ) ) ;
#45223 = AXIS2_PLACEMENT_3D ( 'NONE', #7503, #69003, #27152 ) ;
#45224 = CYLINDRICAL_SURFACE ( 'NONE', #54323, 5.000000000000000000 ) ;
#45225 = ADVANCED_FACE ( 'NONE', ( #77294 ), #17044, .T. ) ;
#45226 = EDGE_LOOP ( 'NONE', ( #39837, #57569, #90228, #59681 ) ) ;
#45227 = DIRECTION ( 'NONE',  ( 0.000000000000000000, 1.000000000000000000, 0.000000000000000000 ) ) ;
#45228 = DIRECTION ( 'NONE',  ( -4.274815082592931898E-19, -0.9999939076577903929, -0.003490651415223739937 ) ) ;
#45229 = PLANE ( 'NONE',  #67485 ) ;
#45230 = CARTESIAN_POINT ( 'NONE',  ( -11.64999999999999680, 2.500000000000000000, 7.088010851410848190 ) ) ;
#45231 = EDGE_LOOP ( 'NONE', ( #109707, #94444 ) ) ;
#45233 = CIRCLE ( 'NONE', #97537, 0.06509327318403745899 ) ;
#45232 = AXIS2_PLACEMENT_3D ( 'NONE', #98289, #38098, #77378 ) ;
#45234 = DIRECTION ( 'NONE',  ( -4.274815082592931898E-19, -0.9999939076577903929, -0.003490651415223739937 ) ) ;
#45235 = DIRECTION ( 'NONE',  ( -0.000000000000000000, -1.000000000000000000, -0.000000000000000000 ) ) ;
#45236 = ORIENTED_EDGE ( 'NONE', *, *, #76632, .T. ) ;
#45237 = DIRECTION ( 'NONE',  ( -0.000000000000000000, -1.000000000000000000, -0.000000000000000000 ) ) ;
#45238 = EDGE_CURVE ( 'NONE', #108508, #106998, #7791, .T. ) ;
#45239 = VERTEX_POINT ( 'NONE', #97574 ) ;
#45240 = FACE_BOUND ( 'NONE', #127236, .T. ) ;
#45241 = DIRECTION ( 'NONE',  ( 0.000000000000000000, 0.000000000000000000, 1.000000000000000000 ) ) ;
#45242 = EDGE_LOOP ( 'NONE', ( #63834, #102153 ) ) ;
#45243 = DIRECTION ( 'NONE',  ( -4.274815082592931898E-19, -0.9999939076577903929, -0.003490651415223739937 ) ) ;
#45244 = FACE_OUTER_BOUND ( 'NONE', #58978, .T. ) ;
#45245 = ORIENTED_EDGE ( 'NONE', *, *, #77643, .T. ) ;
#45246 = ORIENTED_EDGE ( 'NONE', *, *, #75293, .F. ) ;
#45247 = CARTESIAN_POINT ( 'NONE',  ( 186.0052083336747444, -6.551208109652278289, 3.782341765624995134 ) ) ;
#45248 = ORIENTED_EDGE ( 'NONE', *, *, #6678, .T. ) ;
#45249 = LINE ( 'NONE', #119141, #59461 ) ;
#45250 = FACE_OUTER_BOUND ( 'NONE', #58284, .T. ) ;
#45251 = CONICAL_SURFACE ( 'NONE', #76644, 0.1000000000000002554, 0.003490658503988666988 ) ;
#45252 = CIRCLE ( 'NONE', #61984, 0.06509327318403745899 ) ;
#45253 = EDGE_CURVE ( 'NONE', #80196, #90044, #74696, .T. ) ;
#45254 = DIRECTION ( 'NONE',  ( 0.000000000000000000, 0.000000000000000000, -1.000000000000000000 ) ) ;
#45255 = DIRECTION ( 'NONE',  ( 0.000000000000000000, 0.000000000000000000, 1.000000000000000000 ) ) ;
#45256 = DIRECTION ( 'NONE',  ( 0.000000000000000000, 1.000000000000000000, 0.000000000000000000 ) ) ;
#45257 = CIRCLE ( 'NONE', #70301, 0.06509327318403745899 ) ;
#45258 = CARTESIAN_POINT ( 'NONE',  ( -7.050000000000013145, 2.500000000000000000, 2.065063509461097624 ) ) ;
#45259 = CIRCLE ( 'NONE', #116341, 0.1000000000000002554 ) ;
#45260 = EDGE_LOOP ( 'NONE', ( #34885, #93551 ) ) ;
#45261 = AXIS2_PLACEMENT_3D ( 'NONE', #42526, #33353, #93538 ) ;
#45263 = VERTEX_POINT ( 'NONE', #66813 ) ;
#45262 = EDGE_CURVE ( 'NONE', #126164, #71809, #87746, .T. ) ;
#45264 = LINE ( 'NONE', #54420, #121777 ) ;
#45265 = CARTESIAN_POINT ( 'NONE',  ( -7.700000000000016165, 2.500000000000000000, 0.2464101615137735679 ) ) ;
#45266 = DIRECTION ( 'NONE',  ( 0.000000000000000000, -0.000000000000000000, 1.000000000000000000 ) ) ;
#45267 = CARTESIAN_POINT ( 'NONE',  ( 1.899999999999949507, 12.50000000000000000, 4.741630453620009789 ) ) ;
#45269 = EDGE_LOOP ( 'NONE', ( #1633, #88865, #97057, #125155 ) ) ;
#45268 = VERTEX_POINT ( 'NONE', #7900 ) ;
#45270 = FACE_BOUND ( 'NONE', #125954, .T. ) ;
#45271 = ORIENTED_EDGE ( 'NONE', *, *, #128067, .F. ) ;
#45272 = FACE_OUTER_BOUND ( 'NONE', #76078, .T. ) ;
#45273 = DIRECTION ( 'NONE',  ( 0.000000000000000000, 0.000000000000000000, 1.000000000000000000 ) ) ;
#45274 = AXIS2_PLACEMENT_3D ( 'NONE', #116055, #26405, #68238 ) ;
#45275 = VERTEX_POINT ( 'NONE', #106744 ) ;
#45277 = EDGE_CURVE ( 'NONE', #9179, #15257, #14039, .T. ) ;
#45276 = CARTESIAN_POINT ( 'NONE',  ( -11.44999999999999751, 2.500000000000000000, -6.741600689897073728 ) ) ;
#45278 = DIRECTION ( 'NONE',  ( 0.000000000000000000, 1.000000000000000000, 0.000000000000000000 ) ) ;
#45279 = CARTESIAN_POINT ( 'NONE',  ( -9.200000000000006395, 2.500000000000000000, 4.330127018922196314 ) ) ;
#45281 = VECTOR ( 'NONE', #57003, 1000.000000000000000 ) ;
#45280 = AXIS2_PLACEMENT_3D ( 'NONE', #96625, #74440, #75079 ) ;
#45282 = CARTESIAN_POINT ( 'NONE',  ( -4.400000000000025224, 2.500000000000000000, 4.083716857408420609 ) ) ;
#45283 = DIRECTION ( 'NONE',  ( 0.000000000000000000, 0.000000000000000000, 1.000000000000000000 ) ) ;
#45284 = CARTESIAN_POINT ( 'NONE',  ( -7.300000000000018474, 2.500000000000000000, 0.3464101615137735735 ) ) ;
#45285 = ADVANCED_FACE ( 'NONE', ( #50914 ), #16185, .T. ) ;
#45286 = ADVANCED_FACE ( 'NONE', ( #4345 ), #26585, .T. ) ;
#45287 = CARTESIAN_POINT ( 'NONE',  ( 186.6093750003414016, 9.264065473108010111E-16, -7.564683531250000925 ) ) ;
#45288 = LINE ( 'NONE', #87124, #33901 ) ;
#45289 = EDGE_CURVE ( 'NONE', #83265, #14140, #62020, .T. ) ;
#45290 = EDGE_CURVE ( 'NONE', #117196, #49455, #91464, .T. ) ;
#45291 = DIRECTION ( 'NONE',  ( -0.000000000000000000, 1.000000000000000000, -0.000000000000000000 ) ) ;
#45292 = ORIENTED_EDGE ( 'NONE', *, *, #37917, .T. ) ;
#45293 = VERTEX_POINT ( 'NONE', #63947 ) ;
#45294 = CARTESIAN_POINT ( 'NONE',  ( 3.099999999999945466, 2.500000000000000000, -4.083716857408426826 ) ) ;
#45295 = VERTEX_POINT ( 'NONE', #31911 ) ;
#45296 = EDGE_CURVE ( 'NONE', #7787, #85940, #101939, .T. ) ;
#45297 = CARTESIAN_POINT ( 'NONE',  ( -2.500000000000030642, 2.500000000000000000, -5.022947341949754119 ) ) ;
#45300 = EDGE_LOOP ( 'NONE', ( #67102, #77734, #128558, #35335 ) ) ;
#45299 = ORIENTED_EDGE ( 'NONE', *, *, #47779, .T. ) ;
#45298 = EDGE_CURVE ( 'NONE', #29719, #107907, #3100, .T. ) ;
#45301 = EDGE_LOOP ( 'NONE', ( #106001, #66241, #78393, #74263 ) ) ;
#45302 = EDGE_CURVE ( 'NONE', #111299, #116195, #45474, .T. ) ;
#45303 = LINE ( 'NONE', #7279, #102298 ) ;
#45304 = EDGE_CURVE ( 'NONE', #71756, #117403, #41267, .T. ) ;
#45305 = EDGE_CURVE ( 'NONE', #23899, #98477, #32959, .T. ) ;
#45306 = DIRECTION ( 'NONE',  ( -0.000000000000000000, 1.000000000000000000, -0.000000000000000000 ) ) ;
#45307 = PLANE ( 'NONE',  #74377 ) ;
#45308 = DIRECTION ( 'NONE',  ( 0.000000000000000000, 0.000000000000000000, 1.000000000000000000 ) ) ;
#45309 = LINE ( 'NONE', #76047, #43368 ) ;
#45310 = VERTEX_POINT ( 'NONE', #81642 ) ;
#45311 = ADVANCED_FACE ( 'NONE', ( #33216 ), #120676, .T. ) ;
#45312 = LINE ( 'NONE', #115292, #118731 ) ;
#45313 = EDGE_LOOP ( 'NONE', ( #27610, #42648, #128827, #4034 ) ) ;
#45315 = ORIENTED_EDGE ( 'NONE', *, *, #121508, .T. ) ;
#45314 = AXIS2_PLACEMENT_3D ( 'NONE', #30162, #70075, #59638 ) ;
#45316 = EDGE_LOOP ( 'NONE', ( #100224, #128356 ) ) ;
#45317 = AXIS2_PLACEMENT_3D ( 'NONE', #18927, #9123, #49069 ) ;
#45318 = LINE ( 'NONE', #23739, #56854 ) ;
#45319 = ORIENTED_EDGE ( 'NONE', *, *, #84897, .F. ) ;
#45320 = EDGE_LOOP ( 'NONE', ( #120747, #36185, #81592, #31266 ) ) ;
#45321 = EDGE_LOOP ( 'NONE', ( #42238, #3979 ) ) ;
#45322 = DIRECTION ( 'NONE',  ( -1.000000000000000000, 0.000000000000000000, -0.000000000000000000 ) ) ;
#45324 = CONICAL_SURFACE ( 'NONE', #13902, 0.09999999999999982514, 0.003490658503988666988 ) ;
#45323 = AXIS2_PLACEMENT_3D ( 'NONE', #51168, #89785, #119244 ) ;
#45325 = DIRECTION ( 'NONE',  ( 0.000000000000000000, 0.000000000000000000, 1.000000000000000000 ) ) ;
#45326 = DIRECTION ( 'NONE',  ( 0.000000000000000000, 0.000000000000000000, 1.000000000000000000 ) ) ;
#45327 = DIRECTION ( 'NONE',  ( 0.000000000000000000, 0.000000000000000000, 1.000000000000000000 ) ) ;
#45328 = CARTESIAN_POINT ( 'NONE',  ( 5.399999999999932854, 2.500000000000000000, 5.122947341949749323 ) ) ;
#45329 = DIRECTION ( 'NONE',  ( 0.000000000000000000, 0.000000000000000000, 1.000000000000000000 ) ) ;
#45330 = ORIENTED_EDGE ( 'NONE', *, *, #122387, .T. ) ;
#45331 = VECTOR ( 'NONE', #35465, 1000.000000000000000 ) ;
#45332 = CARTESIAN_POINT ( 'NONE',  ( 9.549999999999915445, 12.50000000000000000, -2.165063509461101710 ) ) ;
#45334 = CONICAL_SURFACE ( 'NONE', #97638, 0.1000000000000000472, 0.003490658503988666988 ) ;
#45333 = AXIS2_PLACEMENT_3D ( 'NONE', #69472, #109403, #11195 ) ;
#45335 = ORIENTED_EDGE ( 'NONE', *, *, #12200, .F. ) ;
#45336 = DIRECTION ( 'NONE',  ( 0.000000000000000000, 1.000000000000000000, 0.000000000000000000 ) ) ;
#45337 = CIRCLE ( 'NONE', #118468, 0.06509327318403745899 ) ;
#45338 = ORIENTED_EDGE ( 'NONE', *, *, #111132, .T. ) ;
#45339 = CARTESIAN_POINT ( 'NONE',  ( 185.9895833340161175, -4.445597072760145707, -7.699999999999951328 ) ) ;
#45340 = ORIENTED_EDGE ( 'NONE', *, *, #121149, .T. ) ;
#45341 = ORIENTED_EDGE ( 'NONE', *, *, #77573, .F. ) ;
#45342 = DIRECTION ( 'NONE',  ( 0.000000000000000000, 0.000000000000000000, 1.000000000000000000 ) ) ;
#45343 = DIRECTION ( 'NONE',  ( 0.000000000000000000, -0.9999939076577903929, 0.003490651415223739937 ) ) ;
#45344 = EDGE_CURVE ( 'NONE', #112557, #97087, #114399, .T. ) ;
#45345 = DIRECTION ( 'NONE',  ( 0.000000000000000000, 1.000000000000000000, 0.000000000000000000 ) ) ;
#45346 = ADVANCED_FACE ( 'NONE', ( #74410 ), #85152, .T. ) ;
#45347 = CARTESIAN_POINT ( 'NONE',  ( -12.89999999999999147, 2.500000000000000000, 5.022947341949748790 ) ) ;
#45348 = ORIENTED_EDGE ( 'NONE', *, *, #20031, .T. ) ;
#45349 = CARTESIAN_POINT ( 'NONE',  ( -1.700000000000035261, 2.500000000000000000, 4.330127018922196314 ) ) ;
#45350 = FACE_OUTER_BOUND ( 'NONE', #106754, .T. ) ;
#45351 = DIRECTION ( 'NONE',  ( 0.000000000000000000, 0.000000000000000000, -1.000000000000000000 ) ) ;
#45352 = AXIS2_PLACEMENT_3D ( 'NONE', #73126, #82312, #122237 ) ;
#45353 = DIRECTION ( 'NONE',  ( -0.000000000000000000, 1.000000000000000000, -0.000000000000000000 ) ) ;
#45354 = CONICAL_SURFACE ( 'NONE', #18433, 0.1000000000000002554, 0.003490658503988666988 ) ;
#45355 = ADVANCED_FACE ( 'NONE', ( #84214 ), #28742, .T. ) ;
#45356 = DIRECTION ( 'NONE',  ( 0.000000000000000000, 0.000000000000000000, 1.000000000000000000 ) ) ;
#45357 = ORIENTED_EDGE ( 'NONE', *, *, #58471, .T. ) ;
#45358 = EDGE_CURVE ( 'NONE', #99447, #104181, #64226, .T. ) ;
#45359 = CIRCLE ( 'NONE', #110192, 0.09999999999999982514 ) ;
#45360 = EDGE_LOOP ( 'NONE', ( #14549, #21692 ) ) ;
#45361 = CIRCLE ( 'NONE', #1419, 0.06509327318403745899 ) ;
#45362 = EDGE_LOOP ( 'NONE', ( #39311, #95013 ) ) ;
#45363 = CONICAL_SURFACE ( 'NONE', #89263, 0.1000000000000002554, 0.003490658503988666988 ) ;
#45364 = DIRECTION ( 'NONE',  ( 0.000000000000000000, -0.9999939076577903929, 0.003490651415223739937 ) ) ;
#45365 = DIRECTION ( 'NONE',  ( -0.000000000000000000, 1.000000000000000000, -0.000000000000000000 ) ) ;
#45366 = AXIS2_PLACEMENT_3D ( 'NONE', #127150, #19086, #6681 ) ;
#45367 = CARTESIAN_POINT ( 'NONE',  ( 183.9635416670080872, -4.367472073101519747, 7.564683531249999149 ) ) ;
#45369 = AXIS2_PLACEMENT_3D ( 'NONE', #13715, #1324, #22284 ) ;
#45368 = CARTESIAN_POINT ( 'NONE',  ( 8.749999999999920064, 2.500000000000000000, 5.702370205355745014 ) ) ;
#45370 = CARTESIAN_POINT ( 'NONE',  ( 4.349999999999941025, 12.50000000000000000, -6.148780366869526226 ) ) ;
#45371 = CARTESIAN_POINT ( 'NONE',  ( 9.999999999999911182, 12.50000000000000000, -3.637306695894650055 ) ) ;
#45372 = CARTESIAN_POINT ( 'NONE',  ( 0.4499999999999569344, 2.500000000000000000, -2.265063509461101798 ) ) ;
#45373 = EDGE_LOOP ( 'NONE', ( #103381, #54213 ) ) ;
#45374 = AXIS2_PLACEMENT_3D ( 'NONE', #110739, #30917, #81922 ) ;
#45376 = AXIS2_PLACEMENT_3D ( 'NONE', #14343, #14970, #54286 ) ;
#45375 = AXIS2_PLACEMENT_3D ( 'NONE', #30514, #70414, #91984 ) ;
#45377 = DIRECTION ( 'NONE',  ( 0.000000000000000000, 0.000000000000000000, -1.000000000000000000 ) ) ;
#45378 = CARTESIAN_POINT ( 'NONE',  ( 3.349999999999943689, 12.50000000000000000, 1.407149913249508000 ) ) ;
#45379 = EDGE_LOOP ( 'NONE', ( #48731, #41530, #3680, #90186 ) ) ;
#45380 = DIRECTION ( 'NONE',  ( 0.000000000000000000, 1.000000000000000000, 0.000000000000000000 ) ) ;
#45381 = DIRECTION ( 'NONE',  ( -0.000000000000000000, -1.000000000000000000, -0.000000000000000000 ) ) ;
#45382 = DIRECTION ( 'NONE',  ( 0.000000000000000000, 0.000000000000000000, 1.000000000000000000 ) ) ;
#45383 = EDGE_CURVE ( 'NONE', #37632, #117649, #92102, .T. ) ;
#45384 = ORIENTED_EDGE ( 'NONE', *, *, #47244, .F. ) ;
#45385 = CARTESIAN_POINT ( 'NONE',  ( 0.7999999999999553024, 12.50000000000000000, -4.330127018922201643 ) ) ;
#45386 = EDGE_LOOP ( 'NONE', ( #16739, #25568, #61996, #76980 ) ) ;
#45387 = CARTESIAN_POINT ( 'NONE',  ( 0.3999999999999628852, 12.50000000000000000, 0.6928203230275518099 ) ) ;
#45388 = DIRECTION ( 'NONE',  ( 0.000000000000000000, 0.000000000000000000, 1.000000000000000000 ) ) ;
#45389 = AXIS2_PLACEMENT_3D ( 'NONE', #114966, #102574, #12891 ) ;
#45390 = DIRECTION ( 'NONE',  ( 0.000000000000000000, 0.000000000000000000, 1.000000000000000000 ) ) ;
#45391 = ORIENTED_EDGE ( 'NONE', *, *, #5232, .F. ) ;
#45392 = CARTESIAN_POINT ( 'NONE',  ( 185.7812500006828031, 0.000000000000000000, 7.700000000000000178 ) ) ;
#45393 = CARTESIAN_POINT ( 'NONE',  ( -7.500000000000001776, -1.500000000000000000, -8.999999999999998224 ) ) ;
#45394 = EDGE_CURVE ( 'NONE', #62921, #64709, #3594, .T. ) ;
#45395 = EDGE_CURVE ( 'NONE', #73490, #72875, #54124, .T. ) ;
#45396 = EDGE_LOOP ( 'NONE', ( #89023, #103520 ) ) ;
#45397 = DIRECTION ( 'NONE',  ( 0.000000000000000000, 0.000000000000000000, 1.000000000000000000 ) ) ;
#45398 = CIRCLE ( 'NONE', #32892, 0.06509327318403745899 ) ;
#45399 = ORIENTED_EDGE ( 'NONE', *, *, #8203, .T. ) ;
#45400 = CIRCLE ( 'NONE', #126875, 0.06509327318403741736 ) ;
#45401 = EDGE_LOOP ( 'NONE', ( #110759, #18667 ) ) ;
#45402 = DIRECTION ( 'NONE',  ( -0.000000000000000000, 1.000000000000000000, -0.000000000000000000 ) ) ;
#45403 = DIRECTION ( 'NONE',  ( 0.000000000000000000, 1.000000000000000000, 0.000000000000000000 ) ) ;
#45404 = EDGE_CURVE ( 'NONE', #116963, #111573, #95627, .T. ) ;
#45405 = ORIENTED_EDGE ( 'NONE', *, *, #116811, .T. ) ;
#45406 = CARTESIAN_POINT ( 'NONE',  ( -4.150000000000025224, 2.500000000000000000, 2.857883832488649301 ) ) ;
#45407 = PLANE ( 'NONE',  #69388 ) ;
#45408 = EDGE_LOOP ( 'NONE', ( #45938, #82088 ) ) ;
#45410 = CIRCLE ( 'NONE', #126972, 0.06509327318403745899 ) ;
#45409 = AXIS2_PLACEMENT_3D ( 'NONE', #126342, #47781, #125672 ) ;
#45411 = DIRECTION ( 'NONE',  ( 0.000000000000000000, -0.9999939076577903929, 0.003490651415223739937 ) ) ;
#45412 = CARTESIAN_POINT ( 'NONE',  ( 2.499999999999945377, 2.500000000000000000, 4.922947341949748257 ) ) ;
#45413 = CARTESIAN_POINT ( 'NONE',  ( -2.300000000000033129, 2.500000000000000000, 3.983716857408420076 ) ) ;
#45414 = DIRECTION ( 'NONE',  ( 0.000000000000000000, -0.000000000000000000, 1.000000000000000000 ) ) ;
#45415 = DIRECTION ( 'NONE',  ( -0.000000000000000000, 1.000000000000000000, -0.000000000000000000 ) ) ;
#45416 = CARTESIAN_POINT ( 'NONE',  ( 185.0729166673495172, 4.445597072760072876, -7.700000000000080114 ) ) ;
#45418 = AXIS2_PLACEMENT_3D ( 'NONE', #73245, #123616, #113163 ) ;
#45417 = AXIS2_PLACEMENT_3D ( 'NONE', #61936, #122779, #41020 ) ;
#45419 = AXIS2_PLACEMENT_3D ( 'NONE', #37538, #109490, #22418 ) ;
#45420 = EDGE_LOOP ( 'NONE', ( #55312, #38874 ) ) ;
#45421 = VERTEX_POINT ( 'NONE', #42377 ) ;
#45422 = EDGE_LOOP ( 'NONE', ( #79997, #77685 ) ) ;
#45423 = ORIENTED_EDGE ( 'NONE', *, *, #75701, .T. ) ;
#45424 = CARTESIAN_POINT ( 'NONE',  ( 7.299999999999927880, 12.50000000000000000, -4.676537180435977881 ) ) ;
#45425 = LINE ( 'NONE', #127209, #34525 ) ;
#45426 = DIRECTION ( 'NONE',  ( -0.000000000000000000, 1.000000000000000000, -0.000000000000000000 ) ) ;
#45427 = ORIENTED_EDGE ( 'NONE', *, *, #17652, .T. ) ;
#45428 = FACE_BOUND ( 'NONE', #9710, .T. ) ;
#45429 = CARTESIAN_POINT ( 'NONE',  ( 4.599999999999938360, 2.500000000000000000, -2.276824562219559311E-15 ) ) ;
#45430 = DIRECTION ( 'NONE',  ( 0.000000000000000000, -0.000000000000000000, 1.000000000000000000 ) ) ;
#45432 = EDGE_CURVE ( 'NONE', #38961, #58403, #78923, .T. ) ;
#45431 = DIRECTION ( 'NONE',  ( -0.000000000000000000, 1.000000000000000000, -0.000000000000000000 ) ) ;
#45433 = DIRECTION ( 'NONE',  ( -0.000000000000000000, -1.000000000000000000, -0.000000000000000000 ) ) ;
#45434 = DIRECTION ( 'NONE',  ( 0.000000000000000000, 0.000000000000000000, -1.000000000000000000 ) ) ;
#45435 = CARTESIAN_POINT ( 'NONE',  ( 3.349999999999945466, 2.500000000000000000, -2.757883832488654097 ) ) ;
#45436 = CARTESIAN_POINT ( 'NONE',  ( -3.350000000000028955, 2.500000000000000000, 5.802370205355744659 ) ) ;
#45437 = CARTESIAN_POINT ( 'NONE',  ( 3.149999999999942624, 12.50000000000000000, 6.213873640053559022 ) ) ;
#45438 = EDGE_CURVE ( 'NONE', #100139, #112224, #110211, .T. ) ;
#45439 = DIRECTION ( 'NONE',  ( 0.000000000000000000, 0.000000000000000000, -1.000000000000000000 ) ) ;
#45440 = EDGE_CURVE ( 'NONE', #19106, #60583, #39229, .T. ) ;
#45441 = AXIS2_PLACEMENT_3D ( 'NONE', #8543, #48492, #98873 ) ;
#45442 = ADVANCED_FACE ( 'NONE', ( #56675 ), #108238, .T. ) ;
#45443 = CONICAL_SURFACE ( 'NONE', #103926, 0.1000000000000002554, 0.003490658503988666988 ) ;
#45444 = DIRECTION ( 'NONE',  ( 0.000000000000000000, 0.000000000000000000, 1.000000000000000000 ) ) ;
#45445 = VERTEX_POINT ( 'NONE', #67130 ) ;
#45447 = ORIENTED_EDGE ( 'NONE', *, *, #33778, .T. ) ;
#45446 = AXIS2_PLACEMENT_3D ( 'NONE', #99779, #50057, #8797 ) ;
#45448 = EDGE_LOOP ( 'NONE', ( #28563, #26857 ) ) ;
#45449 = ORIENTED_EDGE ( 'NONE', *, *, #119415, .F. ) ;
#45450 = CARTESIAN_POINT ( 'NONE',  ( -2.300000000000033129, 12.50000000000000000, 4.048810130592458201 ) ) ;
#45451 = ADVANCED_FACE ( 'NONE', ( #46231 ), #68525, .T. ) ;
#45452 = ORIENTED_EDGE ( 'NONE', *, *, #56592, .T. ) ;
#45454 = EDGE_CURVE ( 'NONE', #37705, #77073, #26601, .T. ) ;
#45453 = DIRECTION ( 'NONE',  ( -0.000000000000000000, 1.000000000000000000, -0.000000000000000000 ) ) ;
#45456 = ORIENTED_EDGE ( 'NONE', *, *, #71743, .T. ) ;
#45455 = EDGE_CURVE ( 'NONE', #102121, #116823, #66460, .T. ) ;
#45458 = ORIENTED_EDGE ( 'NONE', *, *, #126112, .F. ) ;
#45457 = AXIS2_PLACEMENT_3D ( 'NONE', #101125, #30473, #11450 ) ;
#45460 = AXIS2_PLACEMENT_3D ( 'NONE', #57334, #76974, #124789 ) ;
#45459 = DIRECTION ( 'NONE',  ( 0.000000000000000000, 1.000000000000000000, 0.000000000000000000 ) ) ;
#45461 = CONICAL_SURFACE ( 'NONE', #97920, 0.09999999999999999167, 0.003490658503988666988 ) ;
#45462 = CONICAL_SURFACE ( 'NONE', #118593, 0.1000000000000000056, 0.003490658503988666988 ) ;
#45463 = EDGE_CURVE ( 'NONE', #89563, #38596, #28831, .T. ) ;
#45464 = CARTESIAN_POINT ( 'NONE',  ( 3.709550432165976463, -1.499999999999871880, 10.00000000000000178 ) ) ;
#45465 = DIRECTION ( 'NONE',  ( 0.000000000000000000, 0.000000000000000000, -1.000000000000000000 ) ) ;
#45466 = LINE ( 'NONE', #112902, #71921 ) ;
#45467 = CARTESIAN_POINT ( 'NONE',  ( -11.64999999999999680, 2.500000000000000000, 6.595190528383296780 ) ) ;
#45468 = AXIS2_PLACEMENT_3D ( 'NONE', #12273, #60750, #103252 ) ;
#45469 = EDGE_CURVE ( 'NONE', #118395, #69772, #43424, .T. ) ;
#45470 = ORIENTED_EDGE ( 'NONE', *, *, #120822, .T. ) ;
#45471 = EDGE_CURVE ( 'NONE', #73598, #112989, #83207, .T. ) ;
#45472 = EDGE_LOOP ( 'NONE', ( #88011, #81400 ) ) ;
#45474 = CIRCLE ( 'NONE', #116453, 0.1000000000000002554 ) ;
#45473 = AXIS2_PLACEMENT_3D ( 'NONE', #42249, #12758, #2965 ) ;
#45475 = ORIENTED_EDGE ( 'NONE', *, *, #31336, .F. ) ;
#45477 = EDGE_LOOP ( 'NONE', ( #8032, #59705 ) ) ;
#45476 = CARTESIAN_POINT ( 'NONE',  ( 1.849999999999948130, 12.50000000000000000, 6.148780366869520009 ) ) ;
#45478 = CARTESIAN_POINT ( 'NONE',  ( 6.049999999999932321, 12.50000000000000000, 1.753560074763284016 ) ) ;
#45479 = ORIENTED_EDGE ( 'NONE', *, *, #24025, .F. ) ;
#45480 = EDGE_LOOP ( 'NONE', ( #75008, #48026 ) ) ;
#45481 = CARTESIAN_POINT ( 'NONE',  ( 13.34999999999990017, 12.50000000000000000, 1.472243186433545459 ) ) ;
#45482 = CARTESIAN_POINT ( 'NONE',  ( -10.84999999999999964, 12.50000000000000000, 5.737276932171707422 ) ) ;
#45483 = CARTESIAN_POINT ( 'NONE',  ( 12.49999999999993960, 2.500000000000000000, -4.330127018922201643 ) ) ;
#45484 = CARTESIAN_POINT ( 'NONE',  ( 187.3906250003414016, 0.000000000000000000, 7.700000000000000178 ) ) ;
#45485 = LINE ( 'NONE', #46111, #25219 ) ;
#45486 = LINE ( 'NONE', #118067, #28872 ) ;
#45487 = AXIS2_PLACEMENT_3D ( 'NONE', #20019, #99867, #58653 ) ;
#45488 = ORIENTED_EDGE ( 'NONE', *, *, #54287, .F. ) ;
#45489 = CARTESIAN_POINT ( 'NONE',  ( -5.200000000000020606, 2.500000000000000000, -0.3464101615137782364 ) ) ;
#45490 = ORIENTED_EDGE ( 'NONE', *, *, #79718, .T. ) ;
#45491 = DIRECTION ( 'NONE',  ( 0.000000000000000000, 0.000000000000000000, 1.000000000000000000 ) ) ;
#45492 = ORIENTED_EDGE ( 'NONE', *, *, #117204, .F. ) ;
#45493 = CARTESIAN_POINT ( 'NONE',  ( 7.299999999999926104, 12.50000000000000000, -3.983716857408426293 ) ) ;
#45494 = CARTESIAN_POINT ( 'NONE',  ( -13.29999999999999005, 12.50000000000000000, -4.330127018922198978 ) ) ;
#45495 = ORIENTED_EDGE ( 'NONE', *, *, #121628, .F. ) ;
#45496 = CARTESIAN_POINT ( 'NONE',  ( -9.200000000000006395, 2.500000000000000000, 4.230127018922196669 ) ) ;
#45497 = DIRECTION ( 'NONE',  ( 0.000000000000000000, 1.000000000000000000, 0.000000000000000000 ) ) ;
#45498 = ORIENTED_EDGE ( 'NONE', *, *, #2482, .T. ) ;
#45499 = SURFACE_STYLE_FILL_AREA ( #95876 ) ;
#45500 = CIRCLE ( 'NONE', #9973, 0.1000000000000002554 ) ;
#45501 = EDGE_CURVE ( 'NONE', #31560, #47494, #51817, .T. ) ;
#45502 = AXIS2_PLACEMENT_3D ( 'NONE', #11379, #2194, #32979 ) ;
#45503 = CARTESIAN_POINT ( 'NONE',  ( 6.249999999999967137, 2.500000000000000000, 6.495190528383297135 ) ) ;
#45504 = EDGE_CURVE ( 'NONE', #61083, #1993, #91516, .T. ) ;
#45505 = EDGE_LOOP ( 'NONE', ( #32616, #25892, #24240, #2222 ) ) ;
#45506 = EDGE_LOOP ( 'NONE', ( #65147, #47945 ) ) ;
#45507 = ORIENTED_EDGE ( 'NONE', *, *, #44377, .T. ) ;
#45508 = DIRECTION ( 'NONE',  ( 0.000000000000000000, 1.846105847067148761E-16, 1.000000000000000000 ) ) ;
#45509 = CARTESIAN_POINT ( 'NONE',  ( 8.349999999999919709, 12.50000000000000000, -2.165063509461101710 ) ) ;
#45510 = CARTESIAN_POINT ( 'NONE',  ( 184.8593750003413732, 0.000000000000000000, 7.564683531250000925 ) ) ;
#45511 = DIRECTION ( 'NONE',  ( -4.274815082592931898E-19, -0.9999939076577903929, -0.003490651415223739937 ) ) ;
#45512 = VECTOR ( 'NONE', #99468, 1000.000000000000000 ) ;
#45513 = CIRCLE ( 'NONE', #7827, 0.09999999999999982514 ) ;
#45514 = FACE_OUTER_BOUND ( 'NONE', #25490, .T. ) ;
#45515 = CARTESIAN_POINT ( 'NONE',  ( 179.5000000000000000, 0.000000000000000000, 0.000000000000000000 ) ) ;
#45516 = VERTEX_POINT ( 'NONE', #49481 ) ;
#45517 = CARTESIAN_POINT ( 'NONE',  ( 21.24754738303297330, 0.7337760880902002292, -4.182111650399407132 ) ) ;
#45518 = AXIS2_PLACEMENT_3D ( 'NONE', #18998, #58951, #106740 ) ;
#45519 = ORIENTED_EDGE ( 'NONE', *, *, #89578, .F. ) ;
#45520 = CIRCLE ( 'NONE', #110538, 0.1000000000000002554 ) ;
#45521 = CARTESIAN_POINT ( 'NONE',  ( 11.44999999999990514, 2.500000000000000000, 2.611473670974873151 ) ) ;
#45522 = FACE_OUTER_BOUND ( 'NONE', #108678, .T. ) ;
#45523 = DIRECTION ( 'NONE',  ( -0.000000000000000000, 1.000000000000000000, -0.000000000000000000 ) ) ;
#45524 = ORIENTED_EDGE ( 'NONE', *, *, #46331, .F. ) ;
#45525 = DIRECTION ( 'NONE',  ( 0.000000000000000000, 0.000000000000000000, -1.000000000000000000 ) ) ;
#45526 = CARTESIAN_POINT ( 'NONE',  ( -12.49999999999999467, 12.50000000000000000, 0.6277270498435161272 ) ) ;
#45527 = AXIS2_PLACEMENT_3D ( 'NONE', #103074, #53343, #72974 ) ;
#45528 = VECTOR ( 'NONE', #106603, 1000.000000000000000 ) ;
#45529 = ORIENTED_EDGE ( 'NONE', *, *, #38213, .T. ) ;
#45530 = AXIS2_PLACEMENT_3D ( 'NONE', #128793, #10282, #107834 ) ;
#45531 = CARTESIAN_POINT ( 'NONE',  ( 10.84999999999991260, 2.500000000000000000, 6.495190528383297135 ) ) ;
#45532 = ADVANCED_FACE ( 'NONE', ( #70391 ), #35096, .T. ) ;
#45533 = AXIS2_PLACEMENT_3D ( 'NONE', #70320, #90588, #40881 ) ;
#45534 = EDGE_LOOP ( 'NONE', ( #42240, #108933 ) ) ;
#45535 = ORIENTED_EDGE ( 'NONE', *, *, #11883, .F. ) ;
#45536 = CARTESIAN_POINT ( 'NONE',  ( 11.44999999999991047, 12.50000000000000000, -2.576566944158915184 ) ) ;
#45537 = VECTOR ( 'NONE', #19841, 1000.000000000000000 ) ;
#45538 = VERTEX_POINT ( 'NONE', #58003 ) ;
#45539 = DIRECTION ( 'NONE',  ( -0.000000000000000000, 1.000000000000000000, -0.000000000000000000 ) ) ;
#45540 = CARTESIAN_POINT ( 'NONE',  ( 11.04999999999990656, 2.500000000000000000, 2.611473670974873151 ) ) ;
#45541 = CONICAL_SURFACE ( 'NONE', #41349, 0.1000000000000002554, 0.003490658503988666988 ) ;
#45542 = DIRECTION ( 'NONE',  ( 0.000000000000000000, 0.000000000000000000, -1.000000000000000000 ) ) ;
#45543 = EDGE_CURVE ( 'NONE', #40133, #105571, #129336, .T. ) ;
#45544 = ORIENTED_EDGE ( 'NONE', *, *, #29329, .T. ) ;
#45545 = CIRCLE ( 'NONE', #108226, 0.1000000000000002554 ) ;
#45546 = FACE_BOUND ( 'NONE', #114843, .T. ) ;
#45548 = VERTEX_POINT ( 'NONE', #39029 ) ;
#45547 = CARTESIAN_POINT ( 'NONE',  ( 6.849999999999929479, 12.50000000000000000, -1.883746621131363597 ) ) ;
#45549 = EDGE_CURVE ( 'NONE', #8757, #59390, #8234, .T. ) ;
#45550 = CARTESIAN_POINT ( 'NONE',  ( -8.749999999999971578, 2.500000000000000000, 6.595190528383296780 ) ) ;
#45551 = AXIS2_PLACEMENT_3D ( 'NONE', #13564, #25984, #85537 ) ;
#45552 = DIRECTION ( 'NONE',  ( 0.000000000000000000, -0.9999939076577903929, 0.003490651415223739937 ) ) ;
#45553 = EDGE_CURVE ( 'NONE', #107210, #18914, #33048, .T. ) ;
#45554 = VERTEX_POINT ( 'NONE', #10186 ) ;
#45555 = AXIS2_PLACEMENT_3D ( 'NONE', #89390, #67805, #118839 ) ;
#45556 = EDGE_LOOP ( 'NONE', ( #57358, #29835, #105495, #97352 ) ) ;
#45557 = ORIENTED_EDGE ( 'NONE', *, *, #118530, .F. ) ;
#45558 = CARTESIAN_POINT ( 'NONE',  ( -0.8000000000000376810, 12.50000000000000000, -4.330127018922201643 ) ) ;
#45559 = DIRECTION ( 'NONE',  ( 0.000000000000000000, 1.000000000000000000, 0.000000000000000000 ) ) ;
#45560 = DIRECTION ( 'NONE',  ( -0.000000000000000000, 1.000000000000000000, -0.000000000000000000 ) ) ;
#45561 = EDGE_CURVE ( 'NONE', #43214, #75247, #108374, .T. ) ;
#45562 = FACE_BOUND ( 'NONE', #107307, .T. ) ;
#45563 = ORIENTED_EDGE ( 'NONE', *, *, #15513, .T. ) ;
#45564 = CARTESIAN_POINT ( 'NONE',  ( 184.9843750003414016, -8.734944146203032389, -1.604583208406768146E-15 ) ) ;
#45565 = DIRECTION ( 'NONE',  ( 0.000000000000000000, -0.9999939076577903929, 0.003490651415223739937 ) ) ;
#45566 = DIRECTION ( 'NONE',  ( 0.000000000000000000, 0.000000000000000000, 1.000000000000000000 ) ) ;
#45567 = DIRECTION ( 'NONE',  ( 0.000000000000000000, 1.000000000000000000, -0.000000000000000000 ) ) ;
#45568 = DIRECTION ( 'NONE',  ( 1.000000000000000000, 0.000000000000000000, 0.000000000000000000 ) ) ;
#45569 = LINE ( 'NONE', #94642, #126287 ) ;
#45570 = DIRECTION ( 'NONE',  ( 0.000000000000000000, 0.000000000000000000, 1.000000000000000000 ) ) ;
#45571 = CARTESIAN_POINT ( 'NONE',  ( 149.5981739382431783, 2.500000000000000000, -1.703575533167231537 ) ) ;
#45572 = DIRECTION ( 'NONE',  ( 0.000000000000000000, 0.000000000000000000, 1.000000000000000000 ) ) ;
#45573 = EDGE_LOOP ( 'NONE', ( #108170, #71407, #22604, #722 ) ) ;
#45574 = ORIENTED_EDGE ( 'NONE', *, *, #42146, .T. ) ;
#45575 = ORIENTED_EDGE ( 'NONE', *, *, #89777, .T. ) ;
#45576 = ORIENTED_EDGE ( 'NONE', *, *, #46746, .F. ) ;
#45577 = ORIENTED_EDGE ( 'NONE', *, *, #83843, .T. ) ;
#45578 = DIRECTION ( 'NONE',  ( 0.000000000000000000, 1.000000000000000000, 0.000000000000000000 ) ) ;
#45579 = DIRECTION ( 'NONE',  ( 0.000000000000000000, 0.000000000000000000, 1.000000000000000000 ) ) ;
#45580 = EDGE_LOOP ( 'NONE', ( #42985, #53183 ) ) ;
#45581 = FACE_BOUND ( 'NONE', #58031, .T. ) ;
#45582 = DIRECTION ( 'NONE',  ( 0.000000000000000000, 0.000000000000000000, -1.000000000000000000 ) ) ;
#45583 = AXIS2_PLACEMENT_3D ( 'NONE', #91824, #41456, #13239 ) ;
#45584 = ADVANCED_FACE ( 'NONE', ( #78295 ), #50125, .T. ) ;
#45585 = AXIS2_PLACEMENT_3D ( 'NONE', #121820, #81883, #73365 ) ;
#45586 = DIRECTION ( 'NONE',  ( 0.000000000000000000, 0.000000000000000000, 1.000000000000000000 ) ) ;
#45587 = ORIENTED_EDGE ( 'NONE', *, *, #116890, .T. ) ;
#45588 = CARTESIAN_POINT ( 'NONE',  ( 8.549999999999918998, 12.50000000000000000, -1.883746621131363597 ) ) ;
#45589 = CARTESIAN_POINT ( 'NONE',  ( -6.650000000000019007, 12.50000000000000000, -1.407149913249512663 ) ) ;
#45590 = EDGE_CURVE ( 'NONE', #20424, #79817, #18347, .T. ) ;
#45591 = DIRECTION ( 'NONE',  ( 0.000000000000000000, 0.000000000000000000, 1.000000000000000000 ) ) ;
#45592 = ORIENTED_EDGE ( 'NONE', *, *, #20772, .T. ) ;
#45593 = LINE ( 'NONE', #95969, #3320 ) ;
#45595 = ADVANCED_FACE ( 'NONE', ( #88741 ), #5811, .T. ) ;
#45594 = CIRCLE ( 'NONE', #116582, 0.06509327318403745899 ) ;
#45596 = ORIENTED_EDGE ( 'NONE', *, *, #112679, .F. ) ;
#45597 = CIRCLE ( 'NONE', #39354, 0.06509327318403745899 ) ;
#45598 = ORIENTED_EDGE ( 'NONE', *, *, #117527, .F. ) ;
#45599 = ORIENTED_EDGE ( 'NONE', *, *, #80366, .T. ) ;
#45600 = ADVANCED_FACE ( 'NONE', ( #118199 ), #99845, .T. ) ;
#45601 = DIRECTION ( 'NONE',  ( -4.274815082592931898E-19, -0.9999939076577903929, -0.003490651415223739937 ) ) ;
#45603 = EDGE_CURVE ( 'NONE', #73436, #38247, #78937, .T. ) ;
#45602 = DIRECTION ( 'NONE',  ( 0.000000000000000000, 0.000000000000000000, 1.000000000000000000 ) ) ;
#45604 = DIRECTION ( 'NONE',  ( 0.000000000000000000, 1.000000000000000000, 0.000000000000000000 ) ) ;
#45606 = ORIENTED_EDGE ( 'NONE', *, *, #8063, .T. ) ;
#45605 = EDGE_CURVE ( 'NONE', #79650, #102847, #124966, .T. ) ;
#45607 = CARTESIAN_POINT ( 'NONE',  ( 2.500000000000002220, 1.499999999999999556, -9.999999999999998224 ) ) ;
#45608 = EDGE_CURVE ( 'NONE', #48547, #128936, #57773, .T. ) ;
#45609 = CIRCLE ( 'NONE', #5763, 0.1000000000000002554 ) ;
#45610 = DIRECTION ( 'NONE',  ( -0.000000000000000000, 1.000000000000000000, -0.000000000000000000 ) ) ;
#45612 = ADVANCED_FACE ( 'NONE', ( #95757 ), #20416, .T. ) ;
#45611 = CARTESIAN_POINT ( 'NONE',  ( 6.849999999999929479, 2.500000000000000000, -1.818653347947326138 ) ) ;
#45613 = CARTESIAN_POINT ( 'NONE',  ( 186.7343750003414300, 8.734944146203032389, 5.348610694689227483E-16 ) ) ;
#45614 = CARTESIAN_POINT ( 'NONE',  ( -0.4000000000000392131, 2.500000000000000000, -4.330127018922201643 ) ) ;
#45615 = AXIS2_PLACEMENT_3D ( 'NONE', #98437, #99111, #76886 ) ;
#45616 = DIRECTION ( 'NONE',  ( 0.000000000000000000, 1.000000000000000000, 0.000000000000000000 ) ) ;
#45617 = ORIENTED_EDGE ( 'NONE', *, *, #59743, .T. ) ;
#45618 = DIRECTION ( 'NONE',  ( -0.000000000000000000, 1.000000000000000000, -0.000000000000000000 ) ) ;
#45619 = EDGE_CURVE ( 'NONE', #119267, #18141, #37496, .T. ) ;
#45620 = CIRCLE ( 'NONE', #106154, 0.09999999999999982514 ) ;
#45621 = ORIENTED_EDGE ( 'NONE', *, *, #70105, .T. ) ;
#45622 = ORIENTED_EDGE ( 'NONE', *, *, #36899, .T. ) ;
#45623 = CIRCLE ( 'NONE', #118765, 0.06509327318403745899 ) ;
#45624 = CARTESIAN_POINT ( 'NONE',  ( 3.549999999999942979, 12.50000000000000000, 1.818653347947321475 ) ) ;
#45625 = DIRECTION ( 'NONE',  ( 0.000000000000000000, 0.000000000000000000, -1.000000000000000000 ) ) ;
#45626 = DIRECTION ( 'NONE',  ( 0.000000000000000000, -0.9999939076577903929, 0.003490651415223739937 ) ) ;
#45627 = VECTOR ( 'NONE', #115450, 1000.000000000000000 ) ;
#45628 = ORIENTED_EDGE ( 'NONE', *, *, #11140, .T. ) ;
#45629 = AXIS2_PLACEMENT_3D ( 'NONE', #33401, #1336, #72032 ) ;
#45630 = ORIENTED_EDGE ( 'NONE', *, *, #88516, .F. ) ;
#45631 = DIRECTION ( 'NONE',  ( 0.000000000000000000, 0.000000000000000000, -1.000000000000000000 ) ) ;
#45632 = CIRCLE ( 'NONE', #3847, 0.1000000000000000472 ) ;
#45633 = CARTESIAN_POINT ( 'NONE',  ( 0.3999999999999563904, 2.500000000000000000, 4.922947341949748257 ) ) ;
#45634 = CARTESIAN_POINT ( 'NONE',  ( 3.949999999999941558, 2.500000000000000000, -1.818653347947326138 ) ) ;
#45635 = ORIENTED_EDGE ( 'NONE', *, *, #13818, .F. ) ;
#45636 = ORIENTED_EDGE ( 'NONE', *, *, #5948, .F. ) ;
#45637 = DIRECTION ( 'NONE',  ( 0.000000000000000000, -0.9999939076577903929, 0.003490651415223739937 ) ) ;
#45638 = AXIS2_PLACEMENT_3D ( 'NONE', #114646, #106755, #37398 ) ;
#45639 = ORIENTED_EDGE ( 'NONE', *, *, #27946, .T. ) ;
#45640 = CARTESIAN_POINT ( 'NONE',  ( 0.5999999999999560130, 2.500000000000000000, -3.983716857408426293 ) ) ;
#45641 = CARTESIAN_POINT ( 'NONE',  ( 7.099999999999927702, 12.50000000000000000, -3.702399969078687292 ) ) ;
#45642 = ORIENTED_EDGE ( 'NONE', *, *, #61565, .T. ) ;
#45643 = DIRECTION ( 'NONE',  ( 0.000000000000000000, -0.000000000000000000, 1.000000000000000000 ) ) ;
#45644 = DIRECTION ( 'NONE',  ( 0.000000000000000000, 0.000000000000000000, 1.000000000000000000 ) ) ;
#45645 = CARTESIAN_POINT ( 'NONE',  ( -3.470671598752761919E-14, 2.500000000000000000, -0.7928203230275518987 ) ) ;
#45646 = CIRCLE ( 'NONE', #60323, 0.1000000000000002554 ) ;
#45647 = DIRECTION ( 'NONE',  ( 0.000000000000000000, -0.9999939076577903929, 0.003490651415223739937 ) ) ;
#45648 = ORIENTED_EDGE ( 'NONE', *, *, #50733, .T. ) ;
#45649 = CARTESIAN_POINT ( 'NONE',  ( 13.34999999999990017, 12.50000000000000000, 1.472243186433545459 ) ) ;
#45650 = AXIS2_PLACEMENT_3D ( 'NONE', #20420, #58425, #59722 ) ;
#45651 = ADVANCED_FACE ( 'NONE', ( #38125 ), #8008, .T. ) ;
#45652 = DIRECTION ( 'NONE',  ( -0.000000000000000000, -1.000000000000000000, -0.000000000000000000 ) ) ;
#45653 = ORIENTED_EDGE ( 'NONE', *, *, #15812, .F. ) ;
#45654 = ORIENTED_EDGE ( 'NONE', *, *, #121981, .F. ) ;
#45655 = CARTESIAN_POINT ( 'NONE',  ( 184.0885416670080872, -6.551208109652273848, -3.782341765625003571 ) ) ;
#45656 = FACE_OUTER_BOUND ( 'NONE', #127324, .T. ) ;
#45657 = DIRECTION ( 'NONE',  ( 0.000000000000000000, 0.000000000000000000, -1.000000000000000000 ) ) ;
#45658 = CARTESIAN_POINT ( 'NONE',  ( 14.14999999999989377, 12.50000000000000000, -2.857883832488653741 ) ) ;
#45659 = CARTESIAN_POINT ( 'NONE',  ( -7.100000000000013856, 2.500000000000000000, 3.537306695894645081 ) ) ;
#45660 = CARTESIAN_POINT ( 'NONE',  ( 0.3999999999999568345, 2.500000000000000000, -5.122947341949753763 ) ) ;
#45661 = EDGE_CURVE ( 'NONE', #47460, #63253, #76855, .T. ) ;
#45662 = LINE ( 'NONE', #116306, #9357 ) ;
#45663 = FACE_OUTER_BOUND ( 'NONE', #111902, .T. ) ;
#45664 = DIRECTION ( 'NONE',  ( 0.000000000000000000, 0.000000000000000000, 1.000000000000000000 ) ) ;
#45665 = CONICAL_SURFACE ( 'NONE', #110489, 0.1000000000000002554, 0.003490658503988666988 ) ;
#45666 = DIRECTION ( 'NONE',  ( 0.000000000000000000, 0.000000000000000000, -1.000000000000000000 ) ) ;
#45667 = EDGE_LOOP ( 'NONE', ( #46580, #126083, #29143, #30167 ) ) ;
#45668 = CIRCLE ( 'NONE', #22687, 0.1000000000000002554 ) ;
#45669 = VERTEX_POINT ( 'NONE', #125220 ) ;
#45670 = CONICAL_SURFACE ( 'NONE', #28947, 0.1000000000000002554, 0.003490658503988666988 ) ;
#45671 = VECTOR ( 'NONE', #92288, 1000.000000000000000 ) ;
#45672 = ORIENTED_EDGE ( 'NONE', *, *, #107088, .T. ) ;
#45673 = CARTESIAN_POINT ( 'NONE',  ( 115.5000000000000000, 2.000000000000000000, -1.999999999999997335 ) ) ;
#45674 = DIRECTION ( 'NONE',  ( 0.000000000000000000, 0.000000000000000000, 1.000000000000000000 ) ) ;
#45675 = CIRCLE ( 'NONE', #14340, 0.06509327318403745899 ) ;
#45676 = ORIENTED_EDGE ( 'NONE', *, *, #42193, .T. ) ;
#45677 = AXIS2_PLACEMENT_3D ( 'NONE', #89733, #52385, #100204 ) ;
#45678 = DIRECTION ( 'NONE',  ( -4.274815082592931898E-19, -0.9999939076577903929, -0.003490651415223739937 ) ) ;
#45679 = CARTESIAN_POINT ( 'NONE',  ( 5.599999999999933031, 12.50000000000000000, -0.4115034346978157509 ) ) ;
#45681 = EDGE_LOOP ( 'NONE', ( #18471, #34499, #110836, #48185 ) ) ;
#45680 = CARTESIAN_POINT ( 'NONE',  ( -6.700000000000019718, 2.500000000000000000, -4.330127018922201643 ) ) ;
#45682 = VECTOR ( 'NONE', #29937, 1000.000000000000000 ) ;
#45683 = CARTESIAN_POINT ( 'NONE',  ( 2.899999999999944844, 12.50000000000000000, 3.572213422710607489 ) ) ;
#45684 = ORIENTED_EDGE ( 'NONE', *, *, #103771, .F. ) ;
#45686 = EDGE_CURVE ( 'NONE', #71126, #121543, #46658, .T. ) ;
#45685 = AXIS2_PLACEMENT_3D ( 'NONE', #94918, #95566, #15034 ) ;
#45687 = ORIENTED_EDGE ( 'NONE', *, *, #83463, .F. ) ;
#45688 = ORIENTED_EDGE ( 'NONE', *, *, #122880, .T. ) ;
#45689 = EDGE_LOOP ( 'NONE', ( #64846, #32937, #126014, #3682 ) ) ;
#45690 = DIRECTION ( 'NONE',  ( -4.274815082592931898E-19, -0.9999939076577903929, -0.003490651415223739937 ) ) ;
#45691 = LINE ( 'NONE', #85600, #63392 ) ;
#45692 = DIRECTION ( 'NONE',  ( -0.000000000000000000, -1.000000000000000000, -0.000000000000000000 ) ) ;
#45693 = DIRECTION ( 'NONE',  ( 0.000000000000000000, 0.000000000000000000, 1.000000000000000000 ) ) ;
#45695 = EDGE_CURVE ( 'NONE', #42825, #100830, #49772, .T. ) ;
#45694 = CONICAL_SURFACE ( 'NONE', #118840, 0.09999999999999982514, 0.003490658503988666988 ) ;
#45696 = VERTEX_POINT ( 'NONE', #87212 ) ;
#45697 = CLOSED_SHELL ( 'NONE', ( #13402, #81027, #87574, #20135, #119079, #52618, #70677, #102908, #45355, #41736, #92946, #119725, #43817, #93994, #1145, #39834, #11725, #55347, #128233, #74708, #94779, #44024, #20923, #91414, #32715, #72470, #98697, #21239, #119253, #85296, #21021, #87421, #78474, #121682, #12361, #23436, #76050, #61423, #5226, #41316, #32854, #51017, #39234, #111017, #15280, #128914, #91353, #57416, #100543, #80350, #21494, #87228, #57251, #38924, #129025, #125121, #79388, #69408, #9372, #19561, #124949, #123772, #119581, #41629, #107194, #32909, #24803, #4575, #4454, #21670, #125774, #65047, #88832, #100132, #50822, #61351, #44275, #115779, #4078, #124150, #100679, #51475, #93905, #74154, #18659, #46911, #91092, #50258, #103043, #21120, #23557, #13835, #8615, #69781, #5917, #45905, #58887, #124388, #61077, #123885, #86635, #124226, #56030, #45612, #111028, #11863, #92516, #104228, #31965, #17820, #27953, #59471, #30500, #18945, #22166, #115242, #31738, #119746, #22100, #41731, #100168, #109307, #50321, #54862, #74616, #90158, #105647, #68626, #58731, #26850, #60530, #17326, #124066, #80762, #50917, #51789, #65196, #103147, #33277, #82672, #98762, #403, #68893, #126913, #82043, #125664, #46276, #72928, #107542, #65104, #56347, #77499, #99420, #61713, #39271, #21518, #97538, #36150, #122555, #120490, #83460, #7951, #76720, #19430, #10276, #70213, #126804, #101861, #10422, #37469, #111650, #34328, #90930, #109692, #72225, #104810, #65422, #78681, #107321, #22267, #56489, #121364, #44969, #56641, #64335, #7316, #22936, #114873, #55362, #69617, #119472, #22513, #75600, #29961, #13177, #112575, #40585, #42447, #53772, #5936, #4565, #105112, #73027, #51543, #30395, #91014, #24760, #73205, #67905, #64725, #81796, #51918, #86798, #35280, #101708, #118607, #13771, #92287, #711, #35588, #22075, #16382, #42788, #4517, #59028, #16695, #120032, #122592, #89477, #101542, #58139, #25973, #45903, #113998, #3296, #104983, #127838, #14952, #120485, #2015, #80081, #17315, #129133, #20935, #129388, #72330, #39071, #118079, #52471, #109093, #114759, #128755, #61974, #76776, #38965, #65103, #118969, #74456, #117377, #37859, #28273, #62856, #89046, #65907, #22111, #113417, #51116, #38347, #109590, #53099, #78748, #109436, #39614, #10378, #27499, #81503, #27259, #6345, #50752, #8006, #37768, #78781, #115916, #4052, #102272, #13164, #13196, #125756, #17927, #118750, #71134, #48533, #120819, #57312, #111893, #56945, #36563, #58158, #42459, #109252, #71453, #36638, #103394, #57658, #99800, #20520, #81182, #925, #5983, #94602, #71400, #91726, #7258, #24585, #9534, #7360, #91094, #15009, #109750, #12029, #76304, #115033, #20399, #57980, #120357, #84675, #30956, #69032, #6006, #25612, #77924, #119599, #4386, #85738, #79560, #106724, #74098, #112036, #70230, #57095, #57726, #21505, #33631, #113454, #59539, #92557, #13094, #65255, #63435, #37038, #44870, #90761, #114756, #58763, #19736, #37271, #47950, #63340, #28700, #6437, #109242, #7303, #56228, #28015, #106265, #101703, #1707, #125215, #73046, #46564, #88210, #126059, #73756, #86946, #11872, #127020, #84607, #22734, #128831, #105838, #64588, #25125, #109665, #66224, #53255, #125988, #11257, #25370, #62411, #34963, #82668, #88583, #100255, #97692, #108093, #32298, #96638, #82084, #97754, #75143, #11299, #101223, #27430, #18866, #68157, #107520, #112835, #1116, #39158, #83937, #52755, #87263, #20412, #93054, #89871, #12318, #97133, #31780, #41625, #62879, #98799, #36727, #12610, #73818, #125829, #83608, #2273, #121218, #15888, #85791, #3022, #20057, #58632, #89372, #109243, #27359, #43344, #38889, #98290, #112433, #90618, #1220, #115107, #44764, #90183, #102890, #55617, #117344, #25175, #90906, #66275, #29744, #1895, #86624, #4315, #107417, #4140, #20575, #15854, #96691, #33470, #45045, #123473, #49125, #9808, #110209, #7470, #102030, #45442, #35396, #87725, #72472, #28604, #25634, #56784, #66100, #88785, #83394, #93205, #117061, #90712, #84899, #108269, #119428, #73356, #69085, #48356, #48314, #85173, #103946, #107145, #98168, #33079, #82407, #102827, #46020, #55200, #73802, #86377, #81374, #66526, #19374, #45600, #55351, #90012, #89881, #56438, #114237, #31283, #72329, #128070, #75278, #21585, #6357, #93220, #15220, #55523, #6296, #117307, #33885, #114152, #87907, #81516, #76143, #25816, #111175, #41626, #80917, #44656, #107463, #125788, #72067, #21106, #9529, #9332, #59481, #39221, #115269, #87781, #93794, #82498, #100548, #99621, #24169, #9745, #29231, #23920, #91098, #72888, #12662, #95677, #53826, #30707, #16503, #47247, #48683, #54651, #125275, #86169, #8721, #112929, #114858, #38858, #43433, #103051, #13924, #72167, #22830, #118444, #54458, #83565, #122351, #99822, #21612, #23734, #1807, #68562, #37570, #51777, #79694, #107354, #15434, #32657, #62719, #33074, #32449, #61991, #85485, #62149, #64377, #68633, #129394, #108579, #35835, #13456, #66510, #8883, #99575, #122301, #80610, #45129, #68097, #12602, #36991, #112972, #47164, #32408, #5678, #125218, #22210, #14071, #87676, #111065, #17379, #100246, #60421, #42620, #63173, #122835, #121645, #121070, #86689, #102440, #21027, #54163, #100295, #119518, #116030, #6647, #76756, #24718, #27136, #45008, #18323, #120089, #17388, #77655, #70049, #47632, #52826, #87685, #101597, #84890, #7669, #72231, #12374, #124230, #51391, #11581, #24586, #63120, #19937, #108509, #6532, #69088, #112376, #54041, #61361, #107383, #127525, #75864, #82717, #98764, #35677, #73654, #98573, #128808, #58170, #62232, #68059, #60345, #22242, #104237, #117630, #106566, #37066, #87084, #15771, #15997, #106252, #23860, #92136, #102712, #10985, #99088, #69736, #113554, #88221, #106880, #77090, #104281, #12923, #98194, #105487, #35110, #29804, #42998, #10864, #29323, #40260, #25163, #114086, #20813, #78077, #25650, #106563, #33889, #79303, #113979, #125811, #107565, #1643, #124781, #9393, #84542, #101756, #24280, #61399, #58058, #103856, #43695, #73878, #119698, #121856, #56179, #68265, #95981, #51971, #25729, #113255, #121619, #85069, #114977, #7418, #25287, #23982, #72465, #33331, #3745, #73363, #37578, #118821, #84911, #71622, #109257, #74107, #31216, #123116, #33776, #75197, #62758, #74843, #59526, #28763, #7160, #128489, #47977, #14645, #113252, #76770, #52212, #30728, #33013, #54380, #113895, #46109, #91251, #32005, #127175, #105077, #115476, #10521, #23971, #63530, #20296, #37625, #17335, #97861, #60008, #119138, #62135, #129387, #87193, #4299, #37220, #54593, #60501, #69824, #36419, #52570, #60196, #66568, #49130, #53935, #50310, #14708, #79574, #70012, #108577, #92251, #129120, #93926, #121978, #23269, #76821, #22237, #14085, #53266, #127894, #97020, #92588, #86301, #8424, #101769, #107190, #108611, #32932, #118981, #117621, #47543, #108626, #59700, #83997, #30233, #31388, #43236, #14800, #4963, #18032, #121776, #103859, #54047, #103672, #75546, #61249, #3485, #40870, #59373, #12930, #91975, #43417, #77343, #119734, #23818, #6826, #100084, #81495, #80882, #106055, #47080, #124489, #32463, #62874, #109305, #83945, #116017, #18611, #77341, #48120, #84604, #37158, #102575, #57898, #114535, #34569, #23321, #116016, #67735, #21340, #81085, #57987, #62558, #33596, #42928, #28333, #124224, #19887, #15177, #85045, #40741, #110573, #119129, #56180, #36831, #14791, #11673, #120183, #125841, #17216, #70272, #37588, #7750, #7462, #930, #48051, #66196, #10826, #36532, #6943, #82683, #45865, #108425, #1938, #33383, #14006, #50156, #125116, #34796, #98685, #79305, #100858, #33327, #11867, #22847, #55013, #16319, #71289, #127060, #71098, #116755, #24905, #42613, #83469, #87976, #47794, #6538, #85875, #67173, #86036, #128335, #21502, #45595, #35417, #8459, #126599, #21175, #100550, #95467, #34977, #125536, #99673, #49292, #115924, #5572, #116448, #7321, #127375, #81958, #36585, #641, #43728, #83979, #24443, #94197, #97396, #121691, #45703, #50575, #77743, #29318, #104070, #65019, #15873, #92151, #94643, #74261, #1432, #60209, #69345, #84794, #73338, #11748, #29977, #48059, #61813, #82666, #24912, #103014, #2736, #3651, #39100, #77911, #75039, #123373, #101133, #33287, #78422, #117957, #70862, #16448, #107618, #2866, #105698, #100148, #114790, #52830, #75151, #85928, #32610, #22595, #65938, #759, #81334, #2536, #82657, #3140, #43674, #92340, #12022, #46072, #49595, #50043, #87966, #112675, #68039, #108051, #40926, #104926, #128680, #124384, #10222, #23552, #11475, #56959, #20705, #86044, #126860, #6093, #69458, #107743, #45285, #47658, #75428, #102867, #17257, #111136, #85048, #89931, #91834, #37113, #51486, #56738, #29966, #38698, #107962, #56337, #43837, #125610, #102487, #24493, #121681, #112191, #17224, #36823, #60206, #103389, #36600, #114724, #15693, #122021, #7310, #75543, #124604, #478, #2573, #41050, #80472, #9795, #41482, #26072, #86676, #50369, #46659, #61392, #34389, #64437, #28911, #109747, #65192, #59368, #111222, #66529, #92031, #23817, #60806, #124665, #121461, #21676, #56320, #51947, #24292, #112820, #34071, #19877, #101813, #102851, #12138, #63760, #7792, #49190, #34054, #101702, #44120, #72883, #14710, #109824, #86475, #48702, #15449, #33473, #22561, #37612, #27684, #92238, #99918, #75140, #124555, #97931, #27118, #114437, #71444, #127584, #42072, #39551, #78823, #110018, #115492, #87096, #124945, #86998, #114908, #108682, #105909, #74273, #103385, #14949, #27523, #25333, #4013, #100535, #129373, #41723, #28685, #24958, #109365, #63442, #94592, #84256, #108480, #7531, #48964, #125780, #31086, #39588, #118688, #103794, #78584, #115144, #92675, #74424, #6663, #15388, #123002, #53994, #88012, #4783, #65190, #77539, #68307, #60452, #100841, #32393, #54004, #21959, #69512, #89791, #109140, #33590, #49346, #127626, #82235, #108927, #97231, #128275, #116583, #4208, #94943, #6640, #30051, #34640, #4215, #105029, #103289, #35525, #67685, #80766, #70122, #118869, #120178, #52268, #67004, #42091, #98429, #100705, #95254, #62163, #25554, #108986, #33772, #11730, #46931, #91672, #93565, #26218, #92712, #30669, #126429, #8785, #13311, #104224, #176, #24439, #118330, #89797, #34469, #56424, #57392, #34537, #41882, #105285, #59951, #107951, #48966, #113519, #109150, #37776, #111501, #123315, #44500, #33228, #69796, #62630, #106489, #14855, #27209, #16105, #47808, #17488, #18639, #91513, #115097, #123587, #107044, #54405, #74713, #10012, #93412, #105338, #33824, #60262, #81414, #37317, #22090, #30744, #63022, #2133, #81698, #10105, #16020, #71585, #80570, #71747, #89993, #90683, #125984, #96965, #46360, #60913, #82225, #66832, #110153, #103954, #105365, #29352, #89647, #46299, #4068, #88236, #70261, #58716, #125360, #57682, #82053, #52362, #48214, #5422, #70829, #1496, #107096, #80179, #123423, #104935, #127734, #116385, #94289, #17748, #119179, #114213, #121110, #72010, #127726, #2175, #35206, #23091, #100849, #103612, #64460, #115601, #97192, #17601, #102962, #101601, #1391, #42684, #16839, #87041, #93302, #129127, #20037, #66284, #120130, #53474, #63769, #91924, #27165, #66017, #54981, #99609, #66982, #10569, #77812, #90175, #32299, #21824, #70680, #15880, #104546, #64165, #24440, #11147, #101580, #95506, #118176, #40296, #33182, #21826, #71495, #47056, #38486, #37154, #97011, #117677, #103643, #54467, #89221, #89149, #106857, #60110, #81896, #13593, #79796, #42516, #96549, #76580, #33004, #26692, #36331, #69852, #56256, #9526, #23264, #114693, #78692, #12181, #10107, #75189, #103962, #72314, #75985, #94869, #54451, #2137, #6249, #30651, #27469, #71162, #93105, #63909, #102753, #53566, #11550, #94930, #33673, #72230, #16675, #39592, #338, #47375, #49277, #93042, #111444, #33634, #68804, #76918, #66372, #43066, #84913, #34797, #89322, #5327, #3268, #102637, #108673, #55296, #123479, #29343, #87047, #91690, #92313, #100833, #61828, #73486, #38692, #61294, #37871, #3613, #2280, #49279, #122966, #88733, #283, #106577, #127031, #58422, #94323, #62998, #9365, #12510, #95737, #91518, #37584, #85734, #13355, #27213, #59260, #128258, #80605, #111560, #57420, #108516, #81544, #112455, #31275, #109847, #116395, #83990, #18926, #29015, #64740, #101259, #98929, #15910, #52119, #112416, #29969, #105091, #14944, #48786, #107938, #51247, #62566, #61877, #35692, #6654, #75982, #80776, #79869, #110461, #114291, #15065, #4203, #44115, #41054, #65046, #8481, #22191, #118298, #47325, #76407, #64901, #10511, #104589, #116411, #93452, #115468, #6565, #35170, #31074, #55574, #33578, #2672, #103805, #77203, #31679, #128238, #77049, #86517, #78841, #22086, #65962, #113879, #5213, #73253, #5729, #32760, #41099, #113410, #39555, #85634, #113892, #113082, #81894, #57513, #74970, #78255, #112218, #36735, #114700, #21852, #103396, #45080, #91111, #88882, #96585, #54355, #122125, #120217, #44693, #87991, #30829, #20132, #88287, #119763, #32923, #128164, #94599, #30825, #85216, #38356, #3525, #64203, #43182, #74069, #50408, #27580, #26974, #111900, #69565, #60661, #7572, #64500, #76283, #113125, #29421, #117353, #1543, #37920, #49870, #119712, #62969, #3335, #48540, #59086, #56242, #36270, #118117, #25076, #108912, #106822, #5267, #120804, #1234, #14704, #118065, #49714, #39889, #57404, #23282, #27845, #18663, #126168, #11985, #110554, #51200, #61728, #28163, #1855, #52104, #18065, #5512, #65371, #95667, #40428, #17981, #90731, #68790, #46738, #90774, #37861, #118020, #484, #67724, #121966, #87208, #40906, #80009, #11820, #2689, #114289, #22682, #63613, #118141, #121780, #29902, #15168, #110454, #85638, #85459, #30998, #42021, #82195, #108277, #12178, #67897, #116600, #119033, #69150, #120904, #100894, #11777, #42457, #106571, #74943, #53894, #10169, #49955, #100292, #65587, #57900, #11254, #23679, #110834, #17627, #10700, #6348, #59810, #46075, #94436, #101126, #4903, #60671, #6832, #127170, #122191, #99470, #119928, #117192, #74975, #79232, #6870, #102348, #41039, #72728, #35405, #84159, #91677, #46032, #18570, #22103, #98581, #89591, #94835, #89557, #31597, #62619, #126856, #93354, #110570, #100129, #76455, #44537, #78849, #90494, #56185, #94294, #71726, #75919, #118842, #4201, #98316, #123910, #109845, #63969, #93398, #114655, #17819, #44967, #103533, #38649, #7464, #38183, #61397, #87819, #47404, #106474, #32562, #39996, #125037, #56958, #115029, #109095, #30798, #38978, #123121, #62404, #12198, #88323, #120238, #74113, #27408, #110293, #34046, #70516, #9322, #84092, #62913, #3031, #96432, #73932, #123645, #19109, #129068, #42889, #78415, #6110, #113561, #8450, #7195, #119016, #58561, #47757, #75713, #27388, #73048, #30130, #125835, #86247, #79312, #53851, #65194, #129546, #48275, #80885, #87, #44918, #120344, #70994, #35354, #127791, #81234, #111455, #82990, #19612, #17283, #62302, #124011, #18981, #96676, #70598, #77183, #125376, #93864, #121015, #128487, #63277, #108822, #31688, #101441, #81588, #72935, #26210, #99507, #17036, #22034, #54009, #81637, #65527, #70671, #51841, #117786, #51567, #56582, #113237, #71581, #54595, #77449, #110471, #49987, #78353, #23600, #97037, #9175, #87341, #9234, #62394, #120707, #27015, #124547, #7155, #15290, #102891, #111459, #112685, #30987, #122594, #99027, #90288, #11143, #31129, #125715, #125624, #7135, #91576, #70724, #41153, #44388, #127286, #17, #1076, #111004, #51959, #94691, #54214, #95259, #74658, #42735, #29236, #66819, #23374, #18070, #108378, #29480, #16736, #71920, #96550, #47797, #33569, #15708, #102185, #66589, #88072, #114923, #27354, #61131, #80733, #20607, #60432, #57224, #7481, #128212, #70726, #84433, #59809, #128614, #126695, #57118, #113614, #68462, #48370, #67266, #84998, #39493, #115117, #110474, #32538, #124054, #118030, #51384, #52338, #94354, #93287, #69364, #106020, #68474, #95978, #22718, #23364, #29578, #43792, #40824, #7483, #86692, #98165, #24907, #85076, #63780, #28746, #59883, #51494, #1581, #61661, #76134, #73047, #74334, #665, #21297, #110313, #318, #8931, #72779, #114592, #29652, #95512, #115208, #78248, #34369, #57073, #118720, #53952, #13012, #60535, #102340, #108265, #10430, #75711, #53897, #3131, #92395, #52685, #35426, #97784, #97138, #56348, #124014, #88219, #89165, #26228, #34886, #84499, #58455, #72784, #35783, #55748, #32277, #10231, #79922, #25971, #116762, #93316, #51554, #95458, #37205, #30068, #45311, #91240, #28651, #34212, #60095, #63959, #129221, #97964, #58143, #30345, #78565, #61778, #28001, #119685, #10804, #18819, #106069, #77402, #9193, #33881, #121128, #34532, #31386, #128337, #31847, #93121, #98072, #89778, #72680, #6408, #119532, #23539, #29326, #127412, #5695, #70763, #57666, #43251, #88848, #24328, #75455, #11228, #75248, #40730, #4563, #107026, #99686, #73339, #18826, #116328, #72160, #66999, #11556, #26942, #65679, #24028, #27866, #27572, #70102, #123432, #44215, #108125, #58309, #26323, #28123, #7731, #90677, #89614, #71301, #19835, #37436, #45651, #1874, #67879, #30552, #43566, #71439, #120674, #108810, #47700, #49184, #42792, #32705, #116913, #90603, #104065, #123067, #93626, #28546, #5115, #17325, #44130, #61742, #125459, #60818, #50909, #81171, #125131, #102911, #119277, #20307, #35106, #36090, #92237, #47958, #2105, #89879, #106221, #22107, #94058, #107183, #39542, #68392, #69189, #81505, #83690, #110152, #125364, #93425, #7988, #80399, #43055, #88377, #94827, #105850, #57734, #114443, #25735, #1252, #80974, #7890, #121394, #99964, #16291, #85783, #40040, #17312, #72367, #19723, #78956, #21484, #78149, #59044, #78739, #49044, #29919, #128823, #63433, #52814, #18136, #66110, #85726, #41412, #123679, #71525, #18563, #12779, #4304, #77856, #112787, #88234, #4614, #47641, #81744, #58301, #80281, #119123, #25581, #99294, #23433, #82952, #56505, #101648, #111779, #63599, #27512, #26394, #91536, #116693, #64371, #10714, #34535, #18350, #101296, #82058, #83233, #87359, #66122, #30080, #55051, #11472, #108985, #23534, #112524, #5473, #97649, #111268, #8930, #58931, #7421, #49422, #9539, #110611, #71051, #106473, #53839, #27696, #59053, #112488, #62456, #94332, #74249, #29608, #28345, #77635, #66664, #15540, #12693, #82574, #103240, #65134, #56506, #128511, #69508, #36166, #7397, #51483, #38191, #14198, #86866, #90441, #17245, #43605, #79043, #105589, #109136, #62723, #61237, #7156, #84272, #122702, #80478, #121953, #68608, #51397, #58211, #21063, #33014, #122689, #77189, #120286, #18354, #29914, #118270, #89407, #38529, #69344, #79321, #83701, #112098, #75869, #3907, #89925, #42096, #76147, #111992, #94587, #83703, #69205, #28769, #76197, #102646, #85156, #9832, #17810, #50118, #127630, #70412, #67754, #28447, #2112, #38375, #89294, #108361, #113363, #4465, #36882, #84690, #69102, #31224, #58161, #35013, #65619, #106369, #17063, #42134, #72281, #92283, #50571, #97244, #28844, #2791, #26392, #60777, #25214, #125052, #94600, #60482, #107884, #46035, #54548, #57453, #106162, #47653, #34935, #22776, #105099, #21074, #20380, #83294, #376, #124291, #108249, #75538, #110714, #93309, #82408, #17680, #7152, #13085, #3614, #67289, #122296, #50225, #61574, #111517, #104667, #41492, #104119, #60768, #45028, #69526, #42844, #2880, #128042, #87680, #3776, #127104, #73552, #26799, #9614, #49699, #112629, #96523, #71239, #35420, #103347, #33000, #10099, #92460, #48075, #10271, #4145, #65224, #64988, #115760, #27244, #6154, #80622, #89281, #8474, #107040, #127336, #69673, #88070, #75396, #47550, #53726, #101663, #53149, #106686, #38045, #101147, #84412, #109789, #28927, #46631, #122543, #2372, #104517, #66746, #42288, #126540, #84849, #63901, #122714, #110770, #3992, #8027, #14503, #126996, #32614, #100451, #36000, #108470, #7707, #91856, #83798, #114384, #123724, #52667, #43834, #77462, #108040, #2115, #63667, #99571, #26537, #50631, #62466, #70462, #113230, #29950, #98628, #93001, #6823, #9952, #51641, #45146, #104046, #112100, #7654, #78985, #89630, #1397, #76208, #33126, #126476, #37146, #6108, #9158, #80454, #71141, #98639, #106995, #5506, #102036, #42668, #128235, #129552, #11131, #94753, #101750, #73343, #18407, #73649, #67006, #117443, #74357, #50739, #754, #75243, #1711, #8323, #41369, #6931, #68843, #82344, #30967, #129132, #60375, #109433, #63508, #66431, #86899, #17439, #1063, #128500, #74663, #96067, #45346, #37322, #42469, #69357, #47556, #28159, #28571, #76664, #117113, #96208, #84645, #69958, #50737, #30397, #78675, #82959, #104522, #77094, #69808, #35424, #93549, #95237, #51399, #6725, #17206, #16018, #14643, #47483, #49602, #40855, #116956, #6239, #14755, #60360, #91735, #21559, #106807, #53264, #36695, #8567, #61220, #32915, #98587, #25733, #44216, #41359, #86800, #53718, #42674, #79917, #74257, #51342, #57014, #102500, #28750, #101302, #3591, #99097, #51642, #31633, #124743, #51378, #119910, #110450, #88527, #19901, #83138, #82393, #23429, #76712, #128344, #122482, #31704, #72623, #112192, #116329, #62869, #95421, #78663, #3705, #95576, #43646, #127430, #38971, #123874, #21880, #15436, #77493, #31438, #37516, #64644, #94032, #122679, #93238, #81801, #108208, #105741, #113103, #47786, #122017, #5939, #56517, #31834, #60611, #56244, #26801, #22154, #50467, #87983, #114707, #43356, #26793, #60963, #107301, #114293, #4154, #52265, #124155, #12402, #69349, #79255, #10372, #24496, #74761, #14394, #56975, #110881, #112532, #32014, #86050, #49854, #30924, #35129, #125654, #85569, #127135, #43553, #99796, #63664, #96808, #8831, #16440, #71019, #83830, #657, #39842, #29194, #85103, #42528, #117806, #34691, #127426, #69971, #42520, #128154, #5166, #85587, #77120, #108620, #12764, #77799, #114914, #18714, #53167, #43663, #36271, #21675, #106053, #84694, #10969, #35520, #88601, #111793, #100398, #20292, #52374, #97350, #113893, #9687, #63905, #91034, #113234, #35793, #70992, #104887, #56694, #473, #14327, #46629, #105007, #64531, #86464, #91520, #82516, #9028, #30862, #108520, #25064, #123732, #13606, #68529, #78068, #64777, #44961, #6233, #126958, #59848, #127180, #84311, #99812, #108730, #40843, #22988, #97286, #118926, #71788, #118227, #34049, #2825, #28450, #18000, #83698, #78060, #100936, #6163, #85944, #26700, #91987, #82405, #32903, #28282, #108836, #67144, #106615, #40900, #35972, #34216, #87399, #125228, #56018, #39062, #84268, #31952, #92301, #100020, #118852, #380, #91787, #15206, #31829, #22716, #110410, #81363, #54205, #124391, #87356, #86778, #51800, #37155, #114578, #52272, #40090, #41727, #60157, #27674, #49755, #68312, #45225, #64957, #56909, #28712, #20714, #44701, #47172, #22882, #78626, #53722, #59819, #22932, #81096, #117060, #76765, #99009, #91990, #28798, #31209, #104272, #25868, #95266, #48126, #3769, #112674, #10071, #20343, #116313, #8, #46322, #63226, #107360, #40230, #73332, #21768, #14940, #86673, #120496, #55630, #44474, #12149, #2992, #63516, #61092, #124638, #8210, #90666, #53095, #83151, #61826, #79682, #83549, #56183, #27965, #18863, #61992, #128926, #108795, #88415, #108676, #116486, #7518, #13175, #13252, #120657, #69, #106471, #37932, #89456, #97215, #104374, #13501, #71755, #56245, #81015, #29585, #74510, #111329, #33054, #96221, #73916, #92471, #3730, #90936, #43560, #107483, #69776, #82722, #105855, #46754, #37770, #30904, #10931, #81492, #20466, #66736, #127577, #15420, #32911, #9319, #120298, #70219, #123979, #106715, #18285, #27996, #103977, #95819, #18247, #1438, #61930, #72936, #5847, #96743, #124488, #77032, #29097, #54455, #26382, #42954, #82329, #71894, #10672, #39288, #89899, #10461, #60517, #128971, #88409, #76483, #12747, #28919, #16760, #58681, #6662, #100840, #42439, #102132, #26899, #38973, #108375, #59651, #21814, #70513, #62345, #113400, #81238, #81092, #11999, #62548, #68453, #34945, #82340, #83757, #104114, #17703, #20606, #108962, #18967, #11891, #89422, #4722, #8407, #55199, #6100, #93796, #121112, #62773, #41525, #53098, #29564, #43358, #40245, #97916, #35019, #100396, #125383, #94036, #68309, #42503, #10555, #30031, #2886, #29495, #40298, #53684, #18399, #10924, #129512, #75604, #71127, #99256, #98427, #81811, #26340, #117035, #37465, #96993, #9698, #87250, #49266, #69849, #60964, #29538, #117858, #66374, #104105, #9949, #75392, #122459, #41430, #105084, #80825, #6091, #3597, #87582, #13759, #15233, #84173, #40597, #86016, #47065, #52407, #90332, #38364, #56193, #36575, #59961, #73104, #14075, #74162, #106708, #32340, #32628, #8776, #8773, #37032, #40671, #93027, #93732, #76040, #128771, #59527, #89924, #27159, #24172, #92409, #102021, #61081, #82913, #91189, #43685, #116952, #99991, #33338, #76719, #109203, #92913, #81582, #120401, #67500, #47489, #104672, #89889, #33466, #94986, #57918, #116346, #124107, #1077, #66088, #103379, #122917, #43991, #34706, #3339, #104436, #100769, #89376, #87458, #38956, #74668, #87670, #114713, #41458, #1067, #97294, #77082, #73829, #50419, #44650, #21345, #23116, #46652, #27492, #15870, #19574, #97592, #46465, #40986, #69629, #113457, #100619, #111471, #68577, #115312, #43658, #21067, #50187, #115010, #127219, #8758, #34637, #55716, #38795, #83958, #17821, #6991, #64078, #102119, #89037, #25021, #25362, #49702, #121791, #78004, #111166, #41110, #28010, #80575, #121396, #9866, #79861, #42910, #123282, #24014, #6644, #39708, #10751, #105753, #83661, #64488, #33087, #127354, #111030, #127572, #96220, #18240, #119753, #51030, #36741, #94396, #107203, #82288, #45768, #120017, #49132, #15866, #36579, #5220, #26662, #89139, #2740, #92662, #113250, #112986, #86937, #69833, #67272, #100785, #16431, #49215, #114132, #27357, #91085, #104206, #116476, #77244, #45899, #98748, #41831, #51410, #72488, #43923, #28484, #36421, #24605, #72173, #34276, #118421, #51069, #31378, #9106, #52112, #11242, #120077, #19416, #80722, #29801, #16799, #120073, #36794, #98906, #3039, #91209, #105269, #86921, #80182, #101236, #126448, #72872, #49710, #15430, #127466, #66846, #22993, #93056, #55674, #123338, #34755, #84536, #79236, #94047, #87102, #89214, #26958, #8879, #113982, #66889, #117102, #24137, #4831, #5779, #31971, #124168, #47640, #118759, #105097, #81281, #17049, #120236, #46153, #121231, #115008, #106641, #126594, #92843, #34645, #125390, #50188, #41306, #97298, #126115, #46121, #114670, #38384, #84824, #35944, #129297, #15687, #32120, #38102, #80073, #22659, #14257, #10737, #60353, #13339, #126762, #56294, #96967, #1644, #105481, #53975, #54980, #45760, #102017, #24342, #788, #74840, #22427, #107260, #32697, #116649, #43420, #18551, #90330, #79094, #121248, #124049, #6064, #53833, #60378, #59295, #61860, #69103, #76297, #35265, #68959, #21007, #96286, #60635, #81600, #47815, #66268, #52485, #95984, #62612, #122143, #83034, #111387, #72340, #125937, #80615, #103655, #66775, #39985, #128393, #24454, #27509, #101442, #73341, #1851, #1960, #89043, #42948, #4729, #31698, #97610, #63011, #27864, #81793, #57571, #93621, #119701, #119809, #8157, #30827, #29438, #66697, #19740, #11000, #33782, #126998, #70503, #111280, #77972, #21982, #74827, #107689, #35247, #79416, #14235, #85340, #59150, #38544, #90506, #46269, #593, #69679, #108206, #81017, #116331, #33639, #80774, #312, #55374, #57244, #123024, #82808, #7848, #7574, #125042, #71380, #121738, #18446, #67937, #80296, #70750, #26881, #21321, #65510, #110726, #78426, #64527, #51585, #125375, #9537, #13654, #88666, #57126, #32003, #114135, #90024, #113722, #52257, #111371, #1135, #126032, #18090, #12035, #43256, #91729, #52261, #66989, #106145, #94178, #55157, #19734, #87722, #3446, #120583, #68218, #47469, #109316, #48700, #22983, #64950, #41571, #42628, #103338, #112547, #93157, #69041, #57652, #105044, #94336, #84993, #15113, #111231, #109909, #54322, #108757, #49142, #33225, #109407, #106166, #51951, #106588, #75447, #117626, #60324, #74828, #125331, #101298, #125508, #100798, #99417, #87669, #115720, #35359, #92900, #74307, #37641, #53665, #10042, #38527, #18662, #49289, #41490, #25206, #49129, #116499, #22974, #20716, #69683, #71961, #93207, #7835, #81910, #37307, #22397, #17333, #14557, #66787, #68470, #78357, #120193, #102335, #119270, #88721, #12050, #74309, #24131, #1859, #1343, #88694, #116964, #123266, #44305, #48081, #27401, #31375, #77309, #82167, #105293, #10956, #28320, #74551, #104582, #74573, #33239, #38094, #2531, #105264, #68722, #27121, #108193, #79353, #14056, #89828, #106637, #70270, #23554, #106736, #76605, #47645, #81510, #50799, #14653, #12518, #113379, #44825, #78999, #41397, #32866, #90432, #122619, #91419, #89739, #86030, #128677, #102077, #11736, #85003, #55465, #105853, #22956, #71409, #73308, #8217, #62807, #33340, #74564, #65020, #129381, #85219, #120232, #42344, #97341, #117471, #35545, #53274, #88078, #24020, #32294, #91940, #89329, #40746, #45532, #73130, #13299, #58715, #101854, #118923, #27961, #7153, #66627, #21765, #5627, #49655, #29082, #86783, #97435, #28335, #95826, #56063, #25306, #2008, #99249, #47954, #75717, #83116, #123181, #19746, #99133, #40505, #121685, #129201, #26181, #103159, #30701, #118340, #88213, #27664, #119861, #107786, #51815, #39938, #54855, #53916, #392, #77194, #1974, #66971, #14491, #21511, #96227, #11781, #6492, #4451, #6000, #100792, #70813, #20179, #119595, #17814, #33231, #108965, #60361, #94185, #21840, #23717, #19283, #10417, #104074, #67825, #31039, #85683, #93876, #25822, #114195, #81731, #24230, #14559, #30954, #11413, #106179, #42334, #31846, #125679, #127013, #128569, #23110, #107481, #56349, #10005, #68051, #82937, #79244, #13073, #37056, #3172, #40310, #91587, #27267, #63024, #75300, #119199, #105161, #94929, #88402, #22794, #16848, #71801, #4460, #88570, #11994, #126530, #115158, #36940, #12439, #81047, #77647, #85158, #82289, #27066, #24338, #47390, #109235, #125562, #10008, #114588, #53984, #107745, #114400, #120977, #65357, #88589, #28913, #120242, #125230, #12130, #27737, #9054, #10057, #45131, #3925, #120644, #25628, #68185, #31522, #127747, #112091, #112772, #25172, #126537, #84705, #113508, #89527, #87668, #62601, #115470, #86785, #6258, #48796, #124003, #86720, #43665, #8461, #119642, #102651, #81318, #27257, #61136, #54165, #56911, #122872, #109378, #109583, #2579, #8767, #85476, #117905, #38634, #57886, #81574, #21188, #52256, #36788, #46772, #61816, #91685, #104017, #25795, #94491, #49273, #19114, #129233, #120090, #31511, #74260, #44561, #26647, #15802, #124801, #90451, #116637, #77581, #81250, #121363, #112360, #92719, #116177, #62711, #97872, #62675, #13241, #102617, #97761, #20293, #104468, #62614, #127121, #29285, #11162, #104126, #124235, #90988, #55164, #33715, #105393, #22253, #27789, #106109, #96869, #67453, #56550, #124695, #87195, #102490, #113090, #53200, #29903, #117536, #101760, #75640, #34717, #78731, #102382, #4153, #97556, #100530, #79705, #33903, #57989, #5604, #40480, #56247, #125663, #74849, #59018, #116656, #127174, #21926, #129484, #90028, #43963, #58884, #23486, #92727, #55632, #71748, #58625, #4110, #11751, #88994, #17879, #108340, #105426, #85789, #127428, #3898, #82817, #94484, #126588, #99665, #20463, #126077, #81089, #122389, #62429, #19377, #31998, #9678, #44850, #95364, #107686, #21348, #72474, #122131, #115319, #54154, #59693, #92893, #123407, #83541, #58719, #129234, #55207, #101922, #26960, #29181, #61552, #75233, #45770, #86213, #81944, #44255, #103278, #104832, #83397, #85965, #70988, #17381, #129066, #52501, #5038, #28864, #25811, #104678, #70263, #95350, #115058, #114722, #108146, #119341, #123270, #107644, #6213, #73457, #54762, #107798, #6205, #102004, #53178, #53574, #84451, #24275, #55564, #47078, #24692, #78836, #61619, #70846, #15120, #11086, #27625, #121839, #76566, #37168, #17111, #20623, #80036, #11571, #69674, #48863, #84155, #75386, #99032, #44461, #122156, #227, #55214, #76629, #96491, #122995, #101118, #114136, #47395, #33614, #54159, #117117, #43530, #67740, #45811, #41711, #38622, #125619, #90038, #13244, #62192, #88337, #41207, #65524, #120065, #59312, #116855, #120985, #107317, #2683, #123176, #37477, #65365, #4472, #83717, #87094, #99556, #123571, #48254, #81938, #68007, #99356, #89008, #12634, #49393, #108316, #55024, #107839, #115165, #54136, #53413, #127259, #43740, #56339, #85935, #72000, #10808, #44752, #88233, #28067, #79964, #24757, #69640, #18728, #41644, #77486, #85882, #48544, #86520, #76703, #17055, #71731, #39854, #74203, #59388, #63816, #117503, #26400, #127028, #53332, #87867, #11529, #48202, #117846, #63101, #51908, #32061, #9046, #5522, #85149, #14942, #35821, #21958, #3752, #80937, #35534, #12859, #125214, #105677, #1363, #91602, #68046, #15823, #28382, #101183, #29617, #124746, #65215, #95525, #104540, #48071, #15549, #112988, #70422, #94208, #115328, #53716, #55453, #75823, #37324, #117944, #79455, #19560, #97998, #33865, #49140, #31799, #56657, #52216, #57835, #124347, #118603, #81623, #92731, #106622, #75718, #80865, #100503, #68488, #128819, #41986, #14938, #27734, #33638, #112365, #39119, #73215, #105737, #20854, #36733, #62096, #4220, #52821, #23268, #91429, #55923, #63159, #35724, #45286, #56907, #126450, #2751, #609, #79459, #67946, #80498, #55610, #113829, #117351, #104720, #16110, #43583, #42946, #44704, #39536, #8256, #49443, #42795, #30813, #84145, #49544, #42873, #59485, #5155, #83929, #9035, #58633, #125385, #53593, #17153, #126092, #213, #84600, #36843, #11154, #124216, #56003, #435, #70377, #4730, #118487, #79770, #80444, #58718, #34214, #57880, #43667, #43969, #4445, #41300, #73667, #36093, #121857, #26851, #46367, #41937, #105889, #97018, #17765, #96263, #61254, #64020, #19625, #111951, #75, #15564, #93556, #38416, #126828, #22828, #82009, #98760, #2218, #23411, #115157, #13806, #76364, #118705, #96089, #43188, #127827, #10176, #103706, #60678, #47026, #24399, #114458, #127321, #113144, #77907, #75252, #18956, #30196, #72108, #10652, #39701, #21490, #43405, #129404, #85374, #67384, #31369, #122142, #30186, #98912, #128816, #108301, #48877, #70166, #90686, #3082, #105905, #118133, #34379, #68045, #120768, #73212, #125931, #125618, #106318, #73837, #25177, #81591, #69058, #19121, #8311, #15644, #21083, #120494, #98462, #44214, #109848, #6660, #90682, #58783, #16728, #83983, #114377, #7143, #31278, #96510, #6697, #17657, #87812, #17342, #45952, #75800, #81878, #77782, #127419, #79195, #38881, #42188, #34696, #74513, #9791, #96132, #34792, #91398, #63444, #18814, #1959, #50481, #15451, #18185, #129248, #120639, #105435, #92737, #30097, #74106, #19061, #25429, #59082, #82022, #126268, #35608, #14396, #127315, #45584, #8302, #23217, #94449, #65891, #39417, #57262, #85466, #104267, #20824, #107781, #14244, #97594, #129412, #72953, #56402, #87790, #96623, #1790, #96794, #61972, #78311, #75290, #50896, #74723, #12612, #23450, #93736, #50716, #89721, #66165, #6813, #105147, #54923, #54146, #16491, #107491, #83386, #117, #94389, #106572, #107647, #59689, #103229, #36992, #122297, #93892, #77866, #1721, #41260, #59653, #92303, #92135, #63705, #30699, #94487, #67074, #1241, #36577, #117229, #63131, #6243, #27667, #113573, #7570, #34868, #64049, #74572, #116169, #38461, #31619, #80929, #108494, #10562, #36486, #18084, #35372, #71437, #55787, #108979, #84947, #112511, #40087, #3288, #12309, #1388, #95563, #88752, #119422, #15667, #26703, #15374, #27018, #102733, #28544, #35879, #13660, #79550, #52042, #59582, #89065, #44818, #127227, #123716, #1404, #57123, #71711, #102952, #55408, #54103, #79701, #103895, #30246, #97706, #119438, #68833, #39110, #33343, #59817, #59614, #46901, #95247, #103793, #116217, #66732, #38669, #117691, #32188, #126742, #29027, #12771, #120597, #79822, #68943, #75094, #104665, #106408, #26856, #5854, #15231, #102894, #90513, #58869, #57946, #96377, #122457, #8160, #71571, #118719, #114440, #125606, #97450, #36072, #42615, #61138, #71002, #113832, #62417, #81917, #128396, #63169, #122602, #115608, #88471, #39703, #29338, #90444, #37677, #129447, #16589, #73937, #102748, #19062, #16836, #52361, #90777, #30324, #55356, #122095, #90203, #65039, #93632, #115491, #65777, #113967, #107467, #94182, #115161, #77628, #7875, #107836, #81266, #122445, #90526, #121961, #125164, #94201, #24070, #34240, #123849, #65113, #22504, #34378, #84319, #17611, #28453, #17487, #2408, #113551, #22972, #57669, #117267, #95529, #105263, #6094, #128610, #113725, #101924, #85114, #68937, #21827, #51484, #123727, #10947, #49193, #70371, #126871, #120505, #84056, #116233, #52531, #51061, #31136, #57064, #98014, #4881, #7903, #7408, #89169, #68323, #87087, #14720, #33763, #63585, #37001, #107244, #120240, #54611, #106625, #101065, #102628, #40543, #93718, #3912, #61236, #56630, #126357, #124906, #59781, #21289, #22159, #75399, #120699, #21844, #114349, #73465, #92241, #78200, #965, #118915, #54620, #22416, #10710, #121519, #28261, #30383, #49434, #31961, #1194, #51066, #30814, #99523, #46750, #8719, #15726, #48845, #126848, #68792, #95687, #93786, #127656, #22567, #45864, #33988, #85478, #83281, #88303, #78677, #9644, #79608, #66958, #32929, #59143, #62919, #43843, #73203, #90084, #15262, #64423, #62563, #110921, #23438, #63661, #115105, #96859, #67580, #25270, #14956, #82652, #122443, #52529, #109934, #64570, #110885, #107221, #39444, #17506, #46841, #85833, #122397, #14476, #112104, #61568, #20458, #9850, #79951, #6104, #89309, #127877, #87147, #6817, #71389, #106719, #7423, #918, #23275, #45451, #89010, #34371, #112888, #66254, #78418, #23595, #102797, #129347, #44224, #112990, #70591, #33731, #99512, #20727, #94012, #102919, #114921, #69338, #107305, #38168, #18705, #107928 ) ) ;
#45698 = DIRECTION ( 'NONE',  ( -4.274815082592931898E-19, -0.9999939076577903929, -0.003490651415223739937 ) ) ;
#45699 = EDGE_LOOP ( 'NONE', ( #32168, #95297, #104246, #20127 ) ) ;
#45700 = CIRCLE ( 'NONE', #127182, 0.06509327318403745899 ) ;
#45701 = CARTESIAN_POINT ( 'NONE',  ( -11.44999999999999751, 2.500000000000000000, -2.411473670974874306 ) ) ;
#45702 = CARTESIAN_POINT ( 'NONE',  ( -5.000000000000024869, 2.500000000000000000, -4.922947341949753586 ) ) ;
#45703 = ADVANCED_FACE ( 'NONE', ( #117961 ), #112460, .T. ) ;
#45704 = CARTESIAN_POINT ( 'NONE',  ( -4.400000000000028777, 2.500000000000000000, -4.776537180435978414 ) ) ;
#45705 = CARTESIAN_POINT ( 'NONE',  ( 19.40342015654640306, -2.551666867760341795, 4.359384978532470534 ) ) ;
#45706 = EDGE_CURVE ( 'NONE', #87575, #84331, #27022, .T. ) ;
#45707 = ORIENTED_EDGE ( 'NONE', *, *, #114284, .T. ) ;
#45708 = VERTEX_POINT ( 'NONE', #108144 ) ;
#45709 = EDGE_CURVE ( 'NONE', #50667, #42109, #55992, .T. ) ;
#45710 = ORIENTED_EDGE ( 'NONE', *, *, #56214, .F. ) ;
#45711 = DIRECTION ( 'NONE',  ( 0.000000000000000000, 0.000000000000000000, -1.000000000000000000 ) ) ;
#45712 = DIRECTION ( 'NONE',  ( 0.000000000000000000, 0.000000000000000000, 1.000000000000000000 ) ) ;
#45713 = DIRECTION ( 'NONE',  ( 0.000000000000000000, 1.000000000000000000, 0.000000000000000000 ) ) ;
#45714 = EDGE_CURVE ( 'NONE', #102404, #63670, #25718, .T. ) ;
#45715 = FACE_BOUND ( 'NONE', #33300, .T. ) ;
#45716 = CARTESIAN_POINT ( 'NONE',  ( 14.34999999999989662, 2.500000000000000000, 2.611473670974873151 ) ) ;
#45717 = CARTESIAN_POINT ( 'NONE',  ( -10.84999999999999964, 12.50000000000000000, 1.472243186433545459 ) ) ;
#45718 = AXIS2_PLACEMENT_3D ( 'NONE', #105347, #125611, #26146 ) ;
#45719 = DIRECTION ( 'NONE',  ( 0.000000000000000000, -0.9999939076577903929, 0.003490651415223739937 ) ) ;
#45720 = DIRECTION ( 'NONE',  ( 0.000000000000000000, 0.000000000000000000, 1.000000000000000000 ) ) ;
#45721 = AXIS2_PLACEMENT_3D ( 'NONE', #87696, #67380, #96218 ) ;
#45722 = CARTESIAN_POINT ( 'NONE',  ( 185.3385416670080872, 6.551208109652274736, 3.782341765625001351 ) ) ;
#45723 = DIRECTION ( 'NONE',  ( 0.000000000000000000, 1.000000000000000000, 0.000000000000000000 ) ) ;
#45724 = CONICAL_SURFACE ( 'NONE', #62454, 0.1000000000000002554, 0.003490658503988666988 ) ;
#45725 = DIRECTION ( 'NONE',  ( 0.000000000000000000, 1.000000000000000000, 0.000000000000000000 ) ) ;
#45726 = DIRECTION ( 'NONE',  ( -0.000000000000000000, -1.000000000000000000, -0.000000000000000000 ) ) ;
#45727 = AXIS2_PLACEMENT_3D ( 'NONE', #90272, #121680, #10442 ) ;
#45728 = ORIENTED_EDGE ( 'NONE', *, *, #12566, .F. ) ;
#45729 = ORIENTED_EDGE ( 'NONE', *, *, #110141, .F. ) ;
#45730 = ORIENTED_EDGE ( 'NONE', *, *, #27831, .T. ) ;
#45731 = ORIENTED_EDGE ( 'NONE', *, *, #108659, .F. ) ;
#45732 = CONICAL_SURFACE ( 'NONE', #39491, 0.1000000000000002554, 0.003490658503988666988 ) ;
#45733 = CARTESIAN_POINT ( 'NONE',  ( -7.100000000000017408, 12.50000000000000000, -3.637306695894650055 ) ) ;
#45734 = FACE_BOUND ( 'NONE', #41971, .T. ) ;
#45735 = CARTESIAN_POINT ( 'NONE',  ( 14.99999999999992895, 2.500000000000000000, -2.276824562219559311E-15 ) ) ;
#45737 = VECTOR ( 'NONE', #8324, 1000.000000000000000 ) ;
#45736 = VECTOR ( 'NONE', #72310, 1000.000000000000000 ) ;
#45738 = EDGE_LOOP ( 'NONE', ( #11256, #94544 ) ) ;
#45739 = CARTESIAN_POINT ( 'NONE',  ( 7.899999999999923084, 2.500000000000000000, -0.6928203230275542523 ) ) ;
#45740 = CARTESIAN_POINT ( 'NONE',  ( 8.099999999999923261, 12.50000000000000000, 3.983716857408420076 ) ) ;
#45741 = ORIENTED_EDGE ( 'NONE', *, *, #67624, .T. ) ;
#45742 = PLANE ( 'NONE',  #74115 ) ;
#45743 = CARTESIAN_POINT ( 'NONE',  ( 1.649999999999948841, 2.500000000000000000, 6.395190528383296602 ) ) ;
#45744 = EDGE_CURVE ( 'NONE', #98189, #17267, #16270, .T. ) ;
#45745 = EDGE_LOOP ( 'NONE', ( #40667, #7288, #88586, #87697 ) ) ;
#45746 = AXIS2_PLACEMENT_3D ( 'NONE', #66013, #75824, #5783 ) ;
#45747 = EDGE_CURVE ( 'NONE', #51306, #79214, #53867, .T. ) ;
#45748 = CARTESIAN_POINT ( 'NONE',  ( -4.600000000000024514, 2.500000000000000000, 0.6928203230275494784 ) ) ;
#45749 = CARTESIAN_POINT ( 'NONE',  ( 4.349999999999936584, 12.50000000000000000, 6.083687093685482772 ) ) ;
#45750 = EDGE_CURVE ( 'NONE', #59076, #22957, #70590, .T. ) ;
#45751 = EDGE_CURVE ( 'NONE', #99163, #96734, #104038, .T. ) ;
#45752 = EDGE_LOOP ( 'NONE', ( #109768, #6566 ) ) ;
#45753 = AXIS2_PLACEMENT_3D ( 'NONE', #97505, #49070, #127612 ) ;
#45754 = CARTESIAN_POINT ( 'NONE',  ( -4.800000000000022915, 2.500000000000000000, 4.083716857408420609 ) ) ;
#45755 = AXIS2_PLACEMENT_3D ( 'NONE', #65753, #28429, #55305 ) ;
#45756 = CARTESIAN_POINT ( 'NONE',  ( -13.09999999999999254, 2.500000000000000000, -3.883716857408423984 ) ) ;
#45757 = ORIENTED_EDGE ( 'NONE', *, *, #26237, .F. ) ;
#45758 = CIRCLE ( 'NONE', #24820, 0.06509327318403745899 ) ;
#45760 = ADVANCED_FACE ( 'NONE', ( #106844 ), #58078, .T. ) ;
#45759 = DIRECTION ( 'NONE',  ( -0.000000000000000000, -1.000000000000000000, -0.000000000000000000 ) ) ;
#45761 = VERTEX_POINT ( 'NONE', #15893 ) ;
#45762 = VERTEX_POINT ( 'NONE', #46025 ) ;
#45763 = CARTESIAN_POINT ( 'NONE',  ( 0.1999999999999571565, 2.500000000000000000, 3.983716857408420076 ) ) ;
#45765 = ORIENTED_EDGE ( 'NONE', *, *, #97619, .F. ) ;
#45764 = CIRCLE ( 'NONE', #20719, 0.06509327318403745899 ) ;
#45766 = DIRECTION ( 'NONE',  ( 0.000000000000000000, 1.000000000000000000, 0.000000000000000000 ) ) ;
#45767 = CARTESIAN_POINT ( 'NONE',  ( 2.899999999999946620, 12.50000000000000000, -0.6928203230275542523 ) ) ;
#45768 = ADVANCED_FACE ( 'NONE', ( #85914 ), #125846, .T. ) ;
#45769 = VECTOR ( 'NONE', #105183, 1000.000000000000000 ) ;
#45770 = ADVANCED_FACE ( 'NONE', ( #68863 ), #93662, .T. ) ;
#45771 = ORIENTED_EDGE ( 'NONE', *, *, #115310, .T. ) ;
#45772 = CARTESIAN_POINT ( 'NONE',  ( 10.64999999999991331, 12.50000000000000000, 6.213873640053559022 ) ) ;
#45773 = DIRECTION ( 'NONE',  ( -0.000000000000000000, -1.000000000000000000, -0.000000000000000000 ) ) ;
#45774 = FACE_OUTER_BOUND ( 'NONE', #31502, .T. ) ;
#45775 = DIRECTION ( 'NONE',  ( 0.000000000000000000, -0.000000000000000000, 1.000000000000000000 ) ) ;
#45776 = CARTESIAN_POINT ( 'NONE',  ( -5.400000000000023448, 2.500000000000000000, -5.122947341949753763 ) ) ;
#45778 = EDGE_CURVE ( 'NONE', #17717, #41136, #95809, .T. ) ;
#45777 = DIRECTION ( 'NONE',  ( -0.000000000000000000, -1.000000000000000000, -0.000000000000000000 ) ) ;
#45779 = AXIS2_PLACEMENT_3D ( 'NONE', #55996, #113642, #6237 ) ;
#45780 = VERTEX_POINT ( 'NONE', #110085 ) ;
#45782 = ORIENTED_EDGE ( 'NONE', *, *, #46870, .F. ) ;
#45781 = CONICAL_SURFACE ( 'NONE', #20731, 0.1000000000000002554, 0.003490658503988666988 ) ;
#45783 = DIRECTION ( 'NONE',  ( -0.000000000000000000, -1.000000000000000000, -0.000000000000000000 ) ) ;
#45784 = CARTESIAN_POINT ( 'NONE',  ( 4.199999999999939782, 2.500000000000000000, -2.276824562219559311E-15 ) ) ;
#45785 = DIRECTION ( 'NONE',  ( -0.000000000000000000, -1.000000000000000000, -0.000000000000000000 ) ) ;
#45787 = VERTEX_POINT ( 'NONE', #48593 ) ;
#45786 = EDGE_LOOP ( 'NONE', ( #56664, #117918 ) ) ;
#45788 = ORIENTED_EDGE ( 'NONE', *, *, #96526, .F. ) ;
#45789 = DIRECTION ( 'NONE',  ( 0.000000000000000000, 0.000000000000000000, -1.000000000000000000 ) ) ;
#45791 = DIRECTION ( 'NONE',  ( 0.7336674352945157240, 0.000000000000000000, 0.6795087154616692438 ) ) ;
#45790 = AXIS2_PLACEMENT_3D ( 'NONE', #98693, #10946, #110463 ) ;
#45792 = CARTESIAN_POINT ( 'NONE',  ( 187.5000000000000000, -1.000000000000025535, 7.634788798650553154 ) ) ;
#45793 = DIRECTION ( 'NONE',  ( 0.000000000000000000, 0.000000000000000000, 1.000000000000000000 ) ) ;
#45794 = DIRECTION ( 'NONE',  ( 0.000000000000000000, 0.000000000000000000, 1.000000000000000000 ) ) ;
#45795 = PLANE ( 'NONE',  #128082 ) ;
#45796 = CARTESIAN_POINT ( 'NONE',  ( -1.050000000000037348, 2.500000000000000000, -2.611473670974877592 ) ) ;
#45797 = CONICAL_SURFACE ( 'NONE', #60382, 0.1000000000000002554, 0.003490658503988666988 ) ;
#45798 = DIRECTION ( 'NONE',  ( 0.000000000000000000, 0.000000000000000000, -1.000000000000000000 ) ) ;
#45799 = DIRECTION ( 'NONE',  ( 0.000000000000000000, 0.000000000000000000, 1.000000000000000000 ) ) ;
#45800 = ORIENTED_EDGE ( 'NONE', *, *, #54545, .T. ) ;
#45801 = VECTOR ( 'NONE', #109046, 1000.000000000000000 ) ;
#45802 = DIRECTION ( 'NONE',  ( -0.000000000000000000, -1.000000000000000000, -0.000000000000000000 ) ) ;
#45803 = EDGE_LOOP ( 'NONE', ( #120624, #91579 ) ) ;
#45804 = ORIENTED_EDGE ( 'NONE', *, *, #41465, .T. ) ;
#45805 = CARTESIAN_POINT ( 'NONE',  ( 8.949999999999919353, 12.50000000000000000, 2.511473670974873507 ) ) ;
#45806 = DIRECTION ( 'NONE',  ( -0.000000000000000000, 1.000000000000000000, -0.000000000000000000 ) ) ;
#45807 = CIRCLE ( 'NONE', #114740, 0.1000000000000002554 ) ;
#45808 = CARTESIAN_POINT ( 'NONE',  ( -10.60000000000000142, 12.50000000000000000, 4.611443907251934426 ) ) ;
#45810 = CIRCLE ( 'NONE', #118957, 0.06509327318403745899 ) ;
#45809 = CARTESIAN_POINT ( 'NONE',  ( -3.150000000000029221, 2.500000000000000000, -1.718653347947326049 ) ) ;
#45811 = ADVANCED_FACE ( 'NONE', ( #80637 ), #10132, .T. ) ;
#45812 = CARTESIAN_POINT ( 'NONE',  ( 8.149999999999923972, 12.50000000000000000, 2.511473670974873507 ) ) ;
#45813 = DIRECTION ( 'NONE',  ( -0.000000000000000000, 1.000000000000000000, -0.000000000000000000 ) ) ;
#45814 = CARTESIAN_POINT ( 'NONE',  ( 10.39999999999991509, 12.50000000000000000, 0.7579135962115869374 ) ) ;
#45815 = ORIENTED_EDGE ( 'NONE', *, *, #115000, .T. ) ;
#45816 = FACE_OUTER_BOUND ( 'NONE', #85542, .T. ) ;
#45817 = VECTOR ( 'NONE', #2282, 1000.000000000000000 ) ;
#45818 = CARTESIAN_POINT ( 'NONE',  ( -3.749999999999994671, 2.500000000000000000, -6.495190528383302464 ) ) ;
#45819 = ORIENTED_EDGE ( 'NONE', *, *, #111340, .F. ) ;
#45820 = ORIENTED_EDGE ( 'NONE', *, *, #13506, .F. ) ;
#45822 = CIRCLE ( 'NONE', #73002, 0.06509327318403745899 ) ;
#45821 = AXIS2_PLACEMENT_3D ( 'NONE', #51788, #83185, #91707 ) ;
#45823 = ORIENTED_EDGE ( 'NONE', *, *, #78213, .T. ) ;
#45824 = AXIS2_PLACEMENT_3D ( 'NONE', #71657, #21928, #91946 ) ;
#45825 = ORIENTED_EDGE ( 'NONE', *, *, #8443, .T. ) ;
#45826 = LINE ( 'NONE', #115839, #125 ) ;
#45827 = FACE_OUTER_BOUND ( 'NONE', #18599, .T. ) ;
#45829 = CIRCLE ( 'NONE', #31173, 0.06509327318403745899 ) ;
#45828 = CONICAL_SURFACE ( 'NONE', #18626, 0.1000000000000002554, 0.003490658503988666988 ) ;
#45830 = FACE_OUTER_BOUND ( 'NONE', #125261, .T. ) ;
#45831 = DIRECTION ( 'NONE',  ( 0.000000000000000000, -0.9999939076577903929, 0.003490651415223739937 ) ) ;
#45832 = PLANE ( 'NONE',  #124468 ) ;
#45833 = ORIENTED_EDGE ( 'NONE', *, *, #58558, .F. ) ;
#45834 = CARTESIAN_POINT ( 'NONE',  ( -9.550000000000006040, 12.50000000000000000, -2.165063509461101710 ) ) ;
#45835 = FACE_OUTER_BOUND ( 'NONE', #96972, .T. ) ;
#45836 = VERTEX_POINT ( 'NONE', #21049 ) ;
#45837 = EDGE_LOOP ( 'NONE', ( #100980, #90903, #20129, #17320 ) ) ;
#45838 = ORIENTED_EDGE ( 'NONE', *, *, #32445, .T. ) ;
#45839 = AXIS2_PLACEMENT_3D ( 'NONE', #108834, #109496, #99687 ) ;
#45840 = CARTESIAN_POINT ( 'NONE',  ( -13.74999999999995381, 2.500000000000000000, 2.165063509461101265 ) ) ;
#45841 = LINE ( 'NONE', #125666, #52947 ) ;
#45842 = CARTESIAN_POINT ( 'NONE',  ( -5.200000000000022382, 2.500000000000000000, 4.676537180435972552 ) ) ;
#45843 = VECTOR ( 'NONE', #105881, 1000.000000000000000 ) ;
#45844 = EDGE_CURVE ( 'NONE', #14892, #86875, #89156, .T. ) ;
#45845 = ORIENTED_EDGE ( 'NONE', *, *, #92621, .F. ) ;
#45846 = CARTESIAN_POINT ( 'NONE',  ( 1.049999999999954525, 2.500000000000000000, 1.818653347947321475 ) ) ;
#45847 = FACE_OUTER_BOUND ( 'NONE', #69066, .T. ) ;
#45848 = EDGE_CURVE ( 'NONE', #18914, #107210, #118789, .T. ) ;
#45849 = CARTESIAN_POINT ( 'NONE',  ( -10.85000000000000142, 2.500000000000000000, -7.088010851410849966 ) ) ;
#45850 = PLANE ( 'NONE',  #25358 ) ;
#45851 = CARTESIAN_POINT ( 'NONE',  ( 4.149999999999941735, 12.50000000000000000, -5.737276932171712751 ) ) ;
#45852 = EDGE_CURVE ( 'NONE', #13448, #63527, #98976, .T. ) ;
#45853 = CONICAL_SURFACE ( 'NONE', #18745, 0.1000000000000002554, 0.003490658503988666988 ) ;
#45854 = VERTEX_POINT ( 'NONE', #110718 ) ;
#45855 = CIRCLE ( 'NONE', #18651, 0.06509327318403745899 ) ;
#45856 = FACE_OUTER_BOUND ( 'NONE', #32803, .T. ) ;
#45857 = ORIENTED_EDGE ( 'NONE', *, *, #96702, .F. ) ;
#45858 = EDGE_CURVE ( 'NONE', #50154, #117751, #70674, .T. ) ;
#45860 = ORIENTED_EDGE ( 'NONE', *, *, #110866, .F. ) ;
#45859 = EDGE_CURVE ( 'NONE', #50793, #33187, #116639, .T. ) ;
#45861 = ORIENTED_EDGE ( 'NONE', *, *, #128399, .T. ) ;
#45862 = EDGE_CURVE ( 'NONE', #103702, #55739, #60366, .T. ) ;
#45864 = ADVANCED_FACE ( 'NONE', ( #38800 ), #88499, .T. ) ;
#45863 = DIRECTION ( 'NONE',  ( 0.000000000000000000, 0.000000000000000000, 1.000000000000000000 ) ) ;
#45865 = ADVANCED_FACE ( 'NONE', ( #79976 ), #26854, .T. ) ;
#45866 = FACE_BOUND ( 'NONE', #17567, .T. ) ;
#45867 = CIRCLE ( 'NONE', #83435, 0.06509327318403745899 ) ;
#45868 = CARTESIAN_POINT ( 'NONE',  ( 186.0729166673494603, 4.445597072760091528, -7.700000000000049916 ) ) ;
#45869 = DIRECTION ( 'NONE',  ( 0.000000000000000000, 0.000000000000000000, 1.000000000000000000 ) ) ;
#45870 = CARTESIAN_POINT ( 'NONE',  ( 1.249999999999986899, 2.500000000000000000, 6.395190528383296602 ) ) ;
#45871 = AXIS2_PLACEMENT_3D ( 'NONE', #128606, #1549, #99767 ) ;
#45872 = AXIS2_PLACEMENT_3D ( 'NONE', #59066, #58430, #97053 ) ;
#45873 = ORIENTED_EDGE ( 'NONE', *, *, #18812, .T. ) ;
#45874 = DIRECTION ( 'NONE',  ( -0.000000000000000000, -1.000000000000000000, -0.000000000000000000 ) ) ;
#45875 = CARTESIAN_POINT ( 'NONE',  ( 0.000000000000000000, 0.000000000000000000, -5.000000000000004441 ) ) ;
#45876 = EDGE_CURVE ( 'NONE', #87229, #124, #121188, .T. ) ;
#45877 = DIRECTION ( 'NONE',  ( -0.000000000000000000, -1.000000000000000000, -0.000000000000000000 ) ) ;
#45878 = DIRECTION ( 'NONE',  ( -0.000000000000000000, -1.000000000000000000, -0.000000000000000000 ) ) ;
#45879 = ORIENTED_EDGE ( 'NONE', *, *, #90285, .F. ) ;
#45880 = DIRECTION ( 'NONE',  ( -0.000000000000000000, 1.000000000000000000, -0.000000000000000000 ) ) ;
#45881 = CARTESIAN_POINT ( 'NONE',  ( 1.449999999999952660, 2.500000000000000000, -6.841600689897078702 ) ) ;
#45882 = AXIS2_PLACEMENT_3D ( 'NONE', #17905, #116110, #86651 ) ;
#45883 = VERTEX_POINT ( 'NONE', #89796 ) ;
#45884 = CARTESIAN_POINT ( 'NONE',  ( 11.44999999999990692, 12.50000000000000000, 1.883746621131358934 ) ) ;
#45885 = FACE_BOUND ( 'NONE', #110637, .T. ) ;
#45886 = CARTESIAN_POINT ( 'NONE',  ( 13.54999999999989768, 12.50000000000000000, -2.576566944158915184 ) ) ;
#45887 = ORIENTED_EDGE ( 'NONE', *, *, #121541, .F. ) ;
#45888 = CARTESIAN_POINT ( 'NONE',  ( 105.0000000000000142, 9.000000000000001776, -0.2499999999999996392 ) ) ;
#45889 = CARTESIAN_POINT ( 'NONE',  ( -1.850000000000033840, 2.500000000000000000, 2.511473670974873507 ) ) ;
#45890 = ORIENTED_EDGE ( 'NONE', *, *, #38640, .T. ) ;
#45891 = VERTEX_POINT ( 'NONE', #50509 ) ;
#45892 = CARTESIAN_POINT ( 'NONE',  ( 184.8385416670080872, 6.551208109652274736, 3.782341765625001351 ) ) ;
#45893 = AXIS2_PLACEMENT_3D ( 'NONE', #62388, #13904, #33571 ) ;
#45894 = VERTEX_POINT ( 'NONE', #59058 ) ;
#45895 = CARTESIAN_POINT ( 'NONE',  ( 185.4635416670080872, -4.367472073101520635, 7.564683531249999149 ) ) ;
#45896 = DIRECTION ( 'NONE',  ( 0.000000000000000000, 1.224646799147353454E-16, 1.000000000000000000 ) ) ;
#45897 = CARTESIAN_POINT ( 'NONE',  ( 0.3999999999999559464, 2.500000000000000000, -4.330127018922201643 ) ) ;
#45898 = DIRECTION ( 'NONE',  ( 0.000000000000000000, 0.000000000000000000, -1.000000000000000000 ) ) ;
#45899 = ADVANCED_FACE ( 'NONE', ( #766 ), #60977, .T. ) ;
#45900 = EDGE_CURVE ( 'NONE', #53553, #61962, #11225, .T. ) ;
#45901 = FACE_OUTER_BOUND ( 'NONE', #84567, .T. ) ;
#45902 = AXIS2_PLACEMENT_3D ( 'NONE', #120632, #119993, #21804 ) ;
#45903 = ADVANCED_FACE ( 'NONE', ( #71429 ), #100018, .T. ) ;
#45904 = ORIENTED_EDGE ( 'NONE', *, *, #21162, .F. ) ;
#45905 = ADVANCED_FACE ( 'NONE', ( #49251 ), #127128, .T. ) ;
#45906 = VERTEX_POINT ( 'NONE', #81898 ) ;
#45907 = CARTESIAN_POINT ( 'NONE',  ( 7.499999999999925393, 2.500000000000000000, -3.637306695894650055 ) ) ;
#45909 = CONICAL_SURFACE ( 'NONE', #16539, 0.09999999999999982514, 0.003490658503988666988 ) ;
#45908 = CIRCLE ( 'NONE', #37507, 0.1000000000000002554 ) ;
#45910 = DIRECTION ( 'NONE',  ( -0.000000000000000000, 1.000000000000000000, -0.000000000000000000 ) ) ;
#45911 = PLANE ( 'NONE',  #5340 ) ;
#45912 = DIRECTION ( 'NONE',  ( -0.000000000000000000, 1.000000000000000000, -0.000000000000000000 ) ) ;
#45913 = AXIS2_PLACEMENT_3D ( 'NONE', #106904, #106272, #55248 ) ;
#45915 = ORIENTED_EDGE ( 'NONE', *, *, #111782, .F. ) ;
#45914 = EDGE_LOOP ( 'NONE', ( #94994, #107625 ) ) ;
#45916 = FACE_BOUND ( 'NONE', #102595, .T. ) ;
#45917 = EDGE_LOOP ( 'NONE', ( #49816, #16028, #24054, #122532 ) ) ;
#45918 = EDGE_CURVE ( 'NONE', #40453, #22266, #42658, .T. ) ;
#45919 = FACE_OUTER_BOUND ( 'NONE', #114275, .T. ) ;
#45920 = DIRECTION ( 'NONE',  ( 0.000000000000000000, 0.000000000000000000, 1.000000000000000000 ) ) ;
#45922 = ORIENTED_EDGE ( 'NONE', *, *, #109842, .T. ) ;
#45921 = EDGE_CURVE ( 'NONE', #5769, #78285, #62287, .T. ) ;
#45923 = DIRECTION ( 'NONE',  ( -0.000000000000000000, -1.000000000000000000, -0.000000000000000000 ) ) ;
#45926 = CARTESIAN_POINT ( 'NONE',  ( -10.84999999999999964, 12.50000000000000000, 2.922977105672686982 ) ) ;
#45925 = AXIS2_PLACEMENT_3D ( 'NONE', #47466, #70803, #102210 ) ;
#45924 = AXIS2_PLACEMENT_3D ( 'NONE', #96032, #56721, #117573 ) ;
#45927 = EDGE_CURVE ( 'NONE', #19851, #59088, #106275, .T. ) ;
#45928 = CARTESIAN_POINT ( 'NONE',  ( -9.350000000000008527, 2.500000000000000000, -6.148780366869520897 ) ) ;
#45929 = EDGE_CURVE ( 'NONE', #109646, #17565, #73371, .T. ) ;
#45930 = PLANE ( 'NONE',  #103008 ) ;
#45931 = DIRECTION ( 'NONE',  ( 0.000000000000000000, 0.000000000000000000, 1.000000000000000000 ) ) ;
#45932 = DIRECTION ( 'NONE',  ( 0.000000000000000000, 0.000000000000000000, 1.000000000000000000 ) ) ;
#45933 = CARTESIAN_POINT ( 'NONE',  ( 186.5677083336747160, -4.367472073101514418, -7.564683531250002702 ) ) ;
#45934 = FACE_OUTER_BOUND ( 'NONE', #65888, .T. ) ;
#45936 = EDGE_CURVE ( 'NONE', #35458, #111625, #60238, .T. ) ;
#45935 = CARTESIAN_POINT ( 'NONE',  ( -1.850000000000033840, 2.500000000000000000, 6.048780366869521252 ) ) ;
#45937 = ORIENTED_EDGE ( 'NONE', *, *, #35533, .F. ) ;
#45938 = ORIENTED_EDGE ( 'NONE', *, *, #113906, .T. ) ;
#45939 = DIRECTION ( 'NONE',  ( -1.000000000000000000, -0.000000000000000000, -0.000000000000000000 ) ) ;
#45940 = ORIENTED_EDGE ( 'NONE', *, *, #70567, .F. ) ;
#45941 = CARTESIAN_POINT ( 'NONE',  ( -6.650000000000018119, 2.500000000000000000, -2.857883832488653741 ) ) ;
#45943 = ORIENTED_EDGE ( 'NONE', *, *, #50963, .F. ) ;
#45942 = EDGE_LOOP ( 'NONE', ( #92782, #92072, #39757, #16650 ) ) ;
#45944 = ORIENTED_EDGE ( 'NONE', *, *, #69245, .F. ) ;
#45945 = FACE_OUTER_BOUND ( 'NONE', #51357, .T. ) ;
#45946 = AXIS2_PLACEMENT_3D ( 'NONE', #13954, #24431, #64351 ) ;
#45947 = AXIS2_PLACEMENT_3D ( 'NONE', #88121, #78351, #116099 ) ;
#45948 = DIRECTION ( 'NONE',  ( 0.000000000000000000, 0.000000000000000000, 1.000000000000000000 ) ) ;
#45949 = CARTESIAN_POINT ( 'NONE',  ( 14.59999999999989484, 2.500000000000000000, 0.6928203230275494784 ) ) ;
#45950 = DIRECTION ( 'NONE',  ( 0.000000000000000000, 1.000000000000000000, 0.000000000000000000 ) ) ;
#45951 = CARTESIAN_POINT ( 'NONE',  ( 87.50000000000001421, 0.000000000000000000, 0.000000000000000000 ) ) ;
#45952 = ADVANCED_FACE ( 'NONE', ( #62917 ), #3982, .T. ) ;
#45953 = ORIENTED_EDGE ( 'NONE', *, *, #20602, .F. ) ;
#45954 = AXIS2_PLACEMENT_3D ( 'NONE', #28936, #49872, #88472 ) ;
#45957 = CIRCLE ( 'NONE', #121155, 0.06509327318403745899 ) ;
#45956 = CARTESIAN_POINT ( 'NONE',  ( -11.04999999999999893, 12.50000000000000000, 6.083687093685482772 ) ) ;
#45955 = AXIS2_PLACEMENT_3D ( 'NONE', #96492, #105699, #57230 ) ;
#45958 = ORIENTED_EDGE ( 'NONE', *, *, #14322, .F. ) ;
#45959 = VERTEX_POINT ( 'NONE', #61640 ) ;
#45960 = ORIENTED_EDGE ( 'NONE', *, *, #39285, .F. ) ;
#45961 = VERTEX_POINT ( 'NONE', #54376 ) ;
#45962 = CARTESIAN_POINT ( 'NONE',  ( 15.39999999999989200, 12.50000000000000000, -0.6928203230275542523 ) ) ;
#45963 = VERTEX_POINT ( 'NONE', #112023 ) ;
#45964 = VERTEX_POINT ( 'NONE', #93029 ) ;
#45965 = AXIS2_PLACEMENT_3D ( 'NONE', #51845, #101583, #129136 ) ;
#45966 = DIRECTION ( 'NONE',  ( 0.000000000000000000, -0.000000000000000000, 1.000000000000000000 ) ) ;
#45967 = AXIS2_PLACEMENT_3D ( 'NONE', #35544, #76745, #57094 ) ;
#45968 = DIRECTION ( 'NONE',  ( 0.000000000000000000, 1.000000000000000000, 0.000000000000000000 ) ) ;
#45969 = DIRECTION ( 'NONE',  ( -0.000000000000000000, 1.000000000000000000, -0.000000000000000000 ) ) ;
#45970 = VECTOR ( 'NONE', #101565, 1000.000000000000000 ) ;
#45971 = EDGE_CURVE ( 'NONE', #104801, #124539, #120850, .T. ) ;
#45972 = DIRECTION ( 'NONE',  ( 0.000000000000000000, 1.000000000000000000, 0.000000000000000000 ) ) ;
#45973 = LINE ( 'NONE', #108735, #13625 ) ;
#45974 = CARTESIAN_POINT ( 'NONE',  ( 1.849999999999949685, 12.50000000000000000, -2.446380397790840266 ) ) ;
#45975 = ORIENTED_EDGE ( 'NONE', *, *, #33736, .T. ) ;
#45976 = DIRECTION ( 'NONE',  ( -0.000000000000000000, -1.000000000000000000, -0.000000000000000000 ) ) ;
#45977 = VECTOR ( 'NONE', #61639, 1000.000000000000000 ) ;
#45978 = EDGE_LOOP ( 'NONE', ( #116881, #25657, #70684, #77115 ) ) ;
#45979 = FACE_OUTER_BOUND ( 'NONE', #20175, .T. ) ;
#45980 = ORIENTED_EDGE ( 'NONE', *, *, #110264, .F. ) ;
#45981 = DIRECTION ( 'NONE',  ( 0.000000000000000000, 1.000000000000000000, 0.000000000000000000 ) ) ;
#45982 = CONICAL_SURFACE ( 'NONE', #129533, 0.1000000000000000056, 0.003490658503988666988 ) ;
#45983 = EDGE_LOOP ( 'NONE', ( #71209, #26044, #43977, #69118 ) ) ;
#45984 = EDGE_CURVE ( 'NONE', #17050, #52727, #76939, .T. ) ;
#45985 = EDGE_LOOP ( 'NONE', ( #72981, #71406 ) ) ;
#45986 = DIRECTION ( 'NONE',  ( -0.000000000000000000, 1.000000000000000000, -0.000000000000000000 ) ) ;
#45987 = DIRECTION ( 'NONE',  ( -0.000000000000000000, 1.000000000000000000, -0.000000000000000000 ) ) ;
#45988 = CARTESIAN_POINT ( 'NONE',  ( 184.5000000000000000, 0.000000000000000000, 0.000000000000000000 ) ) ;
#45989 = FACE_OUTER_BOUND ( 'NONE', #51666, .T. ) ;
#45990 = DIRECTION ( 'NONE',  ( 0.000000000000000000, 1.000000000000000000, 0.000000000000000000 ) ) ;
#45991 = EDGE_LOOP ( 'NONE', ( #83080, #55277, #35315, #19362 ) ) ;
#45992 =( BOUNDED_CURVE ( )  B_SPLINE_CURVE ( 2, ( #31625, #101657, #11968, #42760, #82667, #122582, #15832 ),
 .UNSPECIFIED., .F., .F. ) 
 B_SPLINE_CURVE_WITH_KNOTS ( ( 3, 2, 2, 3 ),
 ( 0.5714285714285719520, 0.5952380952380957879, 0.6190476190476195129, 0.6428571428571433488 ),
 .UNSPECIFIED. ) 
 CURVE ( )  GEOMETRIC_REPRESENTATION_ITEM ( )  RATIONAL_B_SPLINE_CURVE ( ( 0.9999999999999968914, 0.8660254037844418162, 1.000000000000000000, 0.8660254037844387076, 1.000000000000000000, 0.8660254037844361541, 1.000000000000002442 ) ) 
 REPRESENTATION_ITEM ( '' )  );
#45993 = DIRECTION ( 'NONE',  ( 0.000000000000000000, 1.000000000000000000, 0.000000000000000000 ) ) ;
#45994 = DIRECTION ( 'NONE',  ( -0.000000000000000000, 1.000000000000000000, -0.000000000000000000 ) ) ;
#45995 = LINE ( 'NONE', #8607, #106354 ) ;
#45996 = CARTESIAN_POINT ( 'NONE',  ( -0.4500000000000402012, 2.500000000000000000, 2.165063509461097713 ) ) ;
#45997 = CARTESIAN_POINT ( 'NONE',  ( -9.150000000000011013, 2.500000000000000000, -5.702370205355745014 ) ) ;
#45998 = EDGE_LOOP ( 'NONE', ( #126808, #68203, #65812, #116993 ) ) ;
#45999 = ORIENTED_EDGE ( 'NONE', *, *, #78998, .F. ) ;
#46000 = FACE_OUTER_BOUND ( 'NONE', #26756, .T. ) ;
#46001 = AXIS2_PLACEMENT_3D ( 'NONE', #119659, #50289, #39844 ) ;
#46002 = ORIENTED_EDGE ( 'NONE', *, *, #16879, .F. ) ;
#46003 = DIRECTION ( 'NONE',  ( -0.000000000000000000, 1.000000000000000000, -0.000000000000000000 ) ) ;
#46004 = DIRECTION ( 'NONE',  ( 0.000000000000000000, 0.000000000000000000, 1.000000000000000000 ) ) ;
#46005 = EDGE_CURVE ( 'NONE', #69398, #99498, #41993, .T. ) ;
#46007 = CONICAL_SURFACE ( 'NONE', #112899, 0.1000000000000000472, 0.003490658503988666988 ) ;
#46006 = VECTOR ( 'NONE', #103786, 1000.000000000000000 ) ;
#46008 = ORIENTED_EDGE ( 'NONE', *, *, #24588, .F. ) ;
#46009 = CARTESIAN_POINT ( 'NONE',  ( 185.5416666666666572, -4.445597072760122614, 7.699999999999998401 ) ) ;
#46010 = CARTESIAN_POINT ( 'NONE',  ( 3.349999999999944578, 12.50000000000000000, -5.802370205355749988 ) ) ;
#46011 = PLANE ( 'NONE',  #125976 ) ;
#46012 = SURFACE_STYLE_USAGE ( .BOTH. , #27012 ) ;
#46013 = CARTESIAN_POINT ( 'NONE',  ( 4.999999999999936939, 2.500000000000000000, -3.537306695894649966 ) ) ;
#46014 = VERTEX_POINT ( 'NONE', #43294 ) ;
#46016 = CIRCLE ( 'NONE', #31352, 0.06509327318403745899 ) ;
#46015 = CONICAL_SURFACE ( 'NONE', #81517, 0.1000000000000000472, 0.003490658503988666988 ) ;
#46017 = DIRECTION ( 'NONE',  ( 0.000000000000000000, -0.000000000000000000, 1.000000000000000000 ) ) ;
#46018 = DIRECTION ( 'NONE',  ( -4.274815082592931898E-19, -0.9999939076577903929, -0.003490651415223739937 ) ) ;
#46019 = VERTEX_POINT ( 'NONE', #102208 ) ;
#46020 = ADVANCED_FACE ( 'NONE', ( #122491 ), #74888, .T. ) ;
#46021 = EDGE_CURVE ( 'NONE', #1757, #23452, #18444, .T. ) ;
#46022 = EDGE_CURVE ( 'NONE', #103763, #15166, #102076, .T. ) ;
#46024 = EDGE_CURVE ( 'NONE', #83715, #24243, #37242, .T. ) ;
#46023 = CARTESIAN_POINT ( 'NONE',  ( -13.09999999999999076, 12.50000000000000000, 3.983716857408420964 ) ) ;
#46025 = CARTESIAN_POINT ( 'NONE',  ( 13.94999999999989448, 12.50000000000000000, -2.446380397790840266 ) ) ;
#46026 = DIRECTION ( 'NONE',  ( 0.000000000000000000, 0.000000000000000000, 1.000000000000000000 ) ) ;
#46027 = ORIENTED_EDGE ( 'NONE', *, *, #67216, .T. ) ;
#46028 = CARTESIAN_POINT ( 'NONE',  ( -6.900000000000019007, 2.500000000000000000, -4.576537180435978236 ) ) ;
#46029 = EDGE_LOOP ( 'NONE', ( #25154, #42149 ) ) ;
#46030 = CARTESIAN_POINT ( 'NONE',  ( -12.09999999999999609, 12.50000000000000000, 0.06509327318403916596 ) ) ;
#46031 = CARTESIAN_POINT ( 'NONE',  ( 3.099999999999945022, 2.500000000000000000, -0.3464101615137783474 ) ) ;
#46032 = ADVANCED_FACE ( 'NONE', ( #34109 ), #5898, .T. ) ;
#46033 = DIRECTION ( 'NONE',  ( -4.274815082592931898E-19, -0.9999939076577903929, -0.003490651415223739937 ) ) ;
#46034 = ORIENTED_EDGE ( 'NONE', *, *, #102303, .F. ) ;
#46035 = ADVANCED_FACE ( 'NONE', ( #53738 ), #94296, .T. ) ;
#46036 = AXIS2_PLACEMENT_3D ( 'NONE', #37892, #128224, #116443 ) ;
#46038 = EDGE_CURVE ( 'NONE', #86983, #128651, #58175, .T. ) ;
#46037 = DIRECTION ( 'NONE',  ( -0.000000000000000000, 1.000000000000000000, -0.000000000000000000 ) ) ;
#46039 = AXIS2_PLACEMENT_3D ( 'NONE', #22148, #49025, #20838 ) ;
#46040 = DIRECTION ( 'NONE',  ( 0.000000000000000000, 1.000000000000000000, 0.000000000000000000 ) ) ;
#46041 = ORIENTED_EDGE ( 'NONE', *, *, #48543, .T. ) ;
#46042 = EDGE_LOOP ( 'NONE', ( #109773, #103620, #20371, #49815 ) ) ;
#46043 = VECTOR ( 'NONE', #2518, 1000.000000000000000 ) ;
#46044 = DIRECTION ( 'NONE',  ( -4.274815082592931898E-19, -0.9999939076577903929, -0.003490651415223739937 ) ) ;
#46045 = ORIENTED_EDGE ( 'NONE', *, *, #20566, .F. ) ;
#46046 = CARTESIAN_POINT ( 'NONE',  ( 9.799999999999915445, 2.500000000000000000, -4.676537180435977881 ) ) ;
#46047 = CARTESIAN_POINT ( 'NONE',  ( -4.600000000000028066, 12.50000000000000000, -5.088040615133791356 ) ) ;
#46048 = VERTEX_POINT ( 'NONE', #84317 ) ;
#46049 = CIRCLE ( 'NONE', #96198, 0.06509327318403745899 ) ;
#46050 = FACE_OUTER_BOUND ( 'NONE', #122334, .T. ) ;
#46051 = DIRECTION ( 'NONE',  ( 0.000000000000000000, -0.9999939076577903929, 0.003490651415223739937 ) ) ;
#46052 = ORIENTED_EDGE ( 'NONE', *, *, #121368, .F. ) ;
#46054 = CARTESIAN_POINT ( 'NONE',  ( 10.59999999999990905, 2.500000000000000000, -3.983716857408426293 ) ) ;
#46053 = AXIS2_PLACEMENT_3D ( 'NONE', #117130, #107332, #57602 ) ;
#46055 = DIRECTION ( 'NONE',  ( -0.000000000000000000, 1.000000000000000000, -0.000000000000000000 ) ) ;
#46056 = CIRCLE ( 'NONE', #75368, 0.09999999999999999167 ) ;
#46057 = CARTESIAN_POINT ( 'NONE',  ( 9.799999999999918998, 2.500000000000000000, -0.3464101615137782364 ) ) ;
#46058 = CARTESIAN_POINT ( 'NONE',  ( -6.250000000000015987, 12.50000000000000000, 5.802370205355744659 ) ) ;
#46059 = DIRECTION ( 'NONE',  ( 0.000000000000000000, 0.000000000000000000, -1.000000000000000000 ) ) ;
#46060 = AXIS2_PLACEMENT_3D ( 'NONE', #121039, #81748, #101409 ) ;
#46061 = ORIENTED_EDGE ( 'NONE', *, *, #7238, .T. ) ;
#46062 = VERTEX_POINT ( 'NONE', #102034 ) ;
#46063 = EDGE_LOOP ( 'NONE', ( #72511, #1164 ) ) ;
#46064 = EDGE_LOOP ( 'NONE', ( #27109, #105137, #70777, #53699 ) ) ;
#46065 = DIRECTION ( 'NONE',  ( -0.000000000000000000, 1.000000000000000000, -0.000000000000000000 ) ) ;
#46066 = DIRECTION ( 'NONE',  ( 0.000000000000000000, 1.000000000000000000, 0.000000000000000000 ) ) ;
#46067 = DIRECTION ( 'NONE',  ( 0.000000000000000000, -0.000000000000000000, 1.000000000000000000 ) ) ;
#46068 = EDGE_LOOP ( 'NONE', ( #111445, #77169, #72666, #20823 ) ) ;
#46069 = FACE_BOUND ( 'NONE', #1443, .T. ) ;
#46070 = CARTESIAN_POINT ( 'NONE',  ( 14.59999999999989484, 12.50000000000000000, -2.276824562219559311E-15 ) ) ;
#46071 = CARTESIAN_POINT ( 'NONE',  ( 5.449999999999934452, 12.50000000000000000, 2.165063509461097713 ) ) ;
#46072 = ADVANCED_FACE ( 'NONE', ( #104596 ), #81152, .T. ) ;
#46073 = DIRECTION ( 'NONE',  ( 0.000000000000000000, 0.000000000000000000, -1.000000000000000000 ) ) ;
#46074 = CARTESIAN_POINT ( 'NONE',  ( 1.249999999999986899, 12.50000000000000000, 6.495190528383297135 ) ) ;
#46075 = ADVANCED_FACE ( 'NONE', ( #45058 ), #33132, .T. ) ;
#46076 = CARTESIAN_POINT ( 'NONE',  ( -5.200000000000024158, 2.500000000000000000, -4.776537180435977525 ) ) ;
#46077 = DIRECTION ( 'NONE',  ( -0.000000000000000000, 1.000000000000000000, -0.000000000000000000 ) ) ;
#46078 = DIRECTION ( 'NONE',  ( 0.000000000000000000, 0.000000000000000000, 1.000000000000000000 ) ) ;
#46079 = FACE_OUTER_BOUND ( 'NONE', #21603, .T. ) ;
#46080 = DIRECTION ( 'NONE',  ( 0.000000000000000000, -0.9999939076577903929, 0.003490651415223739937 ) ) ;
#46082 = EDGE_CURVE ( 'NONE', #24019, #110675, #44392, .T. ) ;
#46081 = CARTESIAN_POINT ( 'NONE',  ( 8.549999999999924327, 2.500000000000000000, 1.918653347947321564 ) ) ;
#46083 = ORIENTED_EDGE ( 'NONE', *, *, #66259, .F. ) ;
#46084 = EDGE_LOOP ( 'NONE', ( #39044, #32386, #50353, #53123 ) ) ;
#46085 = VERTEX_POINT ( 'NONE', #93501 ) ;
#46086 = ORIENTED_EDGE ( 'NONE', *, *, #94030, .F. ) ;
#46087 = FACE_OUTER_BOUND ( 'NONE', #32510, .T. ) ;
#46088 = EDGE_LOOP ( 'NONE', ( #789, #11043, #96400, #36824 ) ) ;
#46089 = DIRECTION ( 'NONE',  ( 0.000000000000000000, 1.000000000000000000, 0.000000000000000000 ) ) ;
#46090 = CIRCLE ( 'NONE', #123431, 0.09999999999999982514 ) ;
#46091 = ORIENTED_EDGE ( 'NONE', *, *, #62821, .F. ) ;
#46092 = VERTEX_POINT ( 'NONE', #2513 ) ;
#46093 = CARTESIAN_POINT ( 'NONE',  ( 3.749999999999978684, 2.500000000000000000, -2.165063509461101710 ) ) ;
#46094 = CIRCLE ( 'NONE', #14673, 0.09999999999999982514 ) ;
#46095 = DIRECTION ( 'NONE',  ( -0.000000000000000000, -1.000000000000000000, -0.000000000000000000 ) ) ;
#46096 = DIRECTION ( 'NONE',  ( 0.000000000000000000, 0.000000000000000000, 1.000000000000000000 ) ) ;
#46097 = DIRECTION ( 'NONE',  ( 0.000000000000000000, 0.000000000000000000, -1.000000000000000000 ) ) ;
#46098 = PLANE ( 'NONE',  #116615 ) ;
#46099 = ORIENTED_EDGE ( 'NONE', *, *, #105752, .F. ) ;
#46100 = ORIENTED_EDGE ( 'NONE', *, *, #25069, .F. ) ;
#46101 = ORIENTED_EDGE ( 'NONE', *, *, #39824, .T. ) ;
#46102 = VERTEX_POINT ( 'NONE', #12349 ) ;
#46103 = DIRECTION ( 'NONE',  ( 0.000000000000000000, 1.000000000000000000, 0.000000000000000000 ) ) ;
#46104 = ORIENTED_EDGE ( 'NONE', *, *, #50563, .F. ) ;
#46105 = ORIENTED_EDGE ( 'NONE', *, *, #102331, .F. ) ;
#46106 = CARTESIAN_POINT ( 'NONE',  ( 8.349999999999919709, 2.500000000000000000, -1.372243186433550033 ) ) ;
#46107 = DIRECTION ( 'NONE',  ( 0.000000000000000000, -0.000000000000000000, 1.000000000000000000 ) ) ;
#46108 = CARTESIAN_POINT ( 'NONE',  ( 5.199999999999935341, 2.500000000000000000, -0.3464101615137783474 ) ) ;
#46109 = ADVANCED_FACE ( 'NONE', ( #64673 ), #100113, .T. ) ;
#46110 = DIRECTION ( 'NONE',  ( 0.000000000000000000, 1.000000000000000000, 0.000000000000000000 ) ) ;
#46111 = CARTESIAN_POINT ( 'NONE',  ( 4.999999999999933387, 2.500000000000000000, 5.122947341949749323 ) ) ;
#46112 = DIRECTION ( 'NONE',  ( 0.000000000000000000, 0.000000000000000000, 1.000000000000000000 ) ) ;
#46113 = VERTEX_POINT ( 'NONE', #92196 ) ;
#46114 = DIRECTION ( 'NONE',  ( 0.000000000000000000, 0.000000000000000000, 1.000000000000000000 ) ) ;
#46115 = AXIS2_PLACEMENT_3D ( 'NONE', #58038, #35810, #117557 ) ;
#46116 = ORIENTED_EDGE ( 'NONE', *, *, #127473, .F. ) ;
#46117 = CARTESIAN_POINT ( 'NONE',  ( 4.349999999999941025, 12.50000000000000000, -6.083687093685488989 ) ) ;
#46118 = VERTEX_POINT ( 'NONE', #53583 ) ;
#46119 = DIRECTION ( 'NONE',  ( 0.000000000000000000, -0.000000000000000000, 1.000000000000000000 ) ) ;
#46120 = DIRECTION ( 'NONE',  ( 0.000000000000000000, -0.9999939076577903929, 0.003490651415223739937 ) ) ;
#46121 = ADVANCED_FACE ( 'NONE', ( #52931 ), #116819, .T. ) ;
#46122 = ORIENTED_EDGE ( 'NONE', *, *, #84766, .T. ) ;
#46123 = DIRECTION ( 'NONE',  ( 0.000000000000000000, -0.000000000000000000, 1.000000000000000000 ) ) ;
#46124 = ADVANCED_FACE ( 'NONE', ( #3198 ), #103324, .T. ) ;
#46125 = FACE_OUTER_BOUND ( 'NONE', #6734, .T. ) ;
#46126 = ORIENTED_EDGE ( 'NONE', *, *, #12910, .F. ) ;
#46127 = VECTOR ( 'NONE', #36531, 1000.000000000000000 ) ;
#46128 = LINE ( 'NONE', #125966, #23642 ) ;
#46129 = EDGE_LOOP ( 'NONE', ( #60495, #16507, #7580, #55358 ) ) ;
#46131 = VERTEX_POINT ( 'NONE', #43137 ) ;
#46130 = EDGE_CURVE ( 'NONE', #14663, #70719, #49960, .T. ) ;
#46132 = CARTESIAN_POINT ( 'NONE',  ( 6.699999999999928235, 2.500000000000000000, 0.09999999999999772959 ) ) ;
#46133 = DIRECTION ( 'NONE',  ( -4.274815082592931898E-19, -0.9999939076577903929, -0.003490651415223739937 ) ) ;
#46134 = CARTESIAN_POINT ( 'NONE',  ( 186.6718750003414016, 9.264065473108010111E-16, -7.564683531250000925 ) ) ;
#46135 = CARTESIAN_POINT ( 'NONE',  ( -12.49999999999995914, 12.50000000000000000, -4.265033745738161741 ) ) ;
#46136 = CONICAL_SURFACE ( 'NONE', #12755, 0.1000000000000002554, 0.003490658503988666988 ) ;
#46137 = CIRCLE ( 'NONE', #85832, 0.1000000000000000056 ) ;
#46138 = DIRECTION ( 'NONE',  ( 0.000000000000000000, 0.000000000000000000, 1.000000000000000000 ) ) ;
#46139 = CARTESIAN_POINT ( 'NONE',  ( 9.149999999999916866, 2.500000000000000000, 5.702370205355745014 ) ) ;
#46140 = AXIS2_PLACEMENT_3D ( 'NONE', #4453, #15582, #7044 ) ;
#46141 = ORIENTED_EDGE ( 'NONE', *, *, #88119, .F. ) ;
#46142 = CARTESIAN_POINT ( 'NONE',  ( 65.39885637503600435, 3.129858735933689573, -5.811318689367469759 ) ) ;
#46143 = EDGE_CURVE ( 'NONE', #124287, #88819, #3953, .T. ) ;
#46144 = ORIENTED_EDGE ( 'NONE', *, *, #20211, .F. ) ;
#46145 = CIRCLE ( 'NONE', #62881, 0.1000000000000002554 ) ;
#46146 = CARTESIAN_POINT ( 'NONE',  ( -13.94999999999998863, 2.500000000000000000, 2.511473670974877503 ) ) ;
#46147 = CARTESIAN_POINT ( 'NONE',  ( -8.550000000000014921, 2.500000000000000000, -6.248780366869521430 ) ) ;
#46148 = LINE ( 'NONE', #48743, #14581 ) ;
#46149 = EDGE_LOOP ( 'NONE', ( #125086, #113694, #58622, #52333 ) ) ;
#46150 = EDGE_CURVE ( 'NONE', #25156, #79978, #23462, .T. ) ;
#46151 = CARTESIAN_POINT ( 'NONE',  ( -7.100000000000018296, 12.50000000000000000, -0.06509327318403980434 ) ) ;
#46152 = CARTESIAN_POINT ( 'NONE',  ( -6.450000000000017941, 2.500000000000000000, -2.411473670974877859 ) ) ;
#46153 = ADVANCED_FACE ( 'NONE', ( #5103 ), #35281, .T. ) ;
#46154 = EDGE_CURVE ( 'NONE', #98777, #85834, #112634, .T. ) ;
#46155 = EDGE_CURVE ( 'NONE', #82690, #111766, #129384, .T. ) ;
#46156 = EDGE_CURVE ( 'NONE', #100484, #123441, #10227, .T. ) ;
#46157 = ORIENTED_EDGE ( 'NONE', *, *, #118396, .F. ) ;
#46158 = DIRECTION ( 'NONE',  ( 0.000000000000000000, -0.9999939076577903929, 0.003490651415223739937 ) ) ;
#46159 = ORIENTED_EDGE ( 'NONE', *, *, #78360, .F. ) ;
#46160 = ORIENTED_EDGE ( 'NONE', *, *, #117855, .T. ) ;
#46161 = DIRECTION ( 'NONE',  ( -0.000000000000000000, 1.000000000000000000, -0.000000000000000000 ) ) ;
#46162 = EDGE_CURVE ( 'NONE', #75844, #104306, #108416, .T. ) ;
#46163 = AXIS2_PLACEMENT_3D ( 'NONE', #44836, #35028, #74931 ) ;
#46164 = AXIS2_PLACEMENT_3D ( 'NONE', #100511, #61901, #101816 ) ;
#46165 = EDGE_CURVE ( 'NONE', #33390, #30210, #85433, .T. ) ;
#46166 = ORIENTED_EDGE ( 'NONE', *, *, #34242, .T. ) ;
#46167 = CYLINDRICAL_SURFACE ( 'NONE', #90458, 7.700000000000000178 ) ;
#46168 = DIRECTION ( 'NONE',  ( 0.000000000000000000, -0.000000000000000000, 1.000000000000000000 ) ) ;
#46169 = CARTESIAN_POINT ( 'NONE',  ( 12.89999999999990266, 2.500000000000000000, 3.737306695894644371 ) ) ;
#46170 = ORIENTED_EDGE ( 'NONE', *, *, #100734, .F. ) ;
#46171 = EDGE_CURVE ( 'NONE', #53159, #110767, #14276, .T. ) ;
#46174 = EDGE_CURVE ( 'NONE', #79117, #110068, #4434, .T. ) ;
#46173 = FACE_BOUND ( 'NONE', #123867, .T. ) ;
#46172 = CONICAL_SURFACE ( 'NONE', #56616, 0.1000000000000000472, 0.003490658503988666988 ) ;
#46176 = ORIENTED_EDGE ( 'NONE', *, *, #71286, .T. ) ;
#46175 = DIRECTION ( 'NONE',  ( 0.000000000000000000, 1.000000000000000000, 0.000000000000000000 ) ) ;
#46177 = AXIS2_PLACEMENT_3D ( 'NONE', #31148, #2961, #40972 ) ;
#46178 = FACE_OUTER_BOUND ( 'NONE', #81121, .T. ) ;
#46179 = EDGE_CURVE ( 'NONE', #68357, #40294, #79193, .T. ) ;
#46180 = CARTESIAN_POINT ( 'NONE',  ( 1.899999999999951283, 2.500000000000000000, -0.4464101615137782142 ) ) ;
#46181 = EDGE_CURVE ( 'NONE', #76087, #53767, #20596, .T. ) ;
#46182 = ORIENTED_EDGE ( 'NONE', *, *, #69473, .T. ) ;
#46183 = ORIENTED_EDGE ( 'NONE', *, *, #54314, .F. ) ;
#46184 = ORIENTED_EDGE ( 'NONE', *, *, #71291, .F. ) ;
#46185 = DIRECTION ( 'NONE',  ( 0.000000000000000000, 0.000000000000000000, 1.000000000000000000 ) ) ;
#46186 = FACE_OUTER_BOUND ( 'NONE', #28379, .T. ) ;
#46187 = DIRECTION ( 'NONE',  ( 0.000000000000000000, 1.000000000000000000, 0.000000000000000000 ) ) ;
#46188 = FACE_BOUND ( 'NONE', #71623, .T. ) ;
#46189 = ORIENTED_EDGE ( 'NONE', *, *, #23770, .T. ) ;
#46190 = CARTESIAN_POINT ( 'NONE',  ( 186.6927083336747160, 6.551208109652275624, -3.782341765624998686 ) ) ;
#46191 = CARTESIAN_POINT ( 'NONE',  ( 1.849999999999949685, 2.500000000000000000, 1.818653347947321475 ) ) ;
#46192 = DIRECTION ( 'NONE',  ( 0.000000000000000000, -0.9999939076577903929, 0.003490651415223739937 ) ) ;
#46193 = CIRCLE ( 'NONE', #119350, 0.09999999999999999167 ) ;
#46194 = DIRECTION ( 'NONE',  ( 0.000000000000000000, 0.000000000000000000, 1.000000000000000000 ) ) ;
#46195 = CARTESIAN_POINT ( 'NONE',  ( 9.549999999999915445, 2.500000000000000000, 6.495190528383297135 ) ) ;
#46196 = PLANE ( 'NONE',  #125978 ) ;
#46197 = DIRECTION ( 'NONE',  ( 0.000000000000000000, 0.000000000000000000, 1.000000000000000000 ) ) ;
#46198 = CARTESIAN_POINT ( 'NONE',  ( 175.5000000000000000, 0.000000000000000000, -2.000000000000000000 ) ) ;
#46199 = VECTOR ( 'NONE', #128918, 1000.000000000000000 ) ;
#46200 = CONICAL_SURFACE ( 'NONE', #6457, 0.1000000000000002554, 0.003490658503988666988 ) ;
#46201 = CARTESIAN_POINT ( 'NONE',  ( 2.099999999999950351, 2.500000000000000000, -0.6928203230275541413 ) ) ;
#46202 = ORIENTED_EDGE ( 'NONE', *, *, #91688, .T. ) ;
#46203 = ORIENTED_EDGE ( 'NONE', *, *, #126053, .F. ) ;
#46204 = ORIENTED_EDGE ( 'NONE', *, *, #21838, .T. ) ;
#46205 = ORIENTED_EDGE ( 'NONE', *, *, #56764, .T. ) ;
#46206 = ORIENTED_EDGE ( 'NONE', *, *, #27799, .T. ) ;
#46207 = CARTESIAN_POINT ( 'NONE',  ( -10.85000000000000142, 12.50000000000000000, -2.165063509461097713 ) ) ;
#46208 = CARTESIAN_POINT ( 'NONE',  ( -3.350000000000028955, 2.500000000000000000, 5.702370205355745014 ) ) ;
#46209 = ORIENTED_EDGE ( 'NONE', *, *, #42125, .T. ) ;
#46210 = FACE_BOUND ( 'NONE', #53982, .T. ) ;
#46211 = CONICAL_SURFACE ( 'NONE', #58741, 0.09999999999999982514, 0.003490658503988666988 ) ;
#46212 = DIRECTION ( 'NONE',  ( 0.000000000000000000, 0.000000000000000000, 1.000000000000000000 ) ) ;
#46213 = CIRCLE ( 'NONE', #48274, 0.1000000000000002554 ) ;
#46214 = EDGE_CURVE ( 'NONE', #22803, #74283, #91700, .T. ) ;
#46215 = DIRECTION ( 'NONE',  ( 0.000000000000000000, 0.000000000000000000, 1.000000000000000000 ) ) ;
#46216 = EDGE_CURVE ( 'NONE', #97917, #10224, #93760, .T. ) ;
#46217 = FACE_OUTER_BOUND ( 'NONE', #114396, .T. ) ;
#46218 = DIRECTION ( 'NONE',  ( 0.000000000000000000, 1.000000000000000000, 0.000000000000000000 ) ) ;
#46219 = DIRECTION ( 'NONE',  ( 0.000000000000000000, 0.000000000000000000, 1.000000000000000000 ) ) ;
#46220 = EDGE_LOOP ( 'NONE', ( #75777, #71559 ) ) ;
#46221 = DIRECTION ( 'NONE',  ( 0.000000000000000000, 0.000000000000000000, -1.000000000000000000 ) ) ;
#46222 = CIRCLE ( 'NONE', #62945, 0.06509327318403745899 ) ;
#46223 = VERTEX_POINT ( 'NONE', #126825 ) ;
#46224 = AXIS2_PLACEMENT_3D ( 'NONE', #20599, #31709, #60546 ) ;
#46225 = ORIENTED_EDGE ( 'NONE', *, *, #90938, .T. ) ;
#46226 = ORIENTED_EDGE ( 'NONE', *, *, #101290, .T. ) ;
#46227 = CARTESIAN_POINT ( 'NONE',  ( -5.650000000000023448, 12.50000000000000000, -1.818653347947326138 ) ) ;
#46228 = LINE ( 'NONE', #125437, #24642 ) ;
#46229 = CARTESIAN_POINT ( 'NONE',  ( 0.8499999999999553468, 12.50000000000000000, 1.537336459617582918 ) ) ;
#46230 = ORIENTED_EDGE ( 'NONE', *, *, #86460, .F. ) ;
#46231 = FACE_OUTER_BOUND ( 'NONE', #34633, .T. ) ;
#46232 = CIRCLE ( 'NONE', #108908, 0.06509327318403743123 ) ;
#46233 = CARTESIAN_POINT ( 'NONE',  ( 13.54999999999989946, 2.500000000000000000, 2.511473670974873507 ) ) ;
#46234 = DIRECTION ( 'NONE',  ( 0.000000000000000000, 0.000000000000000000, 1.000000000000000000 ) ) ;
#46235 = AXIS2_PLACEMENT_3D ( 'NONE', #101104, #21246, #51383 ) ;
#46236 = VECTOR ( 'NONE', #88779, 1000.000000000000000 ) ;
#46237 = CARTESIAN_POINT ( 'NONE',  ( 184.4479166673494603, -6.668395609140176816, -3.850000000000003642 ) ) ;
#46238 = DIRECTION ( 'NONE',  ( 0.000000000000000000, 0.000000000000000000, 1.000000000000000000 ) ) ;
#46239 = LINE ( 'NONE', #86144, #24448 ) ;
#46240 = VERTEX_POINT ( 'NONE', #76436 ) ;
#46241 = DIRECTION ( 'NONE',  ( -0.000000000000000000, -1.000000000000000000, -0.000000000000000000 ) ) ;
#46242 = ORIENTED_EDGE ( 'NONE', *, *, #78037, .T. ) ;
#46243 = VERTEX_POINT ( 'NONE', #6366 ) ;
#46244 = DIRECTION ( 'NONE',  ( -0.000000000000000000, -1.000000000000000000, -0.000000000000000000 ) ) ;
#46245 = FACE_OUTER_BOUND ( 'NONE', #47248, .T. ) ;
#46246 = FACE_OUTER_BOUND ( 'NONE', #83193, .T. ) ;
#46247 = ORIENTED_EDGE ( 'NONE', *, *, #16989, .F. ) ;
#46248 = ORIENTED_EDGE ( 'NONE', *, *, #112200, .F. ) ;
#46249 = EDGE_CURVE ( 'NONE', #64623, #41154, #102166, .T. ) ;
#46250 = DIRECTION ( 'NONE',  ( 0.000000000000000000, -0.000000000000000000, 1.000000000000000000 ) ) ;
#46251 = CARTESIAN_POINT ( 'NONE',  ( 32.26057503264689075, 3.190811010352110344, -3.146285318386026209 ) ) ;
#46252 = FACE_OUTER_BOUND ( 'NONE', #11965, .T. ) ;
#46253 = ORIENTED_EDGE ( 'NONE', *, *, #64591, .T. ) ;
#46254 = VERTEX_POINT ( 'NONE', #47622 ) ;
#46255 = VECTOR ( 'NONE', #24087, 1000.000000000000000 ) ;
#46256 = CIRCLE ( 'NONE', #69231, 0.06509327318403745899 ) ;
#46257 = CARTESIAN_POINT ( 'NONE',  ( 10.84999999999990905, 12.50000000000000000, 1.472243186433545459 ) ) ;
#46258 = ORIENTED_EDGE ( 'NONE', *, *, #83082, .F. ) ;
#46259 = CARTESIAN_POINT ( 'NONE',  ( 11.24999999999990585, 2.500000000000000000, -5.802370205355749988 ) ) ;
#46260 = CIRCLE ( 'NONE', #90155, 0.06509327318403745899 ) ;
#46261 = FACE_OUTER_BOUND ( 'NONE', #129426, .T. ) ;
#46262 = VERTEX_POINT ( 'NONE', #125525 ) ;
#46263 = DIRECTION ( 'NONE',  ( 0.000000000000000000, 0.000000000000000000, 1.000000000000000000 ) ) ;
#46264 = CONICAL_SURFACE ( 'NONE', #90157, 0.1000000000000002554, 0.003490658503988666988 ) ;
#46265 = CARTESIAN_POINT ( 'NONE',  ( -5.200000000000020606, 2.500000000000000000, 4.083716857408421497 ) ) ;
#46266 = DIRECTION ( 'NONE',  ( 0.000000000000000000, 0.000000000000000000, 1.000000000000000000 ) ) ;
#46268 = EDGE_CURVE ( 'NONE', #107707, #9138, #22765, .T. ) ;
#46267 = AXIS2_PLACEMENT_3D ( 'NONE', #15329, #36302, #66382 ) ;
#46269 = ADVANCED_FACE ( 'NONE', ( #15565 ), #110473, .T. ) ;
#46270 = LINE ( 'NONE', #127420, #102295 ) ;
#46271 = ORIENTED_EDGE ( 'NONE', *, *, #95989, .T. ) ;
#46272 = DIRECTION ( 'NONE',  ( -0.000000000000000000, 1.000000000000000000, -0.000000000000000000 ) ) ;
#46273 = CARTESIAN_POINT ( 'NONE',  ( 0.6499999999999566125, 2.500000000000000000, -6.841600689897077814 ) ) ;
#46274 = EDGE_LOOP ( 'NONE', ( #62452, #72455, #61629, #83609 ) ) ;
#46275 = ORIENTED_EDGE ( 'NONE', *, *, #50726, .T. ) ;
#46276 = ADVANCED_FACE ( 'NONE', ( #106529 ), #127218, .T. ) ;
#46277 = CARTESIAN_POINT ( 'NONE',  ( 185.9635416670080872, -4.367472073101519747, 7.564683531249999149 ) ) ;
#46278 = CARTESIAN_POINT ( 'NONE',  ( -6.250000000000021316, 2.500000000000000000, -1.472243186433550122 ) ) ;
#46279 = CARTESIAN_POINT ( 'NONE',  ( 2.499999999999983569, 2.500000000000000000, -0.1000000000000022815 ) ) ;
#46280 = DIRECTION ( 'NONE',  ( -0.000000000000000000, -1.000000000000000000, -0.000000000000000000 ) ) ;
#46281 = CARTESIAN_POINT ( 'NONE',  ( -6.650000000000018119, 2.500000000000000000, -2.957883832488653830 ) ) ;
#46282 = CARTESIAN_POINT ( 'NONE',  ( -1.650000000000035216, 12.50000000000000000, -5.802370205355749988 ) ) ;
#46283 = DIRECTION ( 'NONE',  ( -0.000000000000000000, 1.000000000000000000, -0.000000000000000000 ) ) ;
#46284 = DIRECTION ( 'NONE',  ( 0.000000000000000000, 0.000000000000000000, 1.000000000000000000 ) ) ;
#46285 = CARTESIAN_POINT ( 'NONE',  ( -10.80000000000000249, 12.50000000000000000, -4.330127018922197202 ) ) ;
#46286 = DIRECTION ( 'NONE',  ( -4.274815082592931898E-19, -0.9999939076577903929, -0.003490651415223739937 ) ) ;
#46287 = AXIS2_PLACEMENT_3D ( 'NONE', #124228, #105225, #94759 ) ;
#46288 = VERTEX_POINT ( 'NONE', #37796 ) ;
#46289 = CIRCLE ( 'NONE', #50497, 0.06509327318403745899 ) ;
#46290 = ORIENTED_EDGE ( 'NONE', *, *, #39421, .F. ) ;
#46291 = DIRECTION ( 'NONE',  ( -0.000000000000000000, 1.000000000000000000, -0.000000000000000000 ) ) ;
#46292 = ORIENTED_EDGE ( 'NONE', *, *, #88725, .T. ) ;
#46293 = FACE_OUTER_BOUND ( 'NONE', #53429, .T. ) ;
#46294 = CARTESIAN_POINT ( 'NONE',  ( 1.449999999999951772, 12.50000000000000000, -6.148780366869526226 ) ) ;
#46295 = DIRECTION ( 'NONE',  ( 0.000000000000000000, 0.000000000000000000, -1.000000000000000000 ) ) ;
#46296 = AXIS2_PLACEMENT_3D ( 'NONE', #35344, #126298, #115150 ) ;
#46297 = ORIENTED_EDGE ( 'NONE', *, *, #50622, .T. ) ;
#46298 = CARTESIAN_POINT ( 'NONE',  ( 18.70618316910015011, -2.558637580971261816, -2.503050677946357272 ) ) ;
#46299 = ADVANCED_FACE ( 'NONE', ( #87528 ), #31079, .T. ) ;
#46300 = CONICAL_SURFACE ( 'NONE', #50811, 0.1000000000000000472, 0.003490658503988666988 ) ;
#46301 = DIRECTION ( 'NONE',  ( 0.000000000000000000, 0.000000000000000000, -1.000000000000000000 ) ) ;
#46303 = VERTEX_POINT ( 'NONE', #86230 ) ;
#46302 = LINE ( 'NONE', #7010, #100352 ) ;
#46304 = EDGE_CURVE ( 'NONE', #56986, #32850, #14315, .T. ) ;
#46305 = EDGE_CURVE ( 'NONE', #73985, #22876, #7023, .T. ) ;
#46306 = DIRECTION ( 'NONE',  ( -0.000000000000000000, -1.000000000000000000, -0.000000000000000000 ) ) ;
#46307 = AXIS2_PLACEMENT_3D ( 'NONE', #86736, #87371, #78875 ) ;
#46308 = ORIENTED_EDGE ( 'NONE', *, *, #3190, .T. ) ;
#46309 = VECTOR ( 'NONE', #86750, 1000.000000000000000 ) ;
#46310 = ORIENTED_EDGE ( 'NONE', *, *, #492, .F. ) ;
#46311 = ORIENTED_EDGE ( 'NONE', *, *, #24902, .T. ) ;
#46312 = ORIENTED_EDGE ( 'NONE', *, *, #29726, .F. ) ;
#46313 = LINE ( 'NONE', #65299, #69608 ) ;
#46314 = EDGE_CURVE ( 'NONE', #6359, #21428, #56762, .T. ) ;
#46315 = EDGE_CURVE ( 'NONE', #125682, #93509, #37169, .T. ) ;
#46316 = EDGE_CURVE ( 'NONE', #125373, #21022, #24802, .T. ) ;
#46317 = CIRCLE ( 'NONE', #106950, 0.06509327318403745899 ) ;
#46318 = LINE ( 'NONE', #39113, #38158 ) ;
#46319 = DIRECTION ( 'NONE',  ( 0.000000000000000000, 0.000000000000000000, -1.000000000000000000 ) ) ;
#46320 = CARTESIAN_POINT ( 'NONE',  ( -6.450000000000019718, 12.50000000000000000, -6.148780366869526226 ) ) ;
#46321 = EDGE_LOOP ( 'NONE', ( #47683, #59283, #16409, #10780 ) ) ;
#46322 = ADVANCED_FACE ( 'NONE', ( #115700 ), #18535, .T. ) ;
#46323 = CIRCLE ( 'NONE', #67136, 0.1000000000000002554 ) ;
#46324 = CIRCLE ( 'NONE', #125725, 0.06509327318403741736 ) ;
#46325 = DIRECTION ( 'NONE',  ( 0.000000000000000000, 0.000000000000000000, 1.000000000000000000 ) ) ;
#46326 = ORIENTED_EDGE ( 'NONE', *, *, #61733, .F. ) ;
#46327 = FACE_OUTER_BOUND ( 'NONE', #99075, .T. ) ;
#46328 = CARTESIAN_POINT ( 'NONE',  ( 16.56576425165006228, -2.499999999999998668, -6.084390597445814564 ) ) ;
#46329 = DIRECTION ( 'NONE',  ( -0.000000000000000000, -1.000000000000000000, -0.000000000000000000 ) ) ;
#46330 = CARTESIAN_POINT ( 'NONE',  ( 18.09676523922663449, -2.526776815559105938, 2.684906793687434234 ) ) ;
#46331 = EDGE_CURVE ( 'NONE', #74045, #110749, #74972, .T. ) ;
#46332 = EDGE_LOOP ( 'NONE', ( #73673, #58081 ) ) ;
#46333 = ORIENTED_EDGE ( 'NONE', *, *, #12475, .F. ) ;
#46334 = ORIENTED_EDGE ( 'NONE', *, *, #13941, .F. ) ;
#46335 = DIRECTION ( 'NONE',  ( 0.000000000000000000, 0.000000000000000000, -1.000000000000000000 ) ) ;
#46336 = DIRECTION ( 'NONE',  ( -4.274815082592931898E-19, -0.9999939076577903929, -0.003490651415223739937 ) ) ;
#46337 = DIRECTION ( 'NONE',  ( 0.000000000000000000, 0.000000000000000000, 1.000000000000000000 ) ) ;
#46338 = FACE_BOUND ( 'NONE', #27060, .T. ) ;
#46339 = DIRECTION ( 'NONE',  ( -0.000000000000000000, -1.000000000000000000, -0.000000000000000000 ) ) ;
#46340 = DIRECTION ( 'NONE',  ( -0.000000000000000000, -1.000000000000000000, -0.000000000000000000 ) ) ;
#46341 = DIRECTION ( 'NONE',  ( 0.000000000000000000, -0.000000000000000000, 1.000000000000000000 ) ) ;
#46342 = CIRCLE ( 'NONE', #6603, 0.06509327318403745899 ) ;
#46343 = AXIS2_PLACEMENT_3D ( 'NONE', #8929, #58695, #109732 ) ;
#46345 = AXIS2_PLACEMENT_3D ( 'NONE', #50003, #212, #40167 ) ;
#46344 = CARTESIAN_POINT ( 'NONE',  ( 185.9218750003414016, 0.000000000000000000, 7.564683531250000925 ) ) ;
#46346 = FACE_OUTER_BOUND ( 'NONE', #52003, .T. ) ;
#46347 = DIRECTION ( 'NONE',  ( 0.000000000000000000, 1.000000000000000000, 0.000000000000000000 ) ) ;
#46348 = FACE_OUTER_BOUND ( 'NONE', #108727, .T. ) ;
#46349 = ORIENTED_EDGE ( 'NONE', *, *, #15719, .F. ) ;
#46350 = VERTEX_POINT ( 'NONE', #27976 ) ;
#46351 = EDGE_LOOP ( 'NONE', ( #76782, #94096 ) ) ;
#46352 = ORIENTED_EDGE ( 'NONE', *, *, #96176, .T. ) ;
#46353 = CONICAL_SURFACE ( 'NONE', #15030, 0.09999999999999982514, 0.003490658503988666988 ) ;
#46354 = CONICAL_SURFACE ( 'NONE', #23363, 0.1000000000000002554, 0.003490658503988666988 ) ;
#46355 = DIRECTION ( 'NONE',  ( 0.000000000000000000, 0.000000000000000000, -1.000000000000000000 ) ) ;
#46356 = FACE_BOUND ( 'NONE', #51831, .T. ) ;
#46357 = CARTESIAN_POINT ( 'NONE',  ( 107.5000000000000142, -1.500000000000000222, -1.322875655532295136 ) ) ;
#46358 = AXIS2_PLACEMENT_3D ( 'NONE', #77588, #117494, #38342 ) ;
#46359 = CARTESIAN_POINT ( 'NONE',  ( -9.400000000000009237, 12.50000000000000000, -4.676537180435974328 ) ) ;
#46360 = ADVANCED_FACE ( 'NONE', ( #25380 ), #95998, .T. ) ;
#46361 = ORIENTED_EDGE ( 'NONE', *, *, #27799, .F. ) ;
#46362 = CARTESIAN_POINT ( 'NONE',  ( -5.850000000000018296, 2.500000000000000000, 2.757883832488649656 ) ) ;
#46363 = DIRECTION ( 'NONE',  ( -0.000000000000000000, -1.000000000000000000, -0.000000000000000000 ) ) ;
#46364 = ORIENTED_EDGE ( 'NONE', *, *, #6548, .T. ) ;
#46365 = DIRECTION ( 'NONE',  ( 0.000000000000000000, 1.000000000000000000, 0.000000000000000000 ) ) ;
#46366 = DIRECTION ( 'NONE',  ( -0.000000000000000000, -1.000000000000000000, -0.000000000000000000 ) ) ;
#46367 = ADVANCED_FACE ( 'NONE', ( #120230 ), #22859, .T. ) ;
#46368 = VERTEX_POINT ( 'NONE', #41687 ) ;
#46369 = DIRECTION ( 'NONE',  ( -0.000000000000000000, 1.000000000000000000, -0.000000000000000000 ) ) ;
#46370 = CARTESIAN_POINT ( 'NONE',  ( -9.999999999999971578, 2.500000000000000000, -4.430127018922197735 ) ) ;
#46371 = CIRCLE ( 'NONE', #6636, 0.06509327318403745899 ) ;
#46372 = AXIS2_PLACEMENT_3D ( 'NONE', #109389, #20375, #18436 ) ;
#46373 = VERTEX_POINT ( 'NONE', #58730 ) ;
#46374 = CARTESIAN_POINT ( 'NONE',  ( -9.600000000000006750, 2.500000000000000000, 5.122947341949749323 ) ) ;
#46375 = FACE_OUTER_BOUND ( 'NONE', #73775, .T. ) ;
#46376 = ORIENTED_EDGE ( 'NONE', *, *, #8312, .F. ) ;
#46377 = CARTESIAN_POINT ( 'NONE',  ( -1.250000000000036193, 2.500000000000000000, 1.472243186433545459 ) ) ;
#46378 = ORIENTED_EDGE ( 'NONE', *, *, #81961, .T. ) ;
#46379 = VERTEX_POINT ( 'NONE', #80953 ) ;
#46380 = DIRECTION ( 'NONE',  ( 0.000000000000000000, 0.000000000000000000, -1.000000000000000000 ) ) ;
#46381 = CIRCLE ( 'NONE', #6646, 0.09999999999999982514 ) ;
#46382 = VERTEX_POINT ( 'NONE', #50210 ) ;
#46383 = CARTESIAN_POINT ( 'NONE',  ( -2.300000000000033573, 2.500000000000000000, -3.883716857408426648 ) ) ;
#46384 = CIRCLE ( 'NONE', #111308, 0.1000000000000000472 ) ;
#46385 = CARTESIAN_POINT ( 'NONE',  ( -10.65000000000000391, 12.50000000000000000, -1.818653347947322141 ) ) ;
#46386 = AXIS2_PLACEMENT_3D ( 'NONE', #43421, #123251, #72229 ) ;
#46387 = ORIENTED_EDGE ( 'NONE', *, *, #12606, .T. ) ;
#46388 = VECTOR ( 'NONE', #112956, 1000.000000000000000 ) ;
#46389 = CARTESIAN_POINT ( 'NONE',  ( -5.400000000000024336, 2.500000000000000000, -3.737306695894649700 ) ) ;
#46390 = DIRECTION ( 'NONE',  ( 0.000000000000000000, 1.000000000000000000, 0.000000000000000000 ) ) ;
#46391 = FACE_OUTER_BOUND ( 'NONE', #58532, .T. ) ;
#46392 = PLANE ( 'NONE',  #46597 ) ;
#46393 = DIRECTION ( 'NONE',  ( -0.000000000000000000, 1.000000000000000000, -0.000000000000000000 ) ) ;
#46394 = FACE_OUTER_BOUND ( 'NONE', #78387, .T. ) ;
#46395 = VECTOR ( 'NONE', #26534, 1000.000000000000000 ) ;
#46396 = VERTEX_POINT ( 'NONE', #101230 ) ;
#46397 = AXIS2_PLACEMENT_3D ( 'NONE', #113478, #124602, #23822 ) ;
#46399 = ORIENTED_EDGE ( 'NONE', *, *, #86939, .F. ) ;
#46398 = EDGE_CURVE ( 'NONE', #99722, #84166, #83492, .T. ) ;
#46400 = DIRECTION ( 'NONE',  ( 0.000000000000000000, 0.000000000000000000, 1.000000000000000000 ) ) ;
#46402 = CONICAL_SURFACE ( 'NONE', #12946, 0.1000000000000000472, 0.003490658503988666988 ) ;
#46401 = CARTESIAN_POINT ( 'NONE',  ( -11.64999999999999680, 12.50000000000000000, 6.495190528383297135 ) ) ;
#46403 = AXIS2_PLACEMENT_3D ( 'NONE', #115298, #75393, #94391 ) ;
#46404 = LINE ( 'NONE', #54939, #43862 ) ;
#46406 = ORIENTED_EDGE ( 'NONE', *, *, #111123, .T. ) ;
#46405 = ORIENTED_EDGE ( 'NONE', *, *, #117260, .F. ) ;
#46407 = ORIENTED_EDGE ( 'NONE', *, *, #28119, .F. ) ;
#46408 = CARTESIAN_POINT ( 'NONE',  ( 5.199999999999935341, 12.50000000000000000, -3.918623584224389056 ) ) ;
#46409 = CIRCLE ( 'NONE', #115444, 0.06509327318403745899 ) ;
#46411 = EDGE_CURVE ( 'NONE', #37483, #91091, #93845, .T. ) ;
#46410 = CARTESIAN_POINT ( 'NONE',  ( -1.650000000000034772, 2.500000000000000000, 1.372243186433545370 ) ) ;
#46412 = DIRECTION ( 'NONE',  ( -4.274815082592931898E-19, -0.9999939076577903929, -0.003490651415223739937 ) ) ;
#46413 = CARTESIAN_POINT ( 'NONE',  ( 0.000000000000000000, 0.000000000000000000, 0.000000000000000000 ) ) ;
#46414 = FACE_OUTER_BOUND ( 'NONE', #93450, .T. ) ;
#46415 = AXIS2_PLACEMENT_3D ( 'NONE', #24322, #55707, #15776 ) ;
#46416 = DIRECTION ( 'NONE',  ( 0.000000000000000000, -0.000000000000000000, 1.000000000000000000 ) ) ;
#46417 = FACE_OUTER_BOUND ( 'NONE', #14872, .T. ) ;
#46418 = DIRECTION ( 'NONE',  ( 0.000000000000000000, 0.000000000000000000, -1.000000000000000000 ) ) ;
#46419 = CARTESIAN_POINT ( 'NONE',  ( -12.89999999999999147, 12.50000000000000000, 3.637306695894644726 ) ) ;
#46420 = EDGE_CURVE ( 'NONE', #80777, #117628, #27041, .T. ) ;
#46421 = EDGE_CURVE ( 'NONE', #100844, #88410, #58047, .T. ) ;
#46422 = CARTESIAN_POINT ( 'NONE',  ( -5.850000000000022737, 12.50000000000000000, -6.495190528383302464 ) ) ;
#46423 = ORIENTED_EDGE ( 'NONE', *, *, #7166, .T. ) ;
#46424 = EDGE_CURVE ( 'NONE', #79959, #68225, #79289, .T. ) ;
#46425 = FACE_OUTER_BOUND ( 'NONE', #37982, .T. ) ;
#46426 = VERTEX_POINT ( 'NONE', #428 ) ;
#46427 = VERTEX_POINT ( 'NONE', #10885 ) ;
#46428 = EDGE_CURVE ( 'NONE', #7354, #79666, #9623, .T. ) ;
#46429 = DIRECTION ( 'NONE',  ( -0.000000000000000000, 1.000000000000000000, -0.000000000000000000 ) ) ;
#46430 = CARTESIAN_POINT ( 'NONE',  ( 2.049999999999950084, 12.50000000000000000, -2.165063509461101710 ) ) ;
#46431 = DIRECTION ( 'NONE',  ( 0.000000000000000000, 1.000000000000000000, 0.000000000000000000 ) ) ;
#46432 = CARTESIAN_POINT ( 'NONE',  ( 6.649999999999928413, 12.50000000000000000, 1.472243186433545459 ) ) ;
#46433 = CARTESIAN_POINT ( 'NONE',  ( -4.800000000000022915, 2.500000000000000000, -0.3464101615137783474 ) ) ;
#46434 = CARTESIAN_POINT ( 'NONE',  ( -0.2000000000000412836, 2.500000000000000000, 4.576537180435972019 ) ) ;
#46435 = CARTESIAN_POINT ( 'NONE',  ( 5.399999999999931966, 12.50000000000000000, 4.330127018922196314 ) ) ;
#46436 = EDGE_LOOP ( 'NONE', ( #5426, #49491 ) ) ;
#46437 = DIRECTION ( 'NONE',  ( 0.000000000000000000, 0.000000000000000000, -1.000000000000000000 ) ) ;
#46438 = AXIS2_PLACEMENT_3D ( 'NONE', #106843, #57771, #28306 ) ;
#46439 = CIRCLE ( 'NONE', #35990, 0.1000000000000000472 ) ;
#46440 = DIRECTION ( 'NONE',  ( 0.000000000000000000, 0.000000000000000000, -1.000000000000000000 ) ) ;
#46441 = ORIENTED_EDGE ( 'NONE', *, *, #66844, .T. ) ;
#46442 = EDGE_LOOP ( 'NONE', ( #37832, #34206, #83731, #75654 ) ) ;
#46443 = VECTOR ( 'NONE', #25516, 1000.000000000000000 ) ;
#46444 = CIRCLE ( 'NONE', #117525, 0.06509327318403745899 ) ;
#46445 = ORIENTED_EDGE ( 'NONE', *, *, #31848, .F. ) ;
#46446 = AXIS2_PLACEMENT_3D ( 'NONE', #14668, #46089, #85983 ) ;
#46447 = AXIS2_PLACEMENT_3D ( 'NONE', #36624, #35961, #16293 ) ;
#46448 = ORIENTED_EDGE ( 'NONE', *, *, #82356, .T. ) ;
#46449 = LINE ( 'NONE', #87023, #4406 ) ;
#46450 = DIRECTION ( 'NONE',  ( -0.000000000000000000, -1.000000000000000000, -0.000000000000000000 ) ) ;
#46451 = AXIS2_PLACEMENT_3D ( 'NONE', #56099, #96657, #25344 ) ;
#46452 = ORIENTED_EDGE ( 'NONE', *, *, #32292, .T. ) ;
#46453 = CARTESIAN_POINT ( 'NONE',  ( 129.5000000000000000, -1.375000000000000222, 6.000000000000000000 ) ) ;
#46454 = CARTESIAN_POINT ( 'NONE',  ( -1.650000000000034772, 2.500000000000000000, 5.702370205355745014 ) ) ;
#46455 = CARTESIAN_POINT ( 'NONE',  ( 2.299999999999947864, 2.500000000000000000, 4.083716857408421497 ) ) ;
#46456 = VERTEX_POINT ( 'NONE', #31215 ) ;
#46457 = DIRECTION ( 'NONE',  ( -0.000000000000000000, 1.000000000000000000, -0.000000000000000000 ) ) ;
#46458 = EDGE_CURVE ( 'NONE', #9494, #79598, #43787, .T. ) ;
#46459 = DIRECTION ( 'NONE',  ( 0.000000000000000000, 0.000000000000000000, -1.000000000000000000 ) ) ;
#46460 = VERTEX_POINT ( 'NONE', #99944 ) ;
#46461 = ORIENTED_EDGE ( 'NONE', *, *, #124796, .F. ) ;
#46462 = VERTEX_POINT ( 'NONE', #61312 ) ;
#46463 = EDGE_CURVE ( 'NONE', #53157, #81003, #91404, .T. ) ;
#46464 = CARTESIAN_POINT ( 'NONE',  ( 2.099999999999950351, 2.500000000000000000, -5.022947341949754119 ) ) ;
#46465 = ADVANCED_FACE ( 'NONE', ( #20737 ), #39756, .T. ) ;
#46466 = ADVANCED_FACE ( 'NONE', ( #90097 ), #50843, .F. ) ;
#46467 = EDGE_CURVE ( 'NONE', #89242, #81079, #20785, .T. ) ;
#46468 = CIRCLE ( 'NONE', #119626, 0.09999999999999999167 ) ;
#46469 = DIRECTION ( 'NONE',  ( 0.000000000000000000, 1.000000000000000000, 0.000000000000000000 ) ) ;
#46470 = EDGE_CURVE ( 'NONE', #122261, #29766, #48921, .T. ) ;
#46471 = EDGE_LOOP ( 'NONE', ( #100029, #26189 ) ) ;
#46472 = FACE_OUTER_BOUND ( 'NONE', #83037, .T. ) ;
#46473 = CARTESIAN_POINT ( 'NONE',  ( 149.5981739382431783, 0.5000000000000000000, 1.703575533167231537 ) ) ;
#46474 = DIRECTION ( 'NONE',  ( -0.000000000000000000, 1.000000000000000000, -0.000000000000000000 ) ) ;
#46475 = CARTESIAN_POINT ( 'NONE',  ( -11.05000000000000249, 2.500000000000000000, -1.918653347947322230 ) ) ;
#46476 = CONICAL_SURFACE ( 'NONE', #54889, 0.1000000000000002554, 0.003490658503988666988 ) ;
#46477 = EDGE_CURVE ( 'NONE', #57283, #101787, #118977, .T. ) ;
#46478 = CIRCLE ( 'NONE', #6747, 0.09999999999999982514 ) ;
#46479 = EDGE_LOOP ( 'NONE', ( #97751, #46184 ) ) ;
#46480 = EDGE_CURVE ( 'NONE', #119348, #93899, #91792, .T. ) ;
#46481 = CARTESIAN_POINT ( 'NONE',  ( -5.850000000000021849, 12.50000000000000000, -7.122917578226816815 ) ) ;
#46482 = CIRCLE ( 'NONE', #71620, 0.1000000000000002554 ) ;
#46483 = EDGE_LOOP ( 'NONE', ( #25652, #88328 ) ) ;
#46484 = ORIENTED_EDGE ( 'NONE', *, *, #51003, .T. ) ;
#46485 = ORIENTED_EDGE ( 'NONE', *, *, #45020, .F. ) ;
#46486 = DIRECTION ( 'NONE',  ( 0.000000000000000000, 0.000000000000000000, 1.000000000000000000 ) ) ;
#46487 = FACE_BOUND ( 'NONE', #93901, .T. ) ;
#46488 = DIRECTION ( 'NONE',  ( 0.000000000000000000, 0.000000000000000000, 1.000000000000000000 ) ) ;
#46490 = CIRCLE ( 'NONE', #73584, 2.750000000000002665 ) ;
#46489 = DIRECTION ( 'NONE',  ( 0.000000000000000000, 0.000000000000000000, 1.000000000000000000 ) ) ;
#46492 = CARTESIAN_POINT ( 'NONE',  ( 1.249999999999988454, 2.500000000000000000, -2.065063509461102065 ) ) ;
#46491 = CIRCLE ( 'NONE', #119653, 0.06509327318403745899 ) ;
#46493 = AXIS2_PLACEMENT_3D ( 'NONE', #55736, #105492, #96292 ) ;
#46494 = ORIENTED_EDGE ( 'NONE', *, *, #104388, .T. ) ;
#46495 = CARTESIAN_POINT ( 'NONE',  ( -4.350000000000027178, 2.500000000000000000, -6.248780366869526759 ) ) ;
#46496 = CYLINDRICAL_SURFACE ( 'NONE', #128338, 2.000000000000000000 ) ;
#46497 = PLANE ( 'NONE',  #103005 ) ;
#46498 = AXIS2_PLACEMENT_3D ( 'NONE', #32707, #2550, #32058 ) ;
#46499 = CARTESIAN_POINT ( 'NONE',  ( -13.09999999999999076, 2.500000000000000000, 3.883716857408421319 ) ) ;
#46500 = VERTEX_POINT ( 'NONE', #29277 ) ;
#46501 = DIRECTION ( 'NONE',  ( 0.000000000000000000, 0.000000000000000000, 1.000000000000000000 ) ) ;
#46502 = CARTESIAN_POINT ( 'NONE',  ( 5.449999999999936229, 12.50000000000000000, 6.495190528383297135 ) ) ;
#46503 = AXIS2_PLACEMENT_3D ( 'NONE', #71318, #32075, #11106 ) ;
#46504 = EDGE_LOOP ( 'NONE', ( #112644, #72924, #98525, #104476 ) ) ;
#46505 = FACE_OUTER_BOUND ( 'NONE', #40271, .T. ) ;
#46506 = DIRECTION ( 'NONE',  ( 0.000000000000000000, 0.000000000000000000, 1.000000000000000000 ) ) ;
#46507 = FACE_BOUND ( 'NONE', #122716, .T. ) ;
#46508 = DIRECTION ( 'NONE',  ( -0.000000000000000000, -1.000000000000000000, -0.000000000000000000 ) ) ;
#46509 = ORIENTED_EDGE ( 'NONE', *, *, #73045, .F. ) ;
#46510 = DIRECTION ( 'NONE',  ( 0.000000000000000000, 0.000000000000000000, 1.000000000000000000 ) ) ;
#46511 = CARTESIAN_POINT ( 'NONE',  ( -15.19999999999998330, 2.500000000000000000, 0.3464101615137758494 ) ) ;
#46512 = ORIENTED_EDGE ( 'NONE', *, *, #62405, .T. ) ;
#46513 = ORIENTED_EDGE ( 'NONE', *, *, #41790, .T. ) ;
#46514 = CONICAL_SURFACE ( 'NONE', #53081, 0.09999999999999999167, 0.003490658503988666988 ) ;
#46515 = CARTESIAN_POINT ( 'NONE',  ( 186.0416666666666856, -4.445597072760122614, 7.699999999999998401 ) ) ;
#46516 = ORIENTED_EDGE ( 'NONE', *, *, #46162, .F. ) ;
#46517 = CARTESIAN_POINT ( 'NONE',  ( 186.1718750003414016, 9.264065473108010111E-16, -7.564683531250000925 ) ) ;
#46518 = DIRECTION ( 'NONE',  ( 0.000000000000000000, 0.000000000000000000, 1.000000000000000000 ) ) ;
#46519 = EDGE_CURVE ( 'NONE', #83167, #98725, #58361, .T. ) ;
#46520 = AXIS2_PLACEMENT_3D ( 'NONE', #19969, #70351, #100455 ) ;
#46521 = CARTESIAN_POINT ( 'NONE',  ( -3.749999999999994671, 12.50000000000000000, -6.430097255199264339 ) ) ;
#46522 = AXIS2_PLACEMENT_3D ( 'NONE', #72013, #111929, #43205 ) ;
#46523 = AXIS2_PLACEMENT_3D ( 'NONE', #73641, #92652, #71723 ) ;
#46524 = FACE_OUTER_BOUND ( 'NONE', #44098, .T. ) ;
#46526 = EDGE_LOOP ( 'NONE', ( #127718, #14052 ) ) ;
#46525 = CONICAL_SURFACE ( 'NONE', #119694, 0.1000000000000000472, 0.003490658503988666988 ) ;
#46527 = AXIS2_PLACEMENT_3D ( 'NONE', #45515, #76894, #55954 ) ;
#46528 = LINE ( 'NONE', #126395, #98793 ) ;
#46529 = DIRECTION ( 'NONE',  ( -0.000000000000000000, -1.000000000000000000, -0.000000000000000000 ) ) ;
#46530 = FACE_OUTER_BOUND ( 'NONE', #2244, .T. ) ;
#46531 = AXIS2_PLACEMENT_3D ( 'NONE', #27389, #107257, #122566 ) ;
#46532 = DIRECTION ( 'NONE',  ( 0.000000000000000000, 0.000000000000000000, -1.000000000000000000 ) ) ;
#46534 = VERTEX_POINT ( 'NONE', #71773 ) ;
#46533 = AXIS2_PLACEMENT_3D ( 'NONE', #50705, #70348, #19964 ) ;
#46535 = CARTESIAN_POINT ( 'NONE',  ( 0.8499999999999545697, 12.50000000000000000, -1.472243186433550122 ) ) ;
#46536 = ORIENTED_EDGE ( 'NONE', *, *, #47795, .F. ) ;
#46537 = CARTESIAN_POINT ( 'NONE',  ( 6.649999999999931966, 2.500000000000000000, -7.288010851410854585 ) ) ;
#46538 = DIRECTION ( 'NONE',  ( 0.000000000000000000, 0.000000000000000000, -1.000000000000000000 ) ) ;
#46539 = AXIS2_PLACEMENT_3D ( 'NONE', #42951, #90727, #61928 ) ;
#46540 = ORIENTED_EDGE ( 'NONE', *, *, #12480, .T. ) ;
#46541 = FACE_OUTER_BOUND ( 'NONE', #41533, .T. ) ;
#46542 = CARTESIAN_POINT ( 'NONE',  ( 17.50000000000000000, -2.500000000000000000, -3.999999999999998224 ) ) ;
#46543 = FACE_OUTER_BOUND ( 'NONE', #118945, .T. ) ;
#46544 = CARTESIAN_POINT ( 'NONE',  ( -14.14999999999998614, 2.500000000000000000, -2.265063509461099578 ) ) ;
#46545 = EDGE_LOOP ( 'NONE', ( #44973, #33600, #85088, #8825 ) ) ;
#46546 = LINE ( 'NONE', #66191, #108021 ) ;
#46547 = DIRECTION ( 'NONE',  ( 0.000000000000000000, -0.9999939076577903929, 0.003490651415223739937 ) ) ;
#46548 = CARTESIAN_POINT ( 'NONE',  ( 186.4427083336747160, -6.551208109652278289, 3.782341765624995134 ) ) ;
#46549 = DIRECTION ( 'NONE',  ( 0.000000000000000000, 0.000000000000000000, -1.000000000000000000 ) ) ;
#46550 = CARTESIAN_POINT ( 'NONE',  ( 1.849999999999948130, 2.500000000000000000, 6.248780366869520542 ) ) ;
#46551 = AXIS2_PLACEMENT_3D ( 'NONE', #72274, #34288, #102371 ) ;
#46552 = ORIENTED_EDGE ( 'NONE', *, *, #3488, .T. ) ;
#46553 = EDGE_LOOP ( 'NONE', ( #73077, #88107, #10134, #42803 ) ) ;
#46554 = DIRECTION ( 'NONE',  ( 0.000000000000000000, 1.000000000000000000, 0.000000000000000000 ) ) ;
#46555 = ORIENTED_EDGE ( 'NONE', *, *, #21176, .T. ) ;
#46556 = FACE_OUTER_BOUND ( 'NONE', #56251, .T. ) ;
#46558 = VERTEX_POINT ( 'NONE', #73061 ) ;
#46557 = EDGE_LOOP ( 'NONE', ( #50802, #105717 ) ) ;
#46559 = VERTEX_POINT ( 'NONE', #14118 ) ;
#46560 = DIRECTION ( 'NONE',  ( 0.000000000000000000, 1.000000000000000000, 0.000000000000000000 ) ) ;
#46561 = AXIS2_PLACEMENT_3D ( 'NONE', #83974, #72256, #31671 ) ;
#46562 = AXIS2_PLACEMENT_3D ( 'NONE', #84829, #56640, #104470 ) ;
#46564 = ADVANCED_FACE ( 'NONE', ( #14746 ), #14409, .T. ) ;
#46563 = DIRECTION ( 'NONE',  ( 0.000000000000000000, 0.000000000000000000, 1.000000000000000000 ) ) ;
#46565 = AXIS2_PLACEMENT_3D ( 'NONE', #64244, #104173, #74071 ) ;
#46566 = CARTESIAN_POINT ( 'NONE',  ( -9.800000000000006040, 12.50000000000000000, 0.3464101615137735735 ) ) ;
#46567 =( NAMED_UNIT ( * ) SI_UNIT ( $, .STERADIAN. ) SOLID_ANGLE_UNIT ( ) );
#46568 = DIRECTION ( 'NONE',  ( -0.000000000000000000, -1.000000000000000000, -0.000000000000000000 ) ) ;
#46569 = CARTESIAN_POINT ( 'NONE',  ( -11.25000000000000178, 12.50000000000000000, -1.472243186433546125 ) ) ;
#46570 = CARTESIAN_POINT ( 'NONE',  ( -10.84999999999999964, 12.50000000000000000, 7.188010851410848723 ) ) ;
#46571 = EDGE_CURVE ( 'NONE', #118622, #50743, #45829, .T. ) ;
#46572 = ORIENTED_EDGE ( 'NONE', *, *, #81631, .F. ) ;
#46573 = CIRCLE ( 'NONE', #4791, 0.06509327318403745899 ) ;
#46574 = EDGE_CURVE ( 'NONE', #23743, #46243, #18627, .T. ) ;
#46575 = CIRCLE ( 'NONE', #84224, 0.09999999999999982514 ) ;
#46576 = CARTESIAN_POINT ( 'NONE',  ( 1.449999999999952660, 2.500000000000000000, -6.941600689897078347 ) ) ;
#46577 = ORIENTED_EDGE ( 'NONE', *, *, #46420, .F. ) ;
#46578 = AXIS2_PLACEMENT_3D ( 'NONE', #60272, #100790, #78616 ) ;
#46579 = ORIENTED_EDGE ( 'NONE', *, *, #43207, .T. ) ;
#46580 = ORIENTED_EDGE ( 'NONE', *, *, #39097, .F. ) ;
#46581 = ORIENTED_EDGE ( 'NONE', *, *, #35533, .T. ) ;
#46582 = EDGE_CURVE ( 'NONE', #58440, #15244, #110567, .T. ) ;
#46584 = EDGE_CURVE ( 'NONE', #54447, #37927, #22041, .T. ) ;
#46583 = DIRECTION ( 'NONE',  ( -0.000000000000000000, 1.000000000000000000, -0.000000000000000000 ) ) ;
#46586 = VERTEX_POINT ( 'NONE', #61957 ) ;
#46585 = EDGE_CURVE ( 'NONE', #29513, #17807, #1898, .T. ) ;
#46587 = ORIENTED_EDGE ( 'NONE', *, *, #48374, .F. ) ;
#46588 = EDGE_CURVE ( 'NONE', #128722, #15804, #63882, .T. ) ;
#46589 = AXIS2_PLACEMENT_3D ( 'NONE', #90271, #68712, #614 ) ;
#46590 = AXIS2_PLACEMENT_3D ( 'NONE', #48458, #57642, #17019 ) ;
#46591 = DIRECTION ( 'NONE',  ( -0.000000000000000000, -1.000000000000000000, -0.000000000000000000 ) ) ;
#46592 = DIRECTION ( 'NONE',  ( -0.000000000000000000, -1.000000000000000000, -0.000000000000000000 ) ) ;
#46593 = DIRECTION ( 'NONE',  ( 0.000000000000000000, 0.000000000000000000, 1.000000000000000000 ) ) ;
#46594 = CONICAL_SURFACE ( 'NONE', #67502, 0.09999999999999982514, 0.003490658503988666988 ) ;
#46595 = DIRECTION ( 'NONE',  ( 0.000000000000000000, 1.000000000000000000, 0.000000000000000000 ) ) ;
#46596 = AXIS2_PLACEMENT_3D ( 'NONE', #16307, #57553, #58212 ) ;
#46597 = AXIS2_PLACEMENT_3D ( 'NONE', #34678, #93579, #15637 ) ;
#46598 = DIRECTION ( 'NONE',  ( 0.000000000000000000, 1.000000000000000000, 0.000000000000000000 ) ) ;
#46599 = EDGE_LOOP ( 'NONE', ( #52206, #31345 ) ) ;
#46600 = EDGE_CURVE ( 'NONE', #26024, #9406, #10315, .T. ) ;
#46601 = CIRCLE ( 'NONE', #23617, 0.06509327318403745899 ) ;
#46602 = DIRECTION ( 'NONE',  ( 0.000000000000000000, 0.000000000000000000, -1.000000000000000000 ) ) ;
#46603 = VERTEX_POINT ( 'NONE', #42315 ) ;
#46604 = CARTESIAN_POINT ( 'NONE',  ( 3.949999999999941558, 12.50000000000000000, -6.148780366869526226 ) ) ;
#46605 = VERTEX_POINT ( 'NONE', #104446 ) ;
#46606 = CIRCLE ( 'NONE', #119765, 0.1000000000000002554 ) ;
#46607 = CARTESIAN_POINT ( 'NONE',  ( -12.29999999999999716, 2.500000000000000000, 0.3464101615137776813 ) ) ;
#46608 = ORIENTED_EDGE ( 'NONE', *, *, #52310, .F. ) ;
#46609 = EDGE_LOOP ( 'NONE', ( #75438, #42350 ) ) ;
#46610 = CARTESIAN_POINT ( 'NONE',  ( 1.249999999999952038, 12.50000000000000000, -1.472243186433550122 ) ) ;
#46611 = CARTESIAN_POINT ( 'NONE',  ( -9.800000000000004263, 2.500000000000000000, -0.3464101615137783474 ) ) ;
#46612 = DIRECTION ( 'NONE',  ( 0.000000000000000000, 0.000000000000000000, 1.000000000000000000 ) ) ;
#46613 = FACE_OUTER_BOUND ( 'NONE', #91122, .T. ) ;
#46614 = CARTESIAN_POINT ( 'NONE',  ( -13.29999999999999005, 2.500000000000000000, -0.09999999999999815981 ) ) ;
#46615 = EDGE_LOOP ( 'NONE', ( #57648, #12222, #47626, #111983 ) ) ;
#46616 = CARTESIAN_POINT ( 'NONE',  ( -9.800000000000004263, 12.50000000000000000, 4.048810130592458201 ) ) ;
#46618 = VECTOR ( 'NONE', #43873, 1000.000000000000000 ) ;
#46617 = FACE_OUTER_BOUND ( 'NONE', #60770, .T. ) ;
#46619 = EDGE_CURVE ( 'NONE', #117732, #113146, #68807, .T. ) ;
#46620 = CARTESIAN_POINT ( 'NONE',  ( 1.449999999999951328, 12.50000000000000000, 2.511473670974873507 ) ) ;
#46621 = CARTESIAN_POINT ( 'NONE',  ( -7.900000000000014566, 12.50000000000000000, -0.6928203230275541413 ) ) ;
#46622 = CARTESIAN_POINT ( 'NONE',  ( -8.550000000000011369, 2.500000000000000000, 1.818653347947321475 ) ) ;
#46623 = ORIENTED_EDGE ( 'NONE', *, *, #106834, .T. ) ;
#46624 = AXIS2_PLACEMENT_3D ( 'NONE', #35864, #6363, #14893 ) ;
#46625 = CONICAL_SURFACE ( 'NONE', #57086, 0.09999999999999999167, 0.003490658503988666988 ) ;
#46626 = ORIENTED_EDGE ( 'NONE', *, *, #108512, .T. ) ;
#46627 = VECTOR ( 'NONE', #115786, 1000.000000000000000 ) ;
#46629 = ADVANCED_FACE ( 'NONE', ( #52136 ), #112729, .T. ) ;
#46628 = AXIS2_PLACEMENT_3D ( 'NONE', #2988, #42938, #82852 ) ;
#46630 = DIRECTION ( 'NONE',  ( 0.000000000000000000, 1.000000000000000000, 0.000000000000000000 ) ) ;
#46631 = ADVANCED_FACE ( 'NONE', ( #4939 ), #52091, .T. ) ;
#46632 = EDGE_CURVE ( 'NONE', #96281, #93919, #129476, .T. ) ;
#46633 = ORIENTED_EDGE ( 'NONE', *, *, #56536, .F. ) ;
#46634 = DIRECTION ( 'NONE',  ( 0.000000000000000000, 0.000000000000000000, 1.000000000000000000 ) ) ;
#46635 = DIRECTION ( 'NONE',  ( 0.000000000000000000, 0.000000000000000000, 1.000000000000000000 ) ) ;
#46636 = CIRCLE ( 'NONE', #103070, 0.06509327318403745899 ) ;
#46637 = AXIS2_PLACEMENT_3D ( 'NONE', #42969, #10863, #102501 ) ;
#46638 = EDGE_CURVE ( 'NONE', #26852, #60457, #73012, .T. ) ;
#46639 = AXIS2_PLACEMENT_3D ( 'NONE', #21909, #111557, #71635 ) ;
#46640 = CIRCLE ( 'NONE', #2713, 0.1000000000000000472 ) ;
#46641 = EDGE_CURVE ( 'NONE', #108185, #40494, #121035, .T. ) ;
#46642 = EDGE_LOOP ( 'NONE', ( #105667, #35233, #49343, #45143 ) ) ;
#46643 = CARTESIAN_POINT ( 'NONE',  ( 185.3750000000000284, 8.891194145520236347, 5.444286225454521982E-16 ) ) ;
#46644 = LINE ( 'NONE', #108135, #89265 ) ;
#46645 = DIRECTION ( 'NONE',  ( -0.000000000000000000, 1.000000000000000000, -0.000000000000000000 ) ) ;
#46646 = EDGE_CURVE ( 'NONE', #103825, #106452, #33769, .T. ) ;
#46647 =( NAMED_UNIT ( * ) PLANE_ANGLE_UNIT ( ) SI_UNIT ( $, .RADIAN. ) );
#46648 = PLANE ( 'NONE',  #7817 ) ;
#46649 = ORIENTED_EDGE ( 'NONE', *, *, #22353, .T. ) ;
#46650 = CIRCLE ( 'NONE', #55055, 0.09999999999999982514 ) ;
#46651 = EDGE_CURVE ( 'NONE', #5985, #30750, #113626, .T. ) ;
#46652 = ADVANCED_FACE ( 'NONE', ( #84152 ), #16548, .T. ) ;
#46653 = EDGE_CURVE ( 'NONE', #59036, #101170, #89735, .T. ) ;
#46654 = CARTESIAN_POINT ( 'NONE',  ( 6.649999999999930189, 2.500000000000000000, -1.372243186433550033 ) ) ;
#46655 = DIRECTION ( 'NONE',  ( 0.000000000000000000, 0.000000000000000000, 1.000000000000000000 ) ) ;
#46656 = ORIENTED_EDGE ( 'NONE', *, *, #16748, .T. ) ;
#46657 = DIRECTION ( 'NONE',  ( 0.000000000000000000, 0.000000000000000000, 1.000000000000000000 ) ) ;
#46658 = LINE ( 'NONE', #35559, #85255 ) ;
#46659 = ADVANCED_FACE ( 'NONE', ( #96537 ), #127395, .T. ) ;
#46660 = CARTESIAN_POINT ( 'NONE',  ( -9.600000000000006750, 2.500000000000000000, -0.7928203230275543412 ) ) ;
#46661 = CIRCLE ( 'NONE', #75897, 0.1000000000000000472 ) ;
#46662 = ORIENTED_EDGE ( 'NONE', *, *, #119077, .F. ) ;
#46663 = DIRECTION ( 'NONE',  ( 0.000000000000000000, -0.000000000000000000, 1.000000000000000000 ) ) ;
#46664 = EDGE_LOOP ( 'NONE', ( #76529, #41282, #72574, #9484 ) ) ;
#46665 = DIRECTION ( 'NONE',  ( 0.000000000000000000, 1.000000000000000000, 0.000000000000000000 ) ) ;
#46666 = FACE_OUTER_BOUND ( 'NONE', #112896, .T. ) ;
#46667 = CARTESIAN_POINT ( 'NONE',  ( -0.2000000000000347888, 2.500000000000000000, 0.2464101615137758439 ) ) ;
#46668 = AXIS2_PLACEMENT_3D ( 'NONE', #23460, #103966, #35235 ) ;
#46669 = VERTEX_POINT ( 'NONE', #117450 ) ;
#46670 = CIRCLE ( 'NONE', #126074, 0.06509327318403745899 ) ;
#46671 = AXIS2_PLACEMENT_3D ( 'NONE', #62615, #112350, #82897 ) ;
#46672 = DIRECTION ( 'NONE',  ( 0.000000000000000000, 0.000000000000000000, 1.000000000000000000 ) ) ;
#46673 = DIRECTION ( 'NONE',  ( -1.000000000000000000, -0.000000000000000000, -0.000000000000000000 ) ) ;
#46674 = ORIENTED_EDGE ( 'NONE', *, *, #100243, .T. ) ;
#46675 = AXIS2_PLACEMENT_3D ( 'NONE', #84348, #7055, #5761 ) ;
#46676 = EDGE_LOOP ( 'NONE', ( #19262, #84734, #43082, #96530 ) ) ;
#46677 = CARTESIAN_POINT ( 'NONE',  ( 129.5000000000000000, 1.375000000000002665, -7.576237522675752345 ) ) ;
#46678 = AXIS2_PLACEMENT_3D ( 'NONE', #52351, #65220, #42558 ) ;
#46679 = AXIS2_PLACEMENT_3D ( 'NONE', #45203, #85108, #25530 ) ;
#46680 = VERTEX_POINT ( 'NONE', #17993 ) ;
#46681 = CARTESIAN_POINT ( 'NONE',  ( -1.650000000000035216, 12.50000000000000000, -5.737276932171712751 ) ) ;
#46682 = CARTESIAN_POINT ( 'NONE',  ( -4.350000000000023626, 2.500000000000000000, 2.511473670974873507 ) ) ;
#46683 = ORIENTED_EDGE ( 'NONE', *, *, #105746, .T. ) ;
#46684 = VERTEX_POINT ( 'NONE', #124732 ) ;
#46685 = CARTESIAN_POINT ( 'NONE',  ( -11.64999999999999680, 2.500000000000000000, -2.857883832488649745 ) ) ;
#46686 = FACE_OUTER_BOUND ( 'NONE', #89966, .T. ) ;
#46687 = VERTEX_POINT ( 'NONE', #7525 ) ;
#46688 = CARTESIAN_POINT ( 'NONE',  ( 1.849999999999948130, 12.50000000000000000, 6.148780366869520009 ) ) ;
#46689 = CARTESIAN_POINT ( 'NONE',  ( 12.89999999999989910, 2.500000000000000000, -0.7928203230275543412 ) ) ;
#46690 = EDGE_CURVE ( 'NONE', #126577, #40083, #119074, .T. ) ;
#46691 = AXIS2_PLACEMENT_3D ( 'NONE', #110884, #2215, #42161 ) ;
#46692 = CONICAL_SURFACE ( 'NONE', #40451, 0.1000000000000002554, 0.003490658503988666988 ) ;
#46693 = AXIS2_PLACEMENT_3D ( 'NONE', #112427, #31299, #111777 ) ;
#46694 = DIRECTION ( 'NONE',  ( 0.000000000000000000, 1.000000000000000000, 0.000000000000000000 ) ) ;
#46695 = CARTESIAN_POINT ( 'NONE',  ( 4.199999999999939782, 2.500000000000000000, -2.276824562219559311E-15 ) ) ;
#46696 = CARTESIAN_POINT ( 'NONE',  ( 3.749999999999942268, 12.50000000000000000, -1.472243186433550122 ) ) ;
#46697 = CONICAL_SURFACE ( 'NONE', #719, 0.1000000000000002554, 0.003490658503988666988 ) ;
#46698 = DIRECTION ( 'NONE',  ( 0.000000000000000000, 0.000000000000000000, 1.000000000000000000 ) ) ;
#46699 = EDGE_LOOP ( 'NONE', ( #57494, #103452, #59559, #28065 ) ) ;
#46700 = VERTEX_POINT ( 'NONE', #84802 ) ;
#46701 = ORIENTED_EDGE ( 'NONE', *, *, #111327, .T. ) ;
#46702 = ORIENTED_EDGE ( 'NONE', *, *, #88816, .F. ) ;
#46703 = DIRECTION ( 'NONE',  ( 0.000000000000000000, 0.000000000000000000, 1.000000000000000000 ) ) ;
#46704 = CARTESIAN_POINT ( 'NONE',  ( 9.549999999999915445, 12.50000000000000000, 6.560283801567334372 ) ) ;
#46705 = LINE ( 'NONE', #25123, #32234 ) ;
#46706 = ORIENTED_EDGE ( 'NONE', *, *, #16164, .F. ) ;
#46707 = EDGE_CURVE ( 'NONE', #57903, #89650, #68886, .T. ) ;
#46708 = FACE_BOUND ( 'NONE', #110475, .T. ) ;
#46709 = CARTESIAN_POINT ( 'NONE',  ( -2.100000000000034284, 2.500000000000000000, -2.385244779468109755E-15 ) ) ;
#46710 = CARTESIAN_POINT ( 'NONE',  ( -3.750000000000031086, 2.500000000000000000, -5.702370205355749455 ) ) ;
#46711 = DIRECTION ( 'NONE',  ( -0.000000000000000000, 1.000000000000000000, -0.000000000000000000 ) ) ;
#46712 = DIRECTION ( 'NONE',  ( 0.000000000000000000, 0.000000000000000000, 1.000000000000000000 ) ) ;
#46713 = CARTESIAN_POINT ( 'NONE',  ( 8.099999999999921485, 12.50000000000000000, -0.4115034346978157509 ) ) ;
#46714 = DIRECTION ( 'NONE',  ( 0.000000000000000000, 1.000000000000000000, 0.000000000000000000 ) ) ;
#46715 = DIRECTION ( 'NONE',  ( 0.000000000000000000, 0.000000000000000000, 1.000000000000000000 ) ) ;
#46716 = CARTESIAN_POINT ( 'NONE',  ( -13.74999999999995381, 2.500000000000000000, 2.165063509461101265 ) ) ;
#46717 = VECTOR ( 'NONE', #35969, 1000.000000000000000 ) ;
#46718 = AXIS2_PLACEMENT_3D ( 'NONE', #117529, #58009, #97912 ) ;
#46719 = FACE_OUTER_BOUND ( 'NONE', #77117, .T. ) ;
#46720 = DIRECTION ( 'NONE',  ( 0.000000000000000000, -0.9999939076577903929, 0.003490651415223739937 ) ) ;
#46721 = CONICAL_SURFACE ( 'NONE', #103148, 0.1000000000000002554, 0.003490658503988666988 ) ;
#46723 = ORIENTED_EDGE ( 'NONE', *, *, #42782, .T. ) ;
#46722 = AXIS2_PLACEMENT_3D ( 'NONE', #65924, #57408, #37131 ) ;
#46724 = ORIENTED_EDGE ( 'NONE', *, *, #121331, .T. ) ;
#46725 = EDGE_LOOP ( 'NONE', ( #77332, #78268 ) ) ;
#46726 = VECTOR ( 'NONE', #97403, 1000.000000000000000 ) ;
#46727 = ORIENTED_EDGE ( 'NONE', *, *, #39935, .T. ) ;
#46729 = AXIS2_PLACEMENT_3D ( 'NONE', #117540, #28554, #19353 ) ;
#46728 = CARTESIAN_POINT ( 'NONE',  ( 12.49999999999993960, 12.50000000000000000, -4.330127018922201643 ) ) ;
#46730 = AXIS2_PLACEMENT_3D ( 'NONE', #21173, #62412, #102953 ) ;
#46731 = DIRECTION ( 'NONE',  ( 0.000000000000000000, 0.000000000000000000, -1.000000000000000000 ) ) ;
#46733 = EDGE_LOOP ( 'NONE', ( #72684, #85228 ) ) ;
#46732 = VERTEX_POINT ( 'NONE', #44897 ) ;
#46734 = EDGE_LOOP ( 'NONE', ( #105521, #105360, #121781, #23573 ) ) ;
#46735 = CARTESIAN_POINT ( 'NONE',  ( -1.700000000000034817, 2.500000000000000000, -4.430127018922202176 ) ) ;
#46736 = CONICAL_SURFACE ( 'NONE', #36288, 0.09999999999999982514, 0.003490658503988666988 ) ;
#46737 = VECTOR ( 'NONE', #71104, 1000.000000000000000 ) ;
#46738 = ADVANCED_FACE ( 'NONE', ( #46830 ), #93945, .T. ) ;
#46739 = CARTESIAN_POINT ( 'NONE',  ( 10.30524027349368765, -1.500000000000191402, 9.130939513664339202 ) ) ;
#46740 = LINE ( 'NONE', #107591, #104387 ) ;
#46741 = PLANE ( 'NONE',  #88629 ) ;
#46742 = CONICAL_SURFACE ( 'NONE', #63463, 0.1000000000000002554, 0.003490658503988666988 ) ;
#46743 = CARTESIAN_POINT ( 'NONE',  ( -11.84999999999999787, 2.500000000000000000, -6.941600689897074794 ) ) ;
#46744 = CIRCLE ( 'NONE', #2823, 0.09999999999999982514 ) ;
#46745 = EDGE_LOOP ( 'NONE', ( #65022, #118301 ) ) ;
#46746 = EDGE_CURVE ( 'NONE', #59695, #113633, #121127, .T. ) ;
#46747 = VERTEX_POINT ( 'NONE', #116191 ) ;
#46748 = ORIENTED_EDGE ( 'NONE', *, *, #61733, .T. ) ;
#46749 = VERTEX_POINT ( 'NONE', #6861 ) ;
#46750 = ADVANCED_FACE ( 'NONE', ( #56614 ), #74990, .T. ) ;
#46752 = EDGE_CURVE ( 'NONE', #107557, #22212, #65141, .T. ) ;
#46751 = DIRECTION ( 'NONE',  ( 0.000000000000000000, 0.000000000000000000, 1.000000000000000000 ) ) ;
#46753 =( BOUNDED_CURVE ( )  B_SPLINE_CURVE ( 2, ( #2635, #42603, #63520, #23579, #103442, #13746, #93615 ),
 .UNSPECIFIED., .F., .F. ) 
 B_SPLINE_CURVE_WITH_KNOTS ( ( 3, 2, 2, 3 ),
 ( 0.3571428571428574283, 0.3809523809523812643, 0.4047619047619051003, 0.4285714285714289362 ),
 .UNSPECIFIED. ) 
 CURVE ( )  GEOMETRIC_REPRESENTATION_ITEM ( )  RATIONAL_B_SPLINE_CURVE ( ( 0.9999999999999984457, 0.8660254037844402619, 1.000000000000000000, 0.8660254037844387076, 1.000000000000000000, 0.8660254037844364872, 1.000000000000002220 ) ) 
 REPRESENTATION_ITEM ( '' )  );
#46755 = VERTEX_POINT ( 'NONE', #95280 ) ;
#46754 = ADVANCED_FACE ( 'NONE', ( #105075 ), #98132, .T. ) ;
#46756 = EDGE_CURVE ( 'NONE', #72001, #102540, #125336, .T. ) ;
#46758 = VERTEX_POINT ( 'NONE', #37007 ) ;
#46757 = EDGE_CURVE ( 'NONE', #115958, #78678, #86069, .T. ) ;
#46759 = CIRCLE ( 'NONE', #7012, 0.06509327318403745899 ) ;
#46760 = FACE_OUTER_BOUND ( 'NONE', #76852, .T. ) ;
#46761 = CARTESIAN_POINT ( 'NONE',  ( 6.249999999999928946, 12.50000000000000000, 2.857883832488649301 ) ) ;
#46762 = DIRECTION ( 'NONE',  ( 0.000000000000000000, -0.000000000000000000, 1.000000000000000000 ) ) ;
#46763 = CARTESIAN_POINT ( 'NONE',  ( 14.19999999999989626, 12.50000000000000000, -2.276824562219559311E-15 ) ) ;
#46764 = DIRECTION ( 'NONE',  ( 0.000000000000000000, 0.000000000000000000, 1.000000000000000000 ) ) ;
#46765 = EDGE_CURVE ( 'NONE', #34089, #22876, #54234, .T. ) ;
#46767 = ORIENTED_EDGE ( 'NONE', *, *, #91890, .F. ) ;
#46766 = AXIS2_PLACEMENT_3D ( 'NONE', #77076, #57440, #426 ) ;
#46768 = CARTESIAN_POINT ( 'NONE',  ( -12.04999999999999716, 12.50000000000000000, -2.165063509461097713 ) ) ;
#46770 = EDGE_CURVE ( 'NONE', #37854, #20339, #14497, .T. ) ;
#46769 = CONICAL_SURFACE ( 'NONE', #119918, 0.1000000000000000472, 0.003490658503988666988 ) ;
#46771 = VECTOR ( 'NONE', #35092, 1000.000000000000000 ) ;
#46772 = ADVANCED_FACE ( 'NONE', ( #75612 ), #27175, .T. ) ;
#46773 = ORIENTED_EDGE ( 'NONE', *, *, #102731, .T. ) ;
#46774 = CARTESIAN_POINT ( 'NONE',  ( 8.549999999999920774, 12.50000000000000000, 6.213873640053559022 ) ) ;
#46775 = ORIENTED_EDGE ( 'NONE', *, *, #13713, .T. ) ;
#46776 = CARTESIAN_POINT ( 'NONE',  ( -8.550000000000011369, 2.500000000000000000, -2.611473670974877592 ) ) ;
#46777 = CARTESIAN_POINT ( 'NONE',  ( 10.44999999999991047, 2.500000000000000000, 2.265063509461097357 ) ) ;
#46778 = ORIENTED_EDGE ( 'NONE', *, *, #3486, .T. ) ;
#46779 = CARTESIAN_POINT ( 'NONE',  ( -6.249999999999981348, 2.500000000000000000, 2.265063509461097357 ) ) ;
#46781 = CIRCLE ( 'NONE', #53037, 0.06509327318403745899 ) ;
#46780 = CARTESIAN_POINT ( 'NONE',  ( -6.050000000000022027, 2.500000000000000000, -1.718653347947326049 ) ) ;
#46782 = EDGE_LOOP ( 'NONE', ( #13530, #116164, #6283, #75391 ) ) ;
#46783 = AXIS2_PLACEMENT_3D ( 'NONE', #102471, #80903, #63193 ) ;
#46784 = B_SPLINE_CURVE_WITH_KNOTS ( 'NONE', 3,
 ( #37604, #8120, #97157, #226 ),
 .UNSPECIFIED., .F., .F.,
 ( 4, 4 ),
 ( 0.001845843513054588186, 0.003313552284081220344 ),
 .UNSPECIFIED. ) ;
#46785 = AXIS2_PLACEMENT_3D ( 'NONE', #122721, #93910, #13396 ) ;
#46786 = DIRECTION ( 'NONE',  ( 0.000000000000000000, -0.9999939076577903929, 0.003490651415223739937 ) ) ;
#46787 = ORIENTED_EDGE ( 'NONE', *, *, #127884, .T. ) ;
#46788 = VERTEX_POINT ( 'NONE', #46169 ) ;
#46789 = DIRECTION ( 'NONE',  ( 0.000000000000000000, 0.000000000000000000, 1.000000000000000000 ) ) ;
#46790 = CARTESIAN_POINT ( 'NONE',  ( 10.59999999999990905, 12.50000000000000000, -3.983716857408426293 ) ) ;
#46791 = CARTESIAN_POINT ( 'NONE',  ( 185.2968750003414300, 8.734944146203032389, 5.348610694689227483E-16 ) ) ;
#46792 = AXIS2_PLACEMENT_3D ( 'NONE', #26598, #116886, #77613 ) ;
#46793 = CARTESIAN_POINT ( 'NONE',  ( -7.500000000000001776, 2.500000000000000000, 10.00000000000000178 ) ) ;
#46794 = CARTESIAN_POINT ( 'NONE',  ( -6.250000000000017764, 12.50000000000000000, 7.253104124594885960 ) ) ;
#46795 = CIRCLE ( 'NONE', #28004, 0.06509327318403745899 ) ;
#46796 = CIRCLE ( 'NONE', #63521, 0.1000000000000002554 ) ;
#46797 = CARTESIAN_POINT ( 'NONE',  ( -0.6500000000000394351, 2.500000000000000000, 2.511473670974873507 ) ) ;
#46798 = AXIS2_PLACEMENT_3D ( 'NONE', #49307, #48004, #38850 ) ;
#46799 = EDGE_LOOP ( 'NONE', ( #95674, #106692, #75345, #4557 ) ) ;
#46800 = AXIS2_PLACEMENT_3D ( 'NONE', #82762, #120731, #84670 ) ;
#46801 = CARTESIAN_POINT ( 'NONE',  ( 10.84999999999990905, 2.500000000000000000, -7.088010851410853519 ) ) ;
#46802 = ORIENTED_EDGE ( 'NONE', *, *, #91933, .T. ) ;
#46803 = FACE_OUTER_BOUND ( 'NONE', #78220, .T. ) ;
#46804 = CARTESIAN_POINT ( 'NONE',  ( -10.45000000000000462, 12.50000000000000000, -6.430097255199260786 ) ) ;
#46805 = DIRECTION ( 'NONE',  ( 0.000000000000000000, 0.000000000000000000, 1.000000000000000000 ) ) ;
#46806 = EDGE_CURVE ( 'NONE', #20962, #69086, #73105, .T. ) ;
#46807 = DIRECTION ( 'NONE',  ( 0.000000000000000000, 0.000000000000000000, 1.000000000000000000 ) ) ;
#46808 = DIRECTION ( 'NONE',  ( -4.274815082592931898E-19, -0.9999939076577903929, -0.003490651415223739937 ) ) ;
#46809 = ORIENTED_EDGE ( 'NONE', *, *, #81745, .F. ) ;
#46810 = EDGE_CURVE ( 'NONE', #72078, #78871, #114853, .T. ) ;
#46811 = EDGE_CURVE ( 'NONE', #98383, #24036, #29209, .T. ) ;
#46812 = CARTESIAN_POINT ( 'NONE',  ( -13.09999999999999076, 2.500000000000000000, 4.676537180435972552 ) ) ;
#46813 = CARTESIAN_POINT ( 'NONE',  ( -9.600000000000006750, 12.50000000000000000, 0.6928203230275494784 ) ) ;
#46814 = AXIS2_PLACEMENT_3D ( 'NONE', #39220, #100047, #119043 ) ;
#46815 = CONICAL_SURFACE ( 'NONE', #107445, 0.1000000000000000472, 0.003490658503988666988 ) ;
#46816 = ORIENTED_EDGE ( 'NONE', *, *, #60059, .F. ) ;
#46817 = EDGE_CURVE ( 'NONE', #70962, #62174, #4126, .T. ) ;
#46818 = CARTESIAN_POINT ( 'NONE',  ( 11.64999999999990798, 2.500000000000000000, 5.802370205355744659 ) ) ;
#46819 = AXIS2_PLACEMENT_3D ( 'NONE', #31066, #122007, #80800 ) ;
#46820 = CONICAL_SURFACE ( 'NONE', #71963, 0.09999999999999982514, 0.003490658503988666988 ) ;
#46821 = ORIENTED_EDGE ( 'NONE', *, *, #55666, .F. ) ;
#46822 = AXIS2_PLACEMENT_3D ( 'NONE', #40207, #41514, #120052 ) ;
#46823 = ORIENTED_EDGE ( 'NONE', *, *, #70911, .F. ) ;
#46824 = DIRECTION ( 'NONE',  ( 0.000000000000000000, 0.000000000000000000, -1.000000000000000000 ) ) ;
#46825 = AXIS2_PLACEMENT_3D ( 'NONE', #45476, #84729, #24529 ) ;
#46826 = VECTOR ( 'NONE', #30865, 1000.000000000000000 ) ;
#46827 = VERTEX_POINT ( 'NONE', #48117 ) ;
#46828 = CARTESIAN_POINT ( 'NONE',  ( 185.2812500006828031, 0.000000000000000000, 7.700000000000000178 ) ) ;
#46829 = LINE ( 'NONE', #8805, #69476 ) ;
#46830 = FACE_OUTER_BOUND ( 'NONE', #87791, .T. ) ;
#46832 = ORIENTED_EDGE ( 'NONE', *, *, #48377, .F. ) ;
#46831 = AXIS2_PLACEMENT_3D ( 'NONE', #64033, #75139, #25376 ) ;
#46833 = AXIS2_PLACEMENT_3D ( 'NONE', #64916, #114665, #84571 ) ;
#46834 = AXIS2_PLACEMENT_3D ( 'NONE', #87089, #68747, #20299 ) ;
#46835 = FACE_BOUND ( 'NONE', #54877, .T. ) ;
#46837 = ORIENTED_EDGE ( 'NONE', *, *, #118716, .T. ) ;
#46836 = DIRECTION ( 'NONE',  ( -0.000000000000000000, -1.000000000000000000, -0.000000000000000000 ) ) ;
#46838 = AXIS2_PLACEMENT_3D ( 'NONE', #35348, #104707, #115154 ) ;
#46839 = CARTESIAN_POINT ( 'NONE',  ( 3.349999999999941913, 2.500000000000000000, 5.702370205355745014 ) ) ;
#46840 = DIRECTION ( 'NONE',  ( 0.000000000000000000, -0.000000000000000000, 1.000000000000000000 ) ) ;
#46841 = ADVANCED_FACE ( 'NONE', ( #72107 ), #87663, .T. ) ;
#46842 = EDGE_LOOP ( 'NONE', ( #86111, #86616, #1422, #52560 ) ) ;
#46843 = ORIENTED_EDGE ( 'NONE', *, *, #43037, .T. ) ;
#46844 = ORIENTED_EDGE ( 'NONE', *, *, #102331, .T. ) ;
#46846 = VECTOR ( 'NONE', #69595, 1000.000000000000000 ) ;
#46845 = DIRECTION ( 'NONE',  ( 0.000000000000000000, 0.000000000000000000, -1.000000000000000000 ) ) ;
#46847 = DIRECTION ( 'NONE',  ( 0.000000000000000000, 0.000000000000000000, -1.000000000000000000 ) ) ;
#46848 = CARTESIAN_POINT ( 'NONE',  ( 14.14999999999989377, 12.50000000000000000, -1.537336459617587581 ) ) ;
#46849 = FACE_BOUND ( 'NONE', #60, .T. ) ;
#46850 = ORIENTED_EDGE ( 'NONE', *, *, #40606, .F. ) ;
#46851 = DIRECTION ( 'NONE',  ( 0.000000000000000000, 1.000000000000000000, 0.000000000000000000 ) ) ;
#46852 = CARTESIAN_POINT ( 'NONE',  ( 12.89999999999989910, 2.500000000000000000, 0.7928203230275495672 ) ) ;
#46853 = AXIS2_PLACEMENT_3D ( 'NONE', #98823, #39927, #119755 ) ;
#46854 = DIRECTION ( 'NONE',  ( -0.000000000000000000, -1.000000000000000000, -0.000000000000000000 ) ) ;
#46855 = EDGE_CURVE ( 'NONE', #111888, #84054, #79371, .T. ) ;
#46856 = CARTESIAN_POINT ( 'NONE',  ( 2.949999999999943334, 2.500000000000000000, 6.595190528383296780 ) ) ;
#46857 = CARTESIAN_POINT ( 'NONE',  ( 12.09999999999990195, 12.50000000000000000, 0.6928203230275494784 ) ) ;
#46858 = DIRECTION ( 'NONE',  ( -0.000000000000000000, -1.000000000000000000, -0.000000000000000000 ) ) ;
#46859 = CARTESIAN_POINT ( 'NONE',  ( 2.949999999999943334, 2.500000000000000000, 6.495190528383297135 ) ) ;
#46860 = CONICAL_SURFACE ( 'NONE', #23884, 0.09999999999999982514, 0.003490658503988666988 ) ;
#46861 = CONICAL_SURFACE ( 'NONE', #25928, 0.09999999999999982514, 0.003490658503988666988 ) ;
#46862 = EDGE_LOOP ( 'NONE', ( #48975, #84684, #16415, #105869 ) ) ;
#46863 = EDGE_LOOP ( 'NONE', ( #22356, #12541 ) ) ;
#46864 = EDGE_LOOP ( 'NONE', ( #6179, #16878, #34352, #106996 ) ) ;
#46865 = ORIENTED_EDGE ( 'NONE', *, *, #76473, .T. ) ;
#46866 = EDGE_LOOP ( 'NONE', ( #51098, #57322 ) ) ;
#46867 = DIRECTION ( 'NONE',  ( 0.000000000000000000, 0.000000000000000000, 1.000000000000000000 ) ) ;
#46868 = CARTESIAN_POINT ( 'NONE',  ( 1.849999999999948130, 2.500000000000000000, 6.248780366869520542 ) ) ;
#46869 = ORIENTED_EDGE ( 'NONE', *, *, #83299, .T. ) ;
#46870 = EDGE_CURVE ( 'NONE', #123660, #56688, #122493, .T. ) ;
#46871 = FACE_BOUND ( 'NONE', #10713, .T. ) ;
#46872 = AXIS2_PLACEMENT_3D ( 'NONE', #57315, #97233, #109641 ) ;
#46873 = DIRECTION ( 'NONE',  ( 0.000000000000000000, 0.000000000000000000, 1.000000000000000000 ) ) ;
#46874 = VECTOR ( 'NONE', #6851, 1000.000000000000000 ) ;
#46875 = CARTESIAN_POINT ( 'NONE',  ( 1.449999999999952660, 2.500000000000000000, -6.841600689897078702 ) ) ;
#46876 = CARTESIAN_POINT ( 'NONE',  ( -7.900000000000011013, 2.500000000000000000, 3.637306695894644726 ) ) ;
#46877 = CARTESIAN_POINT ( 'NONE',  ( -3.100000000000028955, 12.50000000000000000, 4.741630453620009789 ) ) ;
#46878 = CARTESIAN_POINT ( 'NONE',  ( -11.44999999999999751, 2.500000000000000000, 6.248780366869521430 ) ) ;
#46879 = VERTEX_POINT ( 'NONE', #88003 ) ;
#46880 = CARTESIAN_POINT ( 'NONE',  ( -1.250000000000001554, 2.500000000000000000, 6.395190528383296602 ) ) ;
#46881 = EDGE_LOOP ( 'NONE', ( #60166, #74109 ) ) ;
#46882 = AXIS2_PLACEMENT_3D ( 'NONE', #38655, #49111, #19639 ) ;
#46883 = ORIENTED_EDGE ( 'NONE', *, *, #22251, .T. ) ;
#46884 = EDGE_LOOP ( 'NONE', ( #85706, #77474 ) ) ;
#46885 = LINE ( 'NONE', #128695, #94431 ) ;
#46886 = DIRECTION ( 'NONE',  ( 0.000000000000000000, 1.000000000000000000, 0.000000000000000000 ) ) ;
#46888 = AXIS2_PLACEMENT_3D ( 'NONE', #19831, #59774, #99682 ) ;
#46887 = DIRECTION ( 'NONE',  ( 1.000000000000000000, 0.000000000000000000, -0.000000000000000000 ) ) ;
#46889 = ORIENTED_EDGE ( 'NONE', *, *, #51023, .T. ) ;
#46890 = CARTESIAN_POINT ( 'NONE',  ( 7.306656945292924199, 2.499999999999746425, -9.704971168060907871 ) ) ;
#46891 = AXIS2_PLACEMENT_3D ( 'NONE', #113002, #23317, #1109 ) ;
#46892 = CARTESIAN_POINT ( 'NONE',  ( -10.20000000000000462, 2.500000000000000000, 4.676537180435972552 ) ) ;
#46893 = EDGE_CURVE ( 'NONE', #60832, #45836, #47980, .T. ) ;
#46894 = LINE ( 'NONE', #5651, #87086 ) ;
#46895 = CARTESIAN_POINT ( 'NONE',  ( 184.7395833340161460, 4.445597072760117285, 7.699999999999999289 ) ) ;
#46896 = DIRECTION ( 'NONE',  ( 0.000000000000000000, 0.000000000000000000, 1.000000000000000000 ) ) ;
#46897 = DIRECTION ( 'NONE',  ( -4.274815082592931898E-19, -0.9999939076577903929, -0.003490651415223739937 ) ) ;
#46898 = CARTESIAN_POINT ( 'NONE',  ( -1.900000000000034550, 2.500000000000000000, 4.676537180435972552 ) ) ;
#46899 = VERTEX_POINT ( 'NONE', #769 ) ;
#46900 = DIRECTION ( 'NONE',  ( -0.000000000000000000, -1.000000000000000000, -0.000000000000000000 ) ) ;
#46901 = ADVANCED_FACE ( 'NONE', ( #127953 ), #92368, .T. ) ;
#46902 = ORIENTED_EDGE ( 'NONE', *, *, #32335, .F. ) ;
#46904 = EDGE_LOOP ( 'NONE', ( #47834, #86956 ) ) ;
#46903 = AXIS2_PLACEMENT_3D ( 'NONE', #1357, #121772, #10528 ) ;
#46905 = DIRECTION ( 'NONE',  ( -0.000000000000000000, 1.000000000000000000, -0.000000000000000000 ) ) ;
#46906 = CIRCLE ( 'NONE', #65664, 0.06509327318403741736 ) ;
#46907 = AXIS2_PLACEMENT_3D ( 'NONE', #13425, #53374, #63836 ) ;
#46908 = EDGE_CURVE ( 'NONE', #72759, #14578, #60603, .T. ) ;
#46909 = DIRECTION ( 'NONE',  ( 0.000000000000000000, 1.846105847067148022E-16, -1.000000000000000000 ) ) ;
#46911 = ADVANCED_FACE ( 'NONE', ( #51824 ), #20874, .T. ) ;
#46910 = CARTESIAN_POINT ( 'NONE',  ( -4.350000000000027178, 12.50000000000000000, -6.148780366869526226 ) ) ;
#46912 = EDGE_CURVE ( 'NONE', #28244, #49584, #121830, .T. ) ;
#46913 = EDGE_CURVE ( 'NONE', #92549, #23743, #41995, .T. ) ;
#46914 = VERTEX_POINT ( 'NONE', #72746 ) ;
#46915 = ORIENTED_EDGE ( 'NONE', *, *, #16446, .T. ) ;
#46916 = DIRECTION ( 'NONE',  ( -0.000000000000000000, 1.000000000000000000, -0.000000000000000000 ) ) ;
#46917 = AXIS2_PLACEMENT_3D ( 'NONE', #59726, #102675, #63411 ) ;
#46918 = CIRCLE ( 'NONE', #49072, 0.1000000000000002554 ) ;
#46919 = VECTOR ( 'NONE', #2975, 1000.000000000000000 ) ;
#46920 = PLANE ( 'NONE',  #68342 ) ;
#46921 = EDGE_CURVE ( 'NONE', #102305, #125960, #68384, .T. ) ;
#46922 = FACE_OUTER_BOUND ( 'NONE', #29566, .T. ) ;
#46923 = ORIENTED_EDGE ( 'NONE', *, *, #96325, .F. ) ;
#46924 = VERTEX_POINT ( 'NONE', #112025 ) ;
#46925 = EDGE_CURVE ( 'NONE', #90822, #48868, #94028, .T. ) ;
#46926 = CARTESIAN_POINT ( 'NONE',  ( -9.150000000000005684, 12.50000000000000000, 7.188010851410848723 ) ) ;
#46927 = EDGE_CURVE ( 'NONE', #4486, #119497, #90422, .T. ) ;
#46928 = ORIENTED_EDGE ( 'NONE', *, *, #99508, .F. ) ;
#46929 = DIRECTION ( 'NONE',  ( 0.000000000000000000, 0.000000000000000000, 1.000000000000000000 ) ) ;
#46930 = AXIS2_PLACEMENT_3D ( 'NONE', #109762, #10881, #10268 ) ;
#46931 = ADVANCED_FACE ( 'NONE', ( #100893 ), #89817, .T. ) ;
#46932 = AXIS2_PLACEMENT_3D ( 'NONE', #12307, #20850, #92158 ) ;
#46933 = VECTOR ( 'NONE', #113175, 1000.000000000000000 ) ;
#46934 = EDGE_CURVE ( 'NONE', #85762, #13568, #31531, .T. ) ;
#46935 = CARTESIAN_POINT ( 'NONE',  ( -7.100000000000013856, 12.50000000000000000, 3.637306695894644726 ) ) ;
#46936 = ORIENTED_EDGE ( 'NONE', *, *, #8107, .F. ) ;
#46937 = CARTESIAN_POINT ( 'NONE',  ( 5.649999999999932854, 2.500000000000000000, 2.411473670974873862 ) ) ;
#46938 = LINE ( 'NONE', #58039, #65095 ) ;
#46939 = DIRECTION ( 'NONE',  ( 0.000000000000000000, -0.9999939076577903929, 0.003490651415223739937 ) ) ;
#46940 = AXIS2_PLACEMENT_3D ( 'NONE', #45017, #62085, #62728 ) ;
#46942 = EDGE_CURVE ( 'NONE', #36299, #6668, #10400, .T. ) ;
#46941 = CARTESIAN_POINT ( 'NONE',  ( 4.549999999999935874, 12.50000000000000000, 6.560283801567334372 ) ) ;
#46943 = ORIENTED_EDGE ( 'NONE', *, *, #30238, .F. ) ;
#46944 = DIRECTION ( 'NONE',  ( -0.000000000000000000, 1.000000000000000000, -0.000000000000000000 ) ) ;
#46945 = DIRECTION ( 'NONE',  ( 0.000000000000000000, 1.000000000000000000, 0.000000000000000000 ) ) ;
#46946 = ORIENTED_EDGE ( 'NONE', *, *, #26281, .T. ) ;
#46947 = EDGE_LOOP ( 'NONE', ( #1032, #106371 ) ) ;
#46948 = CARTESIAN_POINT ( 'NONE',  ( 184.1718750003414016, 9.264065473108010111E-16, -7.564683531250000925 ) ) ;
#46949 = DIRECTION ( 'NONE',  ( 0.000000000000000000, -0.000000000000000000, 1.000000000000000000 ) ) ;
#46950 = FACE_OUTER_BOUND ( 'NONE', #112903, .T. ) ;
#46951 = DIRECTION ( 'NONE',  ( 0.000000000000000000, 0.000000000000000000, 1.000000000000000000 ) ) ;
#46952 = CONICAL_SURFACE ( 'NONE', #15611, 0.1000000000000002554, 0.003490658503988666988 ) ;
#46953 = CARTESIAN_POINT ( 'NONE',  ( -3.150000000000030109, 2.500000000000000000, 1.918653347947321564 ) ) ;
#46954 = CARTESIAN_POINT ( 'NONE',  ( 0.8499999999999550138, 2.500000000000000000, -5.702370205355749455 ) ) ;
#46955 = LINE ( 'NONE', #38429, #32166 ) ;
#46956 = CARTESIAN_POINT ( 'NONE',  ( 5.599999999999931255, 2.500000000000000000, 4.676537180435972552 ) ) ;
#46957 = DIRECTION ( 'NONE',  ( 0.000000000000000000, -0.9999939076577903929, 0.003490651415223739937 ) ) ;
#46958 = CARTESIAN_POINT ( 'NONE',  ( 13.74999999999989342, 12.50000000000000000, -1.407149913249512663 ) ) ;
#46959 = AXIS2_PLACEMENT_3D ( 'NONE', #71295, #43800, #103357 ) ;
#46960 = VERTEX_POINT ( 'NONE', #2051 ) ;
#46961 = FACE_OUTER_BOUND ( 'NONE', #89112, .T. ) ;
#46962 = EDGE_LOOP ( 'NONE', ( #3170, #110384, #118615, #107093 ) ) ;
#46963 = DIRECTION ( 'NONE',  ( 0.000000000000000000, 0.000000000000000000, 1.000000000000000000 ) ) ;
#46964 = CARTESIAN_POINT ( 'NONE',  ( 11.04999999999990656, 2.500000000000000000, -6.148780366869526226 ) ) ;
#46965 = DIRECTION ( 'NONE',  ( 0.000000000000000000, 0.000000000000000000, -1.000000000000000000 ) ) ;
#46966 = ORIENTED_EDGE ( 'NONE', *, *, #106100, .T. ) ;
#46967 = FACE_OUTER_BOUND ( 'NONE', #78787, .T. ) ;
#46968 = AXIS2_PLACEMENT_3D ( 'NONE', #4131, #114107, #112825 ) ;
#46969 = EDGE_CURVE ( 'NONE', #96613, #50485, #1989, .T. ) ;
#46970 = EDGE_CURVE ( 'NONE', #53584, #128668, #83581, .T. ) ;
#46971 = CARTESIAN_POINT ( 'NONE',  ( 4.149999999999938183, 12.50000000000000000, 2.165063509461097713 ) ) ;
#46973 = EDGE_LOOP ( 'NONE', ( #113458, #51579, #109663, #19697 ) ) ;
#46972 = DIRECTION ( 'NONE',  ( 0.000000000000000000, 0.000000000000000000, 1.000000000000000000 ) ) ;
#46974 = LINE ( 'NONE', #45046, #6109 ) ;
#46975 = ORIENTED_EDGE ( 'NONE', *, *, #60800, .T. ) ;
#46976 = EDGE_CURVE ( 'NONE', #17021, #23771, #58445, .T. ) ;
#46977 = CIRCLE ( 'NONE', #34462, 0.1000000000000002554 ) ;
#46978 = CONICAL_SURFACE ( 'NONE', #120134, 0.1000000000000000472, 0.003490658503988666988 ) ;
#46979 = ORIENTED_EDGE ( 'NONE', *, *, #61871, .F. ) ;
#46980 = EDGE_LOOP ( 'NONE', ( #38084, #49850, #72753, #97639 ) ) ;
#46981 = ORIENTED_EDGE ( 'NONE', *, *, #45603, .F. ) ;
#46982 = DIRECTION ( 'NONE',  ( 0.000000000000000000, 0.000000000000000000, -1.000000000000000000 ) ) ;
#46983 = CONICAL_SURFACE ( 'NONE', #44923, 0.1000000000000002554, 0.003490658503988666988 ) ;
#46984 = CARTESIAN_POINT ( 'NONE',  ( 9.399999999999915090, 2.500000000000000000, 3.883716857408421319 ) ) ;
#46985 = CARTESIAN_POINT ( 'NONE',  ( -6.850000000000013856, 12.50000000000000000, 6.776507416713035248 ) ) ;
#46986 = AXIS2_PLACEMENT_3D ( 'NONE', #44249, #104465, #96561 ) ;
#46987 = CARTESIAN_POINT ( 'NONE',  ( 11.24999999999991118, 12.50000000000000000, -2.857883832488653741 ) ) ;
#46988 = ORIENTED_EDGE ( 'NONE', *, *, #49034, .F. ) ;
#46989 = CARTESIAN_POINT ( 'NONE',  ( -7.300000000000013145, 12.50000000000000000, 3.983716857408420076 ) ) ;
#46990 = ORIENTED_EDGE ( 'NONE', *, *, #41147, .T. ) ;
#46991 = CARTESIAN_POINT ( 'NONE',  ( 23.99354682434742259, -2.839181451644826382, -2.508508607409395186 ) ) ;
#46992 = CARTESIAN_POINT ( 'NONE',  ( 15.62920359459681485, -2.499999999999998668, -5.623946225393044784 ) ) ;
#46993 = DIRECTION ( 'NONE',  ( 0.000000000000000000, 0.000000000000000000, 1.000000000000000000 ) ) ;
#46994 = DIRECTION ( 'NONE',  ( -0.000000000000000000, -1.000000000000000000, -0.000000000000000000 ) ) ;
#46995 = ORIENTED_EDGE ( 'NONE', *, *, #124326, .F. ) ;
#46996 = VERTEX_POINT ( 'NONE', #53109 ) ;
#46997 = ORIENTED_EDGE ( 'NONE', *, *, #46179, .T. ) ;
#46998 = AXIS2_PLACEMENT_3D ( 'NONE', #120833, #71735, #43581 ) ;
#46999 = ORIENTED_EDGE ( 'NONE', *, *, #121810, .F. ) ;
#47000 = LINE ( 'NONE', #126843, #29423 ) ;
#47002 = VECTOR ( 'NONE', #80099, 1000.000000000000000 ) ;
#47001 = CARTESIAN_POINT ( 'NONE',  ( 48.83367117123161449, 2.320420702480692210, 5.300559035860525903 ) ) ;
#47003 = AXIS2_PLACEMENT_3D ( 'NONE', #29197, #8235, #18054 ) ;
#47004 = LINE ( 'NONE', #85621, #58673 ) ;
#47005 = FACE_BOUND ( 'NONE', #33374, .T. ) ;
#47006 = CARTESIAN_POINT ( 'NONE',  ( -10.40000000000000213, 12.50000000000000000, -5.022947341949749678 ) ) ;
#47007 = DIRECTION ( 'NONE',  ( 0.000000000000000000, 0.000000000000000000, 1.000000000000000000 ) ) ;
#47008 = CARTESIAN_POINT ( 'NONE',  ( -15.19999999999998153, 2.500000000000000000, -0.3464101615137759604 ) ) ;
#47009 = FACE_OUTER_BOUND ( 'NONE', #110687, .T. ) ;
#47010 = EDGE_CURVE ( 'NONE', #30131, #79994, #2071, .T. ) ;
#47011 = CONICAL_SURFACE ( 'NONE', #109788, 0.09999999999999982514, 0.003490658503988666988 ) ;
#47012 = CONICAL_SURFACE ( 'NONE', #120160, 0.1000000000000002554, 0.003490658503988666988 ) ;
#47013 = AXIS2_PLACEMENT_3D ( 'NONE', #99092, #9418, #49362 ) ;
#47014 = CARTESIAN_POINT ( 'NONE',  ( 184.2135416670080588, 4.367472073101518859, -7.564683531249999149 ) ) ;
#47015 = CONICAL_SURFACE ( 'NONE', #107646, 0.1000000000000000056, 0.003490658503988666988 ) ;
#47016 = DIRECTION ( 'NONE',  ( -0.000000000000000000, 1.000000000000000000, -0.000000000000000000 ) ) ;
#47017 = FACE_OUTER_BOUND ( 'NONE', #96591, .T. ) ;
#47018 = AXIS2_PLACEMENT_3D ( 'NONE', #118246, #107784, #126787 ) ;
#47019 = CIRCLE ( 'NONE', #5231, 0.06509327318403745899 ) ;
#47020 = DIRECTION ( 'NONE',  ( 0.000000000000000000, 1.000000000000000000, 0.000000000000000000 ) ) ;
#47021 = VERTEX_POINT ( 'NONE', #55676 ) ;
#47022 = ORIENTED_EDGE ( 'NONE', *, *, #111159, .T. ) ;
#47023 = ORIENTED_EDGE ( 'NONE', *, *, #53286, .T. ) ;
#47024 = VERTEX_POINT ( 'NONE', #45870 ) ;
#47025 = VECTOR ( 'NONE', #60645, 1000.000000000000000 ) ;
#47026 = ADVANCED_FACE ( 'NONE', ( #75951 ), #75246, .T. ) ;
#47027 = FACE_OUTER_BOUND ( 'NONE', #80532, .T. ) ;
#47028 = EDGE_CURVE ( 'NONE', #97854, #118876, #68986, .T. ) ;
#47029 = FACE_BOUND ( 'NONE', #11357, .T. ) ;
#47030 = CARTESIAN_POINT ( 'NONE',  ( 8.349999999999923261, 2.500000000000000000, -6.495190528383302464 ) ) ;
#47031 = CARTESIAN_POINT ( 'NONE',  ( 0.6499999999999566125, 12.50000000000000000, -6.776507416713039689 ) ) ;
#47032 = VERTEX_POINT ( 'NONE', #44572 ) ;
#47033 = CARTESIAN_POINT ( 'NONE',  ( -8.750000000000012434, 12.50000000000000000, -5.867463478539781896 ) ) ;
#47034 = ADVANCED_FACE ( 'NONE', ( #55027 ), #45224, .F. ) ;
#47035 = DIRECTION ( 'NONE',  ( 0.000000000000000000, 0.000000000000000000, 1.000000000000000000 ) ) ;
#47037 = VERTEX_POINT ( 'NONE', #115884 ) ;
#47036 = CIRCLE ( 'NONE', #13560, 2.318304356886072615 ) ;
#47038 = DIRECTION ( 'NONE',  ( 0.000000000000000000, -0.9999939076577903929, 0.003490651415223739937 ) ) ;
#47039 = CARTESIAN_POINT ( 'NONE',  ( -6.250000000000021316, 12.50000000000000000, -5.737276932171712751 ) ) ;
#47040 = ORIENTED_EDGE ( 'NONE', *, *, #119769, .F. ) ;
#47041 = DIRECTION ( 'NONE',  ( -0.000000000000000000, -1.000000000000000000, -0.000000000000000000 ) ) ;
#47042 = CARTESIAN_POINT ( 'NONE',  ( 5.449999999999936229, 12.50000000000000000, -2.230156782645139391 ) ) ;
#47043 = AXIS2_PLACEMENT_3D ( 'NONE', #99978, #18823, #50237 ) ;
#47044 = ORIENTED_EDGE ( 'NONE', *, *, #41805, .T. ) ;
#47045 = DIRECTION ( 'NONE',  ( 0.000000000000000000, -0.000000000000000000, 1.000000000000000000 ) ) ;
#47046 = CARTESIAN_POINT ( 'NONE',  ( 9.399999999999915090, 2.500000000000000000, -4.776537180435977525 ) ) ;
#47047 = ORIENTED_EDGE ( 'NONE', *, *, #28012, .F. ) ;
#47048 = CARTESIAN_POINT ( 'NONE',  ( -4.200000000000025935, 2.500000000000000000, -0.1000000000000023925 ) ) ;
#47049 = ORIENTED_EDGE ( 'NONE', *, *, #62605, .T. ) ;
#47050 = EDGE_LOOP ( 'NONE', ( #33017, #48077 ) ) ;
#47051 = DIRECTION ( 'NONE',  ( 0.000000000000000000, -0.000000000000000000, 1.000000000000000000 ) ) ;
#47052 = VERTEX_POINT ( 'NONE', #14443 ) ;
#47053 = CARTESIAN_POINT ( 'NONE',  ( 3.299999999999944755, 12.50000000000000000, -2.385244779468109755E-15 ) ) ;
#47054 = FACE_OUTER_BOUND ( 'NONE', #7963, .T. ) ;
#47055 = VECTOR ( 'NONE', #53740, 1000.000000000000000 ) ;
#47056 = ADVANCED_FACE ( 'NONE', ( #74032 ), #35554, .T. ) ;
#47057 = ORIENTED_EDGE ( 'NONE', *, *, #32768, .F. ) ;
#47059 = CARTESIAN_POINT ( 'NONE',  ( 4.999999999999933387, 12.50000000000000000, 5.022947341949748790 ) ) ;
#47058 = CIRCLE ( 'NONE', #3147, 0.1000000000000002554 ) ;
#47060 = VERTEX_POINT ( 'NONE', #115207 ) ;
#47061 = DIRECTION ( 'NONE',  ( 0.000000000000000000, 1.000000000000000000, 0.000000000000000000 ) ) ;
#47062 = DIRECTION ( 'NONE',  ( 0.000000000000000000, 1.000000000000000000, 0.000000000000000000 ) ) ;
#47063 = CARTESIAN_POINT ( 'NONE',  ( -4.600000000000028955, 2.500000000000000000, -4.330127018922201643 ) ) ;
#47065 = ADVANCED_FACE ( 'NONE', ( #83215 ), #118882, .T. ) ;
#47064 = FACE_OUTER_BOUND ( 'NONE', #118439, .T. ) ;
#47066 = CARTESIAN_POINT ( 'NONE',  ( -3.550000000000028244, 12.50000000000000000, 2.446380397790835826 ) ) ;
#47067 = EDGE_CURVE ( 'NONE', #87160, #51388, #24287, .T. ) ;
#47068 = VERTEX_POINT ( 'NONE', #123135 ) ;
#47069 = EDGE_LOOP ( 'NONE', ( #3322, #110334 ) ) ;
#47070 = FACE_OUTER_BOUND ( 'NONE', #92097, .T. ) ;
#47071 = AXIS2_PLACEMENT_3D ( 'NONE', #99820, #79531, #10144 ) ;
#47072 = AXIS2_PLACEMENT_3D ( 'NONE', #74241, #85969, #23861 ) ;
#47073 = DIRECTION ( 'NONE',  ( -0.000000000000000000, -1.000000000000000000, -0.000000000000000000 ) ) ;
#47074 = EDGE_CURVE ( 'NONE', #76186, #125301, #121209, .T. ) ;
#47075 = CARTESIAN_POINT ( 'NONE',  ( 9.199999999999915801, 2.500000000000000000, 4.430127018922196847 ) ) ;
#47077 = ORIENTED_EDGE ( 'NONE', *, *, #97458, .T. ) ;
#47076 = VERTEX_POINT ( 'NONE', #105430 ) ;
#47078 = ADVANCED_FACE ( 'NONE', ( #23636 ), #63574, .T. ) ;
#47079 = EDGE_LOOP ( 'NONE', ( #18949, #40235 ) ) ;
#47080 = ADVANCED_FACE ( 'NONE', ( #13802 ), #25075, .T. ) ;
#47081 = DIRECTION ( 'NONE',  ( 0.000000000000000000, 1.000000000000000000, 0.000000000000000000 ) ) ;
#47082 = DIRECTION ( 'NONE',  ( -0.000000000000000000, -1.000000000000000000, -0.000000000000000000 ) ) ;
#47083 = FACE_OUTER_BOUND ( 'NONE', #12668, .T. ) ;
#47084 = APPLICATION_PROTOCOL_DEFINITION ( 'draft international standard', 'automotive_design', 1998, #119053 ) ;
#47085 = EDGE_CURVE ( 'NONE', #74025, #113934, #112906, .T. ) ;
#47086 = DIRECTION ( 'NONE',  ( 0.000000000000000000, 0.000000000000000000, 1.000000000000000000 ) ) ;
#47087 = LINE ( 'NONE', #48359, #4236 ) ;
#47088 = DIRECTION ( 'NONE',  ( 1.000000000000000000, 0.000000000000000000, 0.000000000000000000 ) ) ;
#47089 = CARTESIAN_POINT ( 'NONE',  ( 8.349999999999919709, 2.500000000000000000, 7.288010851410849256 ) ) ;
#47090 = DIRECTION ( 'NONE',  ( -0.000000000000000000, 1.000000000000000000, -0.000000000000000000 ) ) ;
#47091 = VECTOR ( 'NONE', #10509, 1000.000000000000000 ) ;
#47093 = EDGE_CURVE ( 'NONE', #122264, #70390, #71049, .T. ) ;
#47092 = CARTESIAN_POINT ( 'NONE',  ( 8.949999999999921130, 12.50000000000000000, -6.906693963081115939 ) ) ;
#47094 = ORIENTED_EDGE ( 'NONE', *, *, #116899, .F. ) ;
#47095 = CONICAL_SURFACE ( 'NONE', #76328, 0.09999999999999982514, 0.003490658503988666988 ) ;
#47096 = CIRCLE ( 'NONE', #95113, 0.06509327318403745899 ) ;
#47097 = DIRECTION ( 'NONE',  ( 0.000000000000000000, 1.000000000000000000, 0.000000000000000000 ) ) ;
#47098 = AXIS2_PLACEMENT_3D ( 'NONE', #96947, #45939, #106135 ) ;
#47099 = ORIENTED_EDGE ( 'NONE', *, *, #100441, .F. ) ;
#47100 = ORIENTED_EDGE ( 'NONE', *, *, #76978, .F. ) ;
#47101 = CARTESIAN_POINT ( 'NONE',  ( -7.700000000000016165, 12.50000000000000000, -3.918623584224389056 ) ) ;
#47102 = CARTESIAN_POINT ( 'NONE',  ( 12.49999999999990052, 2.500000000000000000, 0.6928203230275494784 ) ) ;
#47103 = CARTESIAN_POINT ( 'NONE',  ( 12.69999999999990159, 2.500000000000000000, 4.776537180435972196 ) ) ;
#47104 = CONICAL_SURFACE ( 'NONE', #128689, 0.1000000000000002554, 0.003490658503988666988 ) ;
#47105 = DIRECTION ( 'NONE',  ( 0.000000000000000000, 1.000000000000000000, 0.000000000000000000 ) ) ;
#47106 = VECTOR ( 'NONE', #20161, 1000.000000000000000 ) ;
#47108 = CARTESIAN_POINT ( 'NONE',  ( 185.1666666666666856, -6.668395609140176816, -3.850000000000003642 ) ) ;
#47107 = CIRCLE ( 'NONE', #72245, 0.06509327318403745899 ) ;
#47109 = CARTESIAN_POINT ( 'NONE',  ( 4.799999999999934097, 12.50000000000000000, 4.611443907251934426 ) ) ;
#47110 = LINE ( 'NONE', #35985, #50959 ) ;
#47111 = ORIENTED_EDGE ( 'NONE', *, *, #82872, .F. ) ;
#47112 = DIRECTION ( 'NONE',  ( 0.000000000000000000, -0.000000000000000000, 1.000000000000000000 ) ) ;
#47113 = AXIS2_PLACEMENT_3D ( 'NONE', #127307, #67718, #45525 ) ;
#47114 = CARTESIAN_POINT ( 'NONE',  ( 3.349999999999945466, 12.50000000000000000, -2.792790559304616504 ) ) ;
#47115 = AXIS2_PLACEMENT_3D ( 'NONE', #60001, #11516, #60638 ) ;
#47116 = ORIENTED_EDGE ( 'NONE', *, *, #3429, .F. ) ;
#47117 = VERTEX_POINT ( 'NONE', #24933 ) ;
#47118 = EDGE_LOOP ( 'NONE', ( #50988, #72353 ) ) ;
#47119 = ORIENTED_EDGE ( 'NONE', *, *, #126252, .F. ) ;
#47120 = FACE_OUTER_BOUND ( 'NONE', #41443, .T. ) ;
#47121 = DIRECTION ( 'NONE',  ( 0.000000000000000000, 0.000000000000000000, 1.000000000000000000 ) ) ;
#47122 = ORIENTED_EDGE ( 'NONE', *, *, #30073, .F. ) ;
#47123 = LINE ( 'NONE', #15694, #104921 ) ;
#47124 = EDGE_CURVE ( 'NONE', #81821, #98256, #112625, .T. ) ;
#47125 = CARTESIAN_POINT ( 'NONE',  ( 17.50000000000000000, 2.750000000000000000, -3.432456362931489036 ) ) ;
#47126 = DIRECTION ( 'NONE',  ( 0.000000000000000000, 1.000000000000000000, 0.000000000000000000 ) ) ;
#47127 = ORIENTED_EDGE ( 'NONE', *, *, #112971, .F. ) ;
#47128 = CARTESIAN_POINT ( 'NONE',  ( -2.499999999999996447, 12.50000000000000000, 4.330127018922196314 ) ) ;
#47129 = AXIS2_PLACEMENT_3D ( 'NONE', #19667, #110615, #88380 ) ;
#47131 = ADVANCED_FACE ( 'NONE', ( #37969 ), #49102, .T. ) ;
#47130 = CARTESIAN_POINT ( 'NONE',  ( 5.849999999999932143, 2.500000000000000000, 2.165063509461097713 ) ) ;
#47132 = ORIENTED_EDGE ( 'NONE', *, *, #95567, .F. ) ;
#47133 = EDGE_LOOP ( 'NONE', ( #15212, #109130, #29364, #112607 ) ) ;
#47134 = VERTEX_POINT ( 'NONE', #96231 ) ;
#47135 = PLANE ( 'NONE',  #15404 ) ;
#47136 = VECTOR ( 'NONE', #107401, 1000.000000000000000 ) ;
#47137 = FACE_OUTER_BOUND ( 'NONE', #43366, .T. ) ;
#47138 = ORIENTED_EDGE ( 'NONE', *, *, #25458, .F. ) ;
#47139 = DIRECTION ( 'NONE',  ( 0.000000000000000000, 0.000000000000000000, 1.000000000000000000 ) ) ;
#47140 = DIRECTION ( 'NONE',  ( -0.000000000000000000, 1.000000000000000000, -0.000000000000000000 ) ) ;
#47141 = DIRECTION ( 'NONE',  ( 0.000000000000000000, 0.000000000000000000, -1.000000000000000000 ) ) ;
#47142 = LINE ( 'NONE', #74656, #121422 ) ;
#47143 = AXIS2_PLACEMENT_3D ( 'NONE', #40726, #19779, #121189 ) ;
#47144 = ORIENTED_EDGE ( 'NONE', *, *, #79134, .F. ) ;
#47145 = CARTESIAN_POINT ( 'NONE',  ( 8.949999999999915801, 12.50000000000000000, -1.818653347947326138 ) ) ;
#47146 = VECTOR ( 'NONE', #4995, 1000.000000000000000 ) ;
#47147 = EDGE_LOOP ( 'NONE', ( #20605, #56954, #17708, #52181 ) ) ;
#47148 = ORIENTED_EDGE ( 'NONE', *, *, #96543, .F. ) ;
#47149 = VERTEX_POINT ( 'NONE', #106070 ) ;
#47150 = CARTESIAN_POINT ( 'NONE',  ( 4.999999999999971578, 2.500000000000000000, -2.276824562219559311E-15 ) ) ;
#47151 = FACE_BOUND ( 'NONE', #34900, .T. ) ;
#47152 = DIRECTION ( 'NONE',  ( 0.000000000000000000, 0.000000000000000000, -1.000000000000000000 ) ) ;
#47153 = DIRECTION ( 'NONE',  ( 0.000000000000000000, -0.000000000000000000, 1.000000000000000000 ) ) ;
#47154 = CARTESIAN_POINT ( 'NONE',  ( 3.299999999999944755, 2.500000000000000000, -4.330127018922201643 ) ) ;
#47155 = EDGE_CURVE ( 'NONE', #15933, #100718, #29004, .T. ) ;
#47156 = AXIS2_PLACEMENT_3D ( 'NONE', #63102, #84021, #93856 ) ;
#47157 = CONICAL_SURFACE ( 'NONE', #126578, 0.09999999999999982514, 0.003490658503988666988 ) ;
#47158 = ORIENTED_EDGE ( 'NONE', *, *, #52007, .T. ) ;
#47159 = DIRECTION ( 'NONE',  ( 0.000000000000000000, 0.000000000000000000, -1.000000000000000000 ) ) ;
#47160 = CARTESIAN_POINT ( 'NONE',  ( 187.5000000000000000, 1.500000000000000000, -6.000000000000000000 ) ) ;
#47161 = CARTESIAN_POINT ( 'NONE',  ( -0.4000000000000339950, 2.500000000000000000, 0.6928203230275518099 ) ) ;
#47162 = CARTESIAN_POINT ( 'NONE',  ( 4.149999999999939959, 2.500000000000000000, 2.857883832488649301 ) ) ;
#47163 = VERTEX_POINT ( 'NONE', #46492 ) ;
#47164 = ADVANCED_FACE ( 'NONE', ( #38645 ), #98222, .T. ) ;
#47165 = PLANE ( 'NONE',  #115912 ) ;
#47166 = LINE ( 'NONE', #7867, #37006 ) ;
#47167 = CIRCLE ( 'NONE', #120329, 0.06509327318403745899 ) ;
#47168 = ORIENTED_EDGE ( 'NONE', *, *, #59727, .F. ) ;
#47169 = EDGE_CURVE ( 'NONE', #37316, #59852, #79471, .T. ) ;
#47170 = CARTESIAN_POINT ( 'NONE',  ( -9.150000000000011013, 2.500000000000000000, -5.802370205355744659 ) ) ;
#47172 = ADVANCED_FACE ( 'NONE', ( #107996 ), #127007, .T. ) ;
#47171 = FACE_OUTER_BOUND ( 'NONE', #102773, .T. ) ;
#47173 = CIRCLE ( 'NONE', #126597, 0.1000000000000002554 ) ;
#47174 = FACE_BOUND ( 'NONE', #80759, .T. ) ;
#47175 = DIRECTION ( 'NONE',  ( -0.000000000000000000, 1.000000000000000000, -0.000000000000000000 ) ) ;
#47176 = CIRCLE ( 'NONE', #42995, 0.06509327318403745899 ) ;
#47177 = EDGE_LOOP ( 'NONE', ( #31229, #123086 ) ) ;
#47178 = DIRECTION ( 'NONE',  ( -0.000000000000000000, -1.000000000000000000, -0.000000000000000000 ) ) ;
#47179 = EDGE_CURVE ( 'NONE', #64350, #101033, #58544, .T. ) ;
#47180 = CONICAL_SURFACE ( 'NONE', #111926, 0.1000000000000002554, 0.003490658503988666988 ) ;
#47181 = EDGE_LOOP ( 'NONE', ( #19351, #38847, #91971, #65506 ) ) ;
#47182 = ORIENTED_EDGE ( 'NONE', *, *, #9351, .F. ) ;
#47183 = CARTESIAN_POINT ( 'NONE',  ( 6.899999999999928413, 2.500000000000000000, 4.576537180435972019 ) ) ;
#47184 = EDGE_CURVE ( 'NONE', #63096, #907, #46016, .T. ) ;
#47185 = CARTESIAN_POINT ( 'NONE',  ( 186.6250000000000284, -8.891194145520236347, -1.633285867636356693E-15 ) ) ;
#47186 = ORIENTED_EDGE ( 'NONE', *, *, #110364, .T. ) ;
#47187 = CARTESIAN_POINT ( 'NONE',  ( 185.3802083336747444, 4.367472073101515306, 7.564683531250000925 ) ) ;
#47188 = CARTESIAN_POINT ( 'NONE',  ( 88.00000000000001421, 1.004210375300829477E-15, 8.199999999999999289 ) ) ;
#47189 = DIRECTION ( 'NONE',  ( 0.000000000000000000, 0.000000000000000000, 1.000000000000000000 ) ) ;
#47190 = CONICAL_SURFACE ( 'NONE', #114087, 0.1000000000000002554, 0.003490658503988666988 ) ;
#47191 = CARTESIAN_POINT ( 'NONE',  ( 185.5729166673494603, 4.445597072760072876, -7.700000000000080114 ) ) ;
#47192 = CIRCLE ( 'NONE', #101570, 3.000000000000000444 ) ;
#47193 = AXIS2_PLACEMENT_3D ( 'NONE', #51245, #58485, #20481 ) ;
#47194 = VERTEX_POINT ( 'NONE', #36700 ) ;
#47195 = AXIS2_PLACEMENT_3D ( 'NONE', #10038, #858, #91173 ) ;
#47196 = DIRECTION ( 'NONE',  ( 0.000000000000000000, 1.000000000000000000, 0.000000000000000000 ) ) ;
#47197 = CARTESIAN_POINT ( 'NONE',  ( 3.099999999999945466, 12.50000000000000000, 0.2813168883297361700 ) ) ;
#47198 = DIRECTION ( 'NONE',  ( 0.000000000000000000, -0.000000000000000000, 1.000000000000000000 ) ) ;
#47199 = CONICAL_SURFACE ( 'NONE', #1127, 0.09999999999999982514, 0.003490658503988666988 ) ;
#47200 = DIRECTION ( 'NONE',  ( -0.000000000000000000, 1.000000000000000000, -0.000000000000000000 ) ) ;
#47201 = VERTEX_POINT ( 'NONE', #76612 ) ;
#47202 = DIRECTION ( 'NONE',  ( 0.000000000000000000, 0.000000000000000000, -1.000000000000000000 ) ) ;
#47203 = ORIENTED_EDGE ( 'NONE', *, *, #113241, .F. ) ;
#47204 = DIRECTION ( 'NONE',  ( 0.000000000000000000, -0.000000000000000000, 1.000000000000000000 ) ) ;
#47205 = CARTESIAN_POINT ( 'NONE',  ( 0.8499999999999550138, 2.500000000000000000, -5.802370205355749988 ) ) ;
#47206 = ORIENTED_EDGE ( 'NONE', *, *, #72453, .F. ) ;
#47207 = PLANE ( 'NONE',  #88765 ) ;
#47208 = DIRECTION ( 'NONE',  ( 0.000000000000000000, 1.000000000000000000, 0.000000000000000000 ) ) ;
#47209 = EDGE_CURVE ( 'NONE', #48633, #69160, #47802, .T. ) ;
#47210 = DIRECTION ( 'NONE',  ( 0.000000000000000000, 0.000000000000000000, 1.000000000000000000 ) ) ;
#47211 = CARTESIAN_POINT ( 'NONE',  ( 9.799999999999917222, 12.50000000000000000, 0.3464101615137735735 ) ) ;
#47212 = ORIENTED_EDGE ( 'NONE', *, *, #47531, .F. ) ;
#47213 = DIRECTION ( 'NONE',  ( 0.000000000000000000, 1.000000000000000000, 0.000000000000000000 ) ) ;
#47214 = CARTESIAN_POINT ( 'NONE',  ( -9.800000000000007816, 12.50000000000000000, -3.983716857408421852 ) ) ;
#47215 = CARTESIAN_POINT ( 'NONE',  ( 184.7343750003414016, 8.734944146203032389, 5.348610694689227483E-16 ) ) ;
#47216 = DIRECTION ( 'NONE',  ( 0.000000000000000000, 0.000000000000000000, -1.000000000000000000 ) ) ;
#47217 = AXIS2_PLACEMENT_3D ( 'NONE', #43193, #13695, #123028 ) ;
#47218 = DIRECTION ( 'NONE',  ( 0.000000000000000000, -0.000000000000000000, 1.000000000000000000 ) ) ;
#47219 = EDGE_CURVE ( 'NONE', #20030, #123959, #62743, .T. ) ;
#47220 = EDGE_LOOP ( 'NONE', ( #17744, #96005 ) ) ;
#47221 = ORIENTED_EDGE ( 'NONE', *, *, #45289, .F. ) ;
#47222 = CARTESIAN_POINT ( 'NONE',  ( -6.900000000000015454, 12.50000000000000000, 3.983716857408420076 ) ) ;
#47223 = ORIENTED_EDGE ( 'NONE', *, *, #7568, .F. ) ;
#47224 = CARTESIAN_POINT ( 'NONE',  ( -0.6500000000000403233, 2.500000000000000000, 1.718653347947321386 ) ) ;
#47225 = EDGE_CURVE ( 'NONE', #88700, #31372, #23020, .T. ) ;
#47227 = ORIENTED_EDGE ( 'NONE', *, *, #101355, .T. ) ;
#47226 = ORIENTED_EDGE ( 'NONE', *, *, #20613, .T. ) ;
#47228 = CIRCLE ( 'NONE', #120383, 0.1000000000000000472 ) ;
#47229 = EDGE_LOOP ( 'NONE', ( #32183, #64837, #24363, #51894 ) ) ;
#47230 = EDGE_CURVE ( 'NONE', #54992, #48724, #64775, .T. ) ;
#47231 = CARTESIAN_POINT ( 'NONE',  ( 13.54999999999989591, 12.50000000000000000, -1.753560074763288679 ) ) ;
#47232 = CIRCLE ( 'NONE', #49388, 0.06509327318403745899 ) ;
#47233 = EDGE_CURVE ( 'NONE', #45762, #39409, #102158, .T. ) ;
#47234 = VECTOR ( 'NONE', #55233, 1000.000000000000000 ) ;
#47235 = DIRECTION ( 'NONE',  ( 0.000000000000000000, 0.000000000000000000, 1.000000000000000000 ) ) ;
#47236 = DIRECTION ( 'NONE',  ( 0.000000000000000000, 1.000000000000000000, 0.000000000000000000 ) ) ;
#47237 = PRESENTATION_STYLE_ASSIGNMENT (( #107432 ) ) ;
#47238 = EDGE_CURVE ( 'NONE', #35493, #88394, #24, .T. ) ;
#47239 = DIRECTION ( 'NONE',  ( 0.000000000000000000, 0.000000000000000000, 1.000000000000000000 ) ) ;
#47240 = DIRECTION ( 'NONE',  ( 0.000000000000000000, 0.000000000000000000, 1.000000000000000000 ) ) ;
#47241 = DIRECTION ( 'NONE',  ( 0.000000000000000000, 0.000000000000000000, 1.000000000000000000 ) ) ;
#47242 = ORIENTED_EDGE ( 'NONE', *, *, #68957, .T. ) ;
#47244 = EDGE_CURVE ( 'NONE', #67980, #16778, #35270, .T. ) ;
#47243 = DIRECTION ( 'NONE',  ( 0.000000000000000000, 0.000000000000000000, 1.000000000000000000 ) ) ;
#47245 = ORIENTED_EDGE ( 'NONE', *, *, #17769, .F. ) ;
#47246 = AXIS2_PLACEMENT_3D ( 'NONE', #35400, #37342, #104749 ) ;
#47247 = ADVANCED_FACE ( 'NONE', ( #27482 ), #91692, .T. ) ;
#47248 = EDGE_LOOP ( 'NONE', ( #53024, #85382 ) ) ;
#47249 = VERTEX_POINT ( 'NONE', #8491 ) ;
#47250 = ORIENTED_EDGE ( 'NONE', *, *, #24422, .T. ) ;
#47252 = CONICAL_SURFACE ( 'NONE', #53503, 0.1000000000000002554, 0.003490658503988666988 ) ;
#47251 = CONICAL_SURFACE ( 'NONE', #49317, 0.1000000000000002554, 0.003490658503988666988 ) ;
#47253 = CARTESIAN_POINT ( 'NONE',  ( 10.39999999999991509, 2.500000000000000000, 0.6928203230275494784 ) ) ;
#47254 = EDGE_LOOP ( 'NONE', ( #8152, #78123 ) ) ;
#47255 = VERTEX_POINT ( 'NONE', #28809 ) ;
#47257 = VECTOR ( 'NONE', #58304, 1000.000000000000000 ) ;
#47256 = DIRECTION ( 'NONE',  ( -0.000000000000000000, 1.000000000000000000, -0.000000000000000000 ) ) ;
#47258 = DIRECTION ( 'NONE',  ( 0.000000000000000000, 1.000000000000000000, 0.000000000000000000 ) ) ;
#47259 = AXIS2_PLACEMENT_3D ( 'NONE', #16420, #95659, #113359 ) ;
#47260 = DIRECTION ( 'NONE',  ( 0.000000000000000000, 0.000000000000000000, 1.000000000000000000 ) ) ;
#47261 = DIRECTION ( 'NONE',  ( -0.000000000000000000, -1.000000000000000000, -0.000000000000000000 ) ) ;
#47262 = DIRECTION ( 'NONE',  ( -0.000000000000000000, -1.000000000000000000, -0.000000000000000000 ) ) ;
#47263 = ORIENTED_EDGE ( 'NONE', *, *, #92304, .T. ) ;
#47264 = FACE_OUTER_BOUND ( 'NONE', #77693, .T. ) ;
#47265 = VERTEX_POINT ( 'NONE', #68713 ) ;
#47266 = CARTESIAN_POINT ( 'NONE',  ( -9.150000000000011013, 12.50000000000000000, -5.802370205355744659 ) ) ;
#47267 = VERTEX_POINT ( 'NONE', #108640 ) ;
#47268 = FACE_OUTER_BOUND ( 'NONE', #62958, .T. ) ;
#47269 = VERTEX_POINT ( 'NONE', #98818 ) ;
#47270 = ORIENTED_EDGE ( 'NONE', *, *, #45747, .T. ) ;
#47271 = CARTESIAN_POINT ( 'NONE',  ( -2.050000000000032685, 2.500000000000000000, -2.265063509461101798 ) ) ;
#47272 = LINE ( 'NONE', #5396, #21357 ) ;
#47273 = CIRCLE ( 'NONE', #76512, 0.06509327318403745899 ) ;
#47274 = DIRECTION ( 'NONE',  ( 0.000000000000000000, 1.000000000000000000, 0.000000000000000000 ) ) ;
#47275 = EDGE_CURVE ( 'NONE', #81286, #80090, #9155, .T. ) ;
#47277 = FACE_OUTER_BOUND ( 'NONE', #115545, .T. ) ;
#47276 = CIRCLE ( 'NONE', #55665, 0.06509327318403741736 ) ;
#47278 = FACE_OUTER_BOUND ( 'NONE', #42903, .T. ) ;
#47279 = ORIENTED_EDGE ( 'NONE', *, *, #35470, .F. ) ;
#47280 = DIRECTION ( 'NONE',  ( -0.000000000000000000, -1.000000000000000000, -0.000000000000000000 ) ) ;
#47281 = DIRECTION ( 'NONE',  ( 0.000000000000000000, 0.000000000000000000, 1.000000000000000000 ) ) ;
#47282 = DIRECTION ( 'NONE',  ( 0.000000000000000000, -0.000000000000000000, 1.000000000000000000 ) ) ;
#47283 = FACE_OUTER_BOUND ( 'NONE', #91441, .T. ) ;
#47285 = AXIS2_PLACEMENT_3D ( 'NONE', #21404, #22073, #2387 ) ;
#47284 = CONICAL_SURFACE ( 'NONE', #120434, 0.1000000000000000472, 0.003490658503988666988 ) ;
#47287 = EDGE_CURVE ( 'NONE', #120157, #32665, #68695, .T. ) ;
#47286 = DIRECTION ( 'NONE',  ( -0.000000000000000000, 1.000000000000000000, -0.000000000000000000 ) ) ;
#47288 = ORIENTED_EDGE ( 'NONE', *, *, #19, .T. ) ;
#47289 = ORIENTED_EDGE ( 'NONE', *, *, #27353, .T. ) ;
#47290 = CARTESIAN_POINT ( 'NONE',  ( -1.050000000000038680, 2.500000000000000000, 6.841600689897072485 ) ) ;
#47291 = EDGE_LOOP ( 'NONE', ( #97792, #33771, #37740, #77419 ) ) ;
#47292 = CARTESIAN_POINT ( 'NONE',  ( 5.849999999999935696, 12.50000000000000000, -7.122917578226816815 ) ) ;
#47293 = CARTESIAN_POINT ( 'NONE',  ( 7.499999999999927169, 2.500000000000000000, 3.637306695894644726 ) ) ;
#47294 = VECTOR ( 'NONE', #115964, 1000.000000000000000 ) ;
#47295 = VERTEX_POINT ( 'NONE', #31393 ) ;
#47296 = CARTESIAN_POINT ( 'NONE',  ( 185.5000000000000000, 0.000000000000000000, 7.700000000000000178 ) ) ;
#47297 = FACE_OUTER_BOUND ( 'NONE', #3111, .T. ) ;
#47298 = DIRECTION ( 'NONE',  ( -4.274815082592931898E-19, -0.9999939076577903929, -0.003490651415223739937 ) ) ;
#47299 = DIRECTION ( 'NONE',  ( 0.000000000000000000, 0.000000000000000000, -1.000000000000000000 ) ) ;
#47300 = ORIENTED_EDGE ( 'NONE', *, *, #51693, .T. ) ;
#47301 = CARTESIAN_POINT ( 'NONE',  ( -9.999999999999969802, 2.500000000000000000, 4.230127018922196669 ) ) ;
#47302 = CARTESIAN_POINT ( 'NONE',  ( 149.5981739382431783, 2.500000000000000000, 1.703575533167231537 ) ) ;
#47303 = VERTEX_POINT ( 'NONE', #90944 ) ;
#47304 = DIRECTION ( 'NONE',  ( 0.000000000000000000, 1.000000000000000000, 0.000000000000000000 ) ) ;
#47305 = AXIS2_PLACEMENT_3D ( 'NONE', #111086, #111763, #43050 ) ;
#47306 = DIRECTION ( 'NONE',  ( 0.000000000000000000, -0.9999939076577903929, 0.003490651415223739937 ) ) ;
#47307 = DIRECTION ( 'NONE',  ( 0.000000000000000000, -0.000000000000000000, 1.000000000000000000 ) ) ;
#47308 = ORIENTED_EDGE ( 'NONE', *, *, #54442, .T. ) ;
#47309 = FACE_OUTER_BOUND ( 'NONE', #99359, .T. ) ;
#47310 = CIRCLE ( 'NONE', #34806, 0.09999999999999999167 ) ;
#47311 = EDGE_LOOP ( 'NONE', ( #2077, #75655, #23505, #30457 ) ) ;
#47312 = CARTESIAN_POINT ( 'NONE',  ( -5.400000000000019895, 12.50000000000000000, 3.637306695894644726 ) ) ;
#47313 = FACE_OUTER_BOUND ( 'NONE', #17139, .T. ) ;
#47314 = AXIS2_PLACEMENT_3D ( 'NONE', #99354, #1139, #61360 ) ;
#47315 = DIRECTION ( 'NONE',  ( 0.000000000000000000, 1.000000000000000000, 0.000000000000000000 ) ) ;
#47316 = VECTOR ( 'NONE', #108177, 1000.000000000000000 ) ;
#47317 = ORIENTED_EDGE ( 'NONE', *, *, #19884, .F. ) ;
#47318 = EDGE_CURVE ( 'NONE', #86156, #37898, #125144, .T. ) ;
#47319 = LINE ( 'NONE', #118623, #63519 ) ;
#47320 = CIRCLE ( 'NONE', #107955, 0.06509327318403743123 ) ;
#47321 = DIRECTION ( 'NONE',  ( 0.000000000000000000, -0.000000000000000000, 1.000000000000000000 ) ) ;
#47322 = VERTEX_POINT ( 'NONE', #50368 ) ;
#47323 = EDGE_CURVE ( 'NONE', #92653, #72025, #62461, .T. ) ;
#47324 = CARTESIAN_POINT ( 'NONE',  ( -10.20000000000000639, 2.500000000000000000, -4.083716857408422385 ) ) ;
#47325 = ADVANCED_FACE ( 'NONE', ( #32044 ), #102250, .T. ) ;
#47326 = VERTEX_POINT ( 'NONE', #100122 ) ;
#47328 = VECTOR ( 'NONE', #67916, 1000.000000000000000 ) ;
#47327 = FACE_OUTER_BOUND ( 'NONE', #104754, .T. ) ;
#47330 = AXIS2_PLACEMENT_3D ( 'NONE', #7906, #128362, #127688 ) ;
#47329 = AXIS2_PLACEMENT_3D ( 'NONE', #39204, #109856, #20829 ) ;
#47331 = ORIENTED_EDGE ( 'NONE', *, *, #46927, .T. ) ;
#47332 = DIRECTION ( 'NONE',  ( -0.000000000000000000, -1.000000000000000000, -0.000000000000000000 ) ) ;
#47333 = DIRECTION ( 'NONE',  ( -4.274815082592931898E-19, -0.9999939076577903929, -0.003490651415223739937 ) ) ;
#47334 = EDGE_CURVE ( 'NONE', #71492, #109003, #70022, .T. ) ;
#47335 = EDGE_CURVE ( 'NONE', #702, #89145, #6079, .T. ) ;
#47336 = ORIENTED_EDGE ( 'NONE', *, *, #11686, .F. ) ;
#47337 = ORIENTED_EDGE ( 'NONE', *, *, #4285, .T. ) ;
#47338 = EDGE_CURVE ( 'NONE', #109850, #100401, #129375, .T. ) ;
#47339 = LINE ( 'NONE', #106875, #1720 ) ;
#47340 = CARTESIAN_POINT ( 'NONE',  ( 6.049999999999932321, 2.500000000000000000, -1.818653347947326138 ) ) ;
#47341 = VERTEX_POINT ( 'NONE', #59581 ) ;
#47342 = LINE ( 'NONE', #87239, #21700 ) ;
#47343 = CARTESIAN_POINT ( 'NONE',  ( -11.24999999999996270, 12.50000000000000000, 2.165063509461097713 ) ) ;
#47344 = DIRECTION ( 'NONE',  ( 0.000000000000000000, 1.000000000000000000, 0.000000000000000000 ) ) ;
#47345 = DIRECTION ( 'NONE',  ( 0.000000000000000000, -0.9999939076577903929, 0.003490651415223739937 ) ) ;
#47346 = DIRECTION ( 'NONE',  ( -0.000000000000000000, 1.000000000000000000, -0.000000000000000000 ) ) ;
#47347 = DIRECTION ( 'NONE',  ( 0.000000000000000000, 0.000000000000000000, -1.000000000000000000 ) ) ;
#47348 = ORIENTED_EDGE ( 'NONE', *, *, #2582, .T. ) ;
#47349 = ORIENTED_EDGE ( 'NONE', *, *, #83461, .T. ) ;
#47350 = ORIENTED_EDGE ( 'NONE', *, *, #82506, .T. ) ;
#47351 = ORIENTED_EDGE ( 'NONE', *, *, #80209, .F. ) ;
#47352 = PLANE ( 'NONE',  #66240 ) ;
#47353 = CARTESIAN_POINT ( 'NONE',  ( -13.74999999999998934, 12.50000000000000000, -1.472243186433547901 ) ) ;
#47354 = LINE ( 'NONE', #127210, #92864 ) ;
#47355 = ORIENTED_EDGE ( 'NONE', *, *, #83799, .F. ) ;
#47356 = FACE_BOUND ( 'NONE', #69636, .T. ) ;
#47357 = DIRECTION ( 'NONE',  ( 0.000000000000000000, 0.000000000000000000, 1.000000000000000000 ) ) ;
#47358 = DIRECTION ( 'NONE',  ( 0.000000000000000000, 1.000000000000000000, 0.000000000000000000 ) ) ;
#47359 = DIRECTION ( 'NONE',  ( 0.000000000000000000, -0.000000000000000000, 1.000000000000000000 ) ) ;
#47360 = CONICAL_SURFACE ( 'NONE', #39067, 0.09999999999999999167, 0.003490658503988666988 ) ;
#47361 = LINE ( 'NONE', #27703, #99392 ) ;
#47362 = CARTESIAN_POINT ( 'NONE',  ( -12.89999999999999147, 2.500000000000000000, 1.843143693225357538E-15 ) ) ;
#47363 = CARTESIAN_POINT ( 'NONE',  ( -2.700000000000030820, 2.500000000000000000, 0.3464101615137735735 ) ) ;
#47364 = CARTESIAN_POINT ( 'NONE',  ( 1.649999999999951061, 2.500000000000000000, -6.495190528383302464 ) ) ;
#47365 = LINE ( 'NONE', #29026, #91042 ) ;
#47366 = DIRECTION ( 'NONE',  ( -0.000000000000000000, 1.000000000000000000, -0.000000000000000000 ) ) ;
#47367 = DIRECTION ( 'NONE',  ( 0.000000000000000000, 0.000000000000000000, -1.000000000000000000 ) ) ;
#47369 = CIRCLE ( 'NONE', #20266, 0.1000000000000000472 ) ;
#47368 = AXIS2_PLACEMENT_3D ( 'NONE', #21703, #91721, #19085 ) ;
#47370 = EDGE_LOOP ( 'NONE', ( #34859, #95387, #14680, #28017 ) ) ;
#47371 = ORIENTED_EDGE ( 'NONE', *, *, #118115, .T. ) ;
#47372 = ORIENTED_EDGE ( 'NONE', *, *, #128245, .F. ) ;
#47373 = ORIENTED_EDGE ( 'NONE', *, *, #80724, .F. ) ;
#47374 = LINE ( 'NONE', #39512, #60182 ) ;
#47375 = ADVANCED_FACE ( 'NONE', ( #1271 ), #41636, .T. ) ;
#47376 = DIRECTION ( 'NONE',  ( 0.000000000000000000, 1.000000000000000000, 0.000000000000000000 ) ) ;
#47377 = EDGE_CURVE ( 'NONE', #87449, #113705, #1906, .T. ) ;
#47379 = ORIENTED_EDGE ( 'NONE', *, *, #70974, .T. ) ;
#47378 = VERTEX_POINT ( 'NONE', #30757 ) ;
#47380 = ORIENTED_EDGE ( 'NONE', *, *, #55927, .T. ) ;
#47381 = EDGE_CURVE ( 'NONE', #19267, #82725, #79827, .T. ) ;
#47382 = DIRECTION ( 'NONE',  ( 0.000000000000000000, 1.000000000000000000, 0.000000000000000000 ) ) ;
#47384 = AXIS2_PLACEMENT_3D ( 'NONE', #45881, #125697, #53756 ) ;
#47383 = AXIS2_PLACEMENT_3D ( 'NONE', #100242, #121162, #41336 ) ;
#47385 = AXIS2_PLACEMENT_3D ( 'NONE', #87625, #85698, #75237 ) ;
#47386 = DIRECTION ( 'NONE',  ( 0.000000000000000000, 1.000000000000000000, 0.000000000000000000 ) ) ;
#47387 = CARTESIAN_POINT ( 'NONE',  ( -12.89999999999999147, 12.50000000000000000, 0.06509327318403926310 ) ) ;
#47388 = EDGE_CURVE ( 'NONE', #58176, #116703, #52083, .T. ) ;
#47389 = CARTESIAN_POINT ( 'NONE',  ( 6.899999999999928413, 2.500000000000000000, -4.576537180435977348 ) ) ;
#47390 = ADVANCED_FACE ( 'NONE', ( #49747 ), #111205, .T. ) ;
#47391 = CARTESIAN_POINT ( 'NONE',  ( -2.300000000000033573, 2.500000000000000000, 0.2464101615137735679 ) ) ;
#47392 = DIRECTION ( 'NONE',  ( 0.000000000000000000, 1.000000000000000000, 0.000000000000000000 ) ) ;
#47393 = ORIENTED_EDGE ( 'NONE', *, *, #113680, .T. ) ;
#47395 = ADVANCED_FACE ( 'NONE', ( #111877 ), #114753, .T. ) ;
#47394 = DIRECTION ( 'NONE',  ( 0.000000000000000000, 0.000000000000000000, -1.000000000000000000 ) ) ;
#47396 = ORIENTED_EDGE ( 'NONE', *, *, #124057, .F. ) ;
#47397 = EDGE_CURVE ( 'NONE', #44028, #114232, #52307, .T. ) ;
#47398 = ORIENTED_EDGE ( 'NONE', *, *, #54716, .T. ) ;
#47399 = ORIENTED_EDGE ( 'NONE', *, *, #87683, .F. ) ;
#47400 = PLANE ( 'NONE',  #96428 ) ;
#47401 = ORIENTED_EDGE ( 'NONE', *, *, #55940, .T. ) ;
#47402 = AXIS2_PLACEMENT_3D ( 'NONE', #13546, #71844, #3731 ) ;
#47403 = ORIENTED_EDGE ( 'NONE', *, *, #54719, .T. ) ;
#47404 = ADVANCED_FACE ( 'NONE', ( #100742 ), #12375, .T. ) ;
#47406 = DIRECTION ( 'NONE',  ( 0.000000000000000000, 1.000000000000000000, 0.000000000000000000 ) ) ;
#47405 = VECTOR ( 'NONE', #68278, 1000.000000000000000 ) ;
#47407 = CARTESIAN_POINT ( 'NONE',  ( -1.050000000000037348, 12.50000000000000000, -6.841600689897078702 ) ) ;
#47409 = CIRCLE ( 'NONE', #105883, 0.06509327318403745899 ) ;
#47408 = DIRECTION ( 'NONE',  ( -4.274815082592931898E-19, -0.9999939076577903929, -0.003490651415223739937 ) ) ;
#47410 = CARTESIAN_POINT ( 'NONE',  ( -11.89999999999999680, 12.50000000000000000, -0.3464101615137741841 ) ) ;
#47411 = CARTESIAN_POINT ( 'NONE',  ( 0.3999999999999555023, 2.500000000000000000, 4.330127018922196314 ) ) ;
#47412 = VECTOR ( 'NONE', #114316, 1000.000000000000000 ) ;
#47413 = VERTEX_POINT ( 'NONE', #20267 ) ;
#47415 = VECTOR ( 'NONE', #54414, 1000.000000000000000 ) ;
#47414 = CARTESIAN_POINT ( 'NONE',  ( -14.39999999999998614, 2.500000000000000000, 0.3464101615137758494 ) ) ;
#47416 = EDGE_LOOP ( 'NONE', ( #122073, #63840, #34114, #65978 ) ) ;
#47417 = AXIS2_PLACEMENT_3D ( 'NONE', #109, #30250, #59713 ) ;
#47418 = CARTESIAN_POINT ( 'NONE',  ( 186.0000000000000000, 0.000000000000000000, 7.700000000000000178 ) ) ;
#47419 = VERTEX_POINT ( 'NONE', #20911 ) ;
#47420 = CARTESIAN_POINT ( 'NONE',  ( 9.999999999999952038, 12.50000000000000000, -2.276824562219559311E-15 ) ) ;
#47421 = CARTESIAN_POINT ( 'NONE',  ( -14.99999999999998401, 12.50000000000000000, 0.6928203230275518099 ) ) ;
#47422 = VERTEX_POINT ( 'NONE', #60839 ) ;
#47423 = DIRECTION ( 'NONE',  ( -0.000000000000000000, 1.000000000000000000, -0.000000000000000000 ) ) ;
#47424 = CIRCLE ( 'NONE', #124776, 0.09999999999999982514 ) ;
#47425 = CARTESIAN_POINT ( 'NONE',  ( -10.20000000000000462, 2.500000000000000000, -4.776537180435973085 ) ) ;
#47426 = ORIENTED_EDGE ( 'NONE', *, *, #111922, .F. ) ;
#47427 = AXIS2_PLACEMENT_3D ( 'NONE', #91427, #21391, #71136 ) ;
#47429 = CONICAL_SURFACE ( 'NONE', #120573, 0.09999999999999982514, 0.003490658503988666988 ) ;
#47428 = AXIS2_PLACEMENT_3D ( 'NONE', #120800, #50776, #13410 ) ;
#47430 = CARTESIAN_POINT ( 'NONE',  ( -4.200000000000025935, 2.500000000000000000, 0.09999999999999761857 ) ) ;
#47431 = ORIENTED_EDGE ( 'NONE', *, *, #120501, .T. ) ;
#47432 = ORIENTED_EDGE ( 'NONE', *, *, #108262, .T. ) ;
#47433 = DIRECTION ( 'NONE',  ( -0.000000000000000000, -1.000000000000000000, -0.000000000000000000 ) ) ;
#47434 = DIRECTION ( 'NONE',  ( -4.274815082592931898E-19, -0.9999939076577903929, -0.003490651415223739937 ) ) ;
#47435 = CARTESIAN_POINT ( 'NONE',  ( 187.0885416670080872, -6.551208109652273848, -3.782341765625003571 ) ) ;
#47436 = DIRECTION ( 'NONE',  ( 0.000000000000000000, -0.000000000000000000, 1.000000000000000000 ) ) ;
#47438 = EDGE_CURVE ( 'NONE', #27568, #7845, #37419, .T. ) ;
#47437 = DIRECTION ( 'NONE',  ( -0.000000000000000000, -1.000000000000000000, -0.000000000000000000 ) ) ;
#47439 = LINE ( 'NONE', #105045, #21510 ) ;
#47440 = AXIS2_PLACEMENT_3D ( 'NONE', #105151, #3108, #94057 ) ;
#47441 = ORIENTED_EDGE ( 'NONE', *, *, #82710, .T. ) ;
#47442 = DIRECTION ( 'NONE',  ( -0.000000000000000000, 1.000000000000000000, -0.000000000000000000 ) ) ;
#47443 = CARTESIAN_POINT ( 'NONE',  ( 2.299999999999949640, 12.50000000000000000, -0.3464101615137782364 ) ) ;
#47444 = EDGE_LOOP ( 'NONE', ( #14111, #43539, #41849, #97835 ) ) ;
#47445 = CARTESIAN_POINT ( 'NONE',  ( 12.89999999999989910, 2.500000000000000000, 0.5928203230275495006 ) ) ;
#47446 = DIRECTION ( 'NONE',  ( 0.000000000000000000, 0.000000000000000000, -1.000000000000000000 ) ) ;
#47447 = CARTESIAN_POINT ( 'NONE',  ( -14.14999999999998614, 12.50000000000000000, 2.099970236277064028 ) ) ;
#47448 = FACE_OUTER_BOUND ( 'NONE', #21366, .T. ) ;
#47449 = DIRECTION ( 'NONE',  ( 0.000000000000000000, 1.000000000000000000, 0.000000000000000000 ) ) ;
#47450 = ORIENTED_EDGE ( 'NONE', *, *, #105256, .F. ) ;
#47451 = AXIS2_PLACEMENT_3D ( 'NONE', #34014, #5820, #72658 ) ;
#47452 = VECTOR ( 'NONE', #9769, 1000.000000000000000 ) ;
#47453 = DIRECTION ( 'NONE',  ( 0.000000000000000000, 0.000000000000000000, 1.000000000000000000 ) ) ;
#47454 = DIRECTION ( 'NONE',  ( 0.000000000000000000, 1.000000000000000000, 0.000000000000000000 ) ) ;
#47455 = ORIENTED_EDGE ( 'NONE', *, *, #65516, .F. ) ;
#47457 = AXIS2_PLACEMENT_3D ( 'NONE', #42697, #122521, #72776 ) ;
#47456 = CIRCLE ( 'NONE', #62142, 0.1000000000000002554 ) ;
#47458 = CARTESIAN_POINT ( 'NONE',  ( -0.2000000000000408673, 2.500000000000000000, -3.983716857408426293 ) ) ;
#47459 = VERTEX_POINT ( 'NONE', #62784 ) ;
#47460 = VERTEX_POINT ( 'NONE', #63417 ) ;
#47461 = CARTESIAN_POINT ( 'NONE',  ( 7.299999999999927880, 2.500000000000000000, -4.676537180435977881 ) ) ;
#47462 = ORIENTED_EDGE ( 'NONE', *, *, #36078, .F. ) ;
#47463 = LINE ( 'NONE', #86067, #57218 ) ;
#47464 = LINE ( 'NONE', #128631, #94425 ) ;
#47465 = CONICAL_SURFACE ( 'NONE', #120629, 0.1000000000000000472, 0.003490658503988666988 ) ;
#47466 = CARTESIAN_POINT ( 'NONE',  ( 14.59999999999989484, 2.500000000000000000, -0.6928203230275541413 ) ) ;
#47467 = ORIENTED_EDGE ( 'NONE', *, *, #13914, .T. ) ;
#47469 = ADVANCED_FACE ( 'NONE', ( #93522 ), #56269, .T. ) ;
#47468 = VECTOR ( 'NONE', #21253, 1000.000000000000000 ) ;
#47470 = FACE_BOUND ( 'NONE', #109332, .T. ) ;
#47472 = ORIENTED_EDGE ( 'NONE', *, *, #49020, .F. ) ;
#47471 = DIRECTION ( 'NONE',  ( -0.000000000000000000, 1.000000000000000000, -0.000000000000000000 ) ) ;
#47473 = DIRECTION ( 'NONE',  ( 0.000000000000000000, 0.000000000000000000, -1.000000000000000000 ) ) ;
#47474 = EDGE_CURVE ( 'NONE', #99703, #20674, #3946, .T. ) ;
#47475 = PLANE ( 'NONE',  #113658 ) ;
#47476 = EDGE_CURVE ( 'NONE', #24974, #120381, #45822, .T. ) ;
#47477 = ORIENTED_EDGE ( 'NONE', *, *, #34546, .F. ) ;
#47478 = ORIENTED_EDGE ( 'NONE', *, *, #65946, .T. ) ;
#47479 = ORIENTED_EDGE ( 'NONE', *, *, #71138, .T. ) ;
#47480 = CARTESIAN_POINT ( 'NONE',  ( -11.89999999999999503, 2.500000000000000000, 4.676537180435972552 ) ) ;
#47481 = FACE_OUTER_BOUND ( 'NONE', #66305, .T. ) ;
#47482 = EDGE_CURVE ( 'NONE', #87449, #55169, #98035, .T. ) ;
#47483 = ADVANCED_FACE ( 'NONE', ( #53606 ), #104616, .T. ) ;
#47484 = DIRECTION ( 'NONE',  ( -4.274815082592931898E-19, -0.9999939076577903929, -0.003490651415223739937 ) ) ;
#47485 = EDGE_CURVE ( 'NONE', #9662, #11963, #58352, .T. ) ;
#47486 = FACE_BOUND ( 'NONE', #20957, .T. ) ;
#47488 = EDGE_CURVE ( 'NONE', #3359, #127971, #43797, .T. ) ;
#47487 = ORIENTED_EDGE ( 'NONE', *, *, #129123, .T. ) ;
#47489 = ADVANCED_FACE ( 'NONE', ( #74529 ), #66633, .T. ) ;
#47490 = AXIS2_PLACEMENT_3D ( 'NONE', #79256, #28212, #30157 ) ;
#47491 = CARTESIAN_POINT ( 'NONE',  ( 9.399999999999915090, 12.50000000000000000, 4.611443907251934426 ) ) ;
#47492 = CARTESIAN_POINT ( 'NONE',  ( 4.799999999999937650, 2.500000000000000000, -0.3464101615137782364 ) ) ;
#47493 = AXIS2_PLACEMENT_3D ( 'NONE', #96291, #24988, #104192 ) ;
#47494 = VERTEX_POINT ( 'NONE', #52959 ) ;
#47495 = CARTESIAN_POINT ( 'NONE',  ( 184.7916666666666572, 4.445597072760062218, -7.700000000000102318 ) ) ;
#47496 = CIRCLE ( 'NONE', #14021, 0.09999999999999982514 ) ;
#47497 = DIRECTION ( 'NONE',  ( 0.000000000000000000, 0.000000000000000000, -1.000000000000000000 ) ) ;
#47498 = CARTESIAN_POINT ( 'NONE',  ( -16.50000000000000000, -1.500000000000000000, 1.734723475976807094E-15 ) ) ;
#47499 = EDGE_CURVE ( 'NONE', #18828, #106287, #35357, .T. ) ;
#47500 = CARTESIAN_POINT ( 'NONE',  ( -12.29999999999999538, 12.50000000000000000, -4.676537180435976104 ) ) ;
#47501 = CIRCLE ( 'NONE', #118586, 0.06509327318403745899 ) ;
#47502 = DIRECTION ( 'NONE',  ( -0.000000000000000000, -1.000000000000000000, -0.000000000000000000 ) ) ;
#47503 = CONICAL_SURFACE ( 'NONE', #95613, 0.1000000000000002554, 0.003490658503988666988 ) ;
#47504 = EDGE_CURVE ( 'NONE', #20024, #91438, #83069, .T. ) ;
#47505 = CONICAL_SURFACE ( 'NONE', #74687, 0.09999999999999999167, 0.003490658503988666988 ) ;
#47506 = EDGE_LOOP ( 'NONE', ( #92323, #92738 ) ) ;
#47507 = EDGE_LOOP ( 'NONE', ( #9380, #17181 ) ) ;
#47508 = ORIENTED_EDGE ( 'NONE', *, *, #48818, .F. ) ;
#47509 = ORIENTED_EDGE ( 'NONE', *, *, #121380, .F. ) ;
#47510 = ORIENTED_EDGE ( 'NONE', *, *, #88894, .F. ) ;
#47511 = CARTESIAN_POINT ( 'NONE',  ( 108.0000000000000142, 8.500000000000000000, 0.2500000000000000000 ) ) ;
#47512 = CARTESIAN_POINT ( 'NONE',  ( 3.349999999999945466, 2.500000000000000000, -6.395190528383301931 ) ) ;
#47513 = VECTOR ( 'NONE', #49011, 1000.000000000000000 ) ;
#47514 = EDGE_LOOP ( 'NONE', ( #122601, #31726, #115255, #106367 ) ) ;
#47515 = FACE_BOUND ( 'NONE', #95875, .T. ) ;
#47516 = DIRECTION ( 'NONE',  ( 0.000000000000000000, 1.000000000000000000, 0.000000000000000000 ) ) ;
#47518 = AXIS2_PLACEMENT_3D ( 'NONE', #57667, #116565, #87107 ) ;
#47517 = CIRCLE ( 'NONE', #120675, 0.06509327318403745899 ) ;
#47519 = DIRECTION ( 'NONE',  ( -0.000000000000000000, 1.000000000000000000, -0.000000000000000000 ) ) ;
#47520 = CARTESIAN_POINT ( 'NONE',  ( 184.5000000000000000, -6.267304879582558996, 4.236192450104883100 ) ) ;
#47521 = DIRECTION ( 'NONE',  ( 0.000000000000000000, 0.000000000000000000, 1.000000000000000000 ) ) ;
#47522 = CARTESIAN_POINT ( 'NONE',  ( -10.45000000000000462, 2.500000000000000000, -6.595190528383298556 ) ) ;
#47523 = ORIENTED_EDGE ( 'NONE', *, *, #86189, .F. ) ;
#47524 = DIRECTION ( 'NONE',  ( 0.000000000000000000, 0.000000000000000000, 1.000000000000000000 ) ) ;
#47525 = EDGE_LOOP ( 'NONE', ( #18911, #34923 ) ) ;
#47526 = VERTEX_POINT ( 'NONE', #24785 ) ;
#47527 = EDGE_LOOP ( 'NONE', ( #114486, #111301 ) ) ;
#47528 = DIRECTION ( 'NONE',  ( 0.000000000000000000, 0.000000000000000000, 1.000000000000000000 ) ) ;
#47529 = DIRECTION ( 'NONE',  ( 0.000000000000000000, 1.000000000000000000, 0.000000000000000000 ) ) ;
#47530 = DIRECTION ( 'NONE',  ( 0.000000000000000000, 0.000000000000000000, 1.000000000000000000 ) ) ;
#47531 = EDGE_CURVE ( 'NONE', #79131, #122997, #54129, .T. ) ;
#47532 = EDGE_LOOP ( 'NONE', ( #114339, #25189 ) ) ;
#47533 = AXIS2_PLACEMENT_3D ( 'NONE', #126237, #44452, #75834 ) ;
#47534 = CARTESIAN_POINT ( 'NONE',  ( 16.56576425165006228, 1.499999999999999778, -6.084390597445810123 ) ) ;
#47535 = EDGE_CURVE ( 'NONE', #30131, #78082, #25400, .T. ) ;
#47536 = FACE_OUTER_BOUND ( 'NONE', #17317, .T. ) ;
#47537 = EDGE_CURVE ( 'NONE', #90525, #128150, #33334, .T. ) ;
#47538 = DIRECTION ( 'NONE',  ( 0.000000000000000000, -0.000000000000000000, 1.000000000000000000 ) ) ;
#47539 = CARTESIAN_POINT ( 'NONE',  ( 186.4010416670080588, -4.367472073101519747, 7.564683531249999149 ) ) ;
#47540 = DIRECTION ( 'NONE',  ( 0.000000000000000000, 1.000000000000000000, 0.000000000000000000 ) ) ;
#47541 = CARTESIAN_POINT ( 'NONE',  ( 194.5000000000000000, 0.000000000000000000, -5.000000000000000000 ) ) ;
#47542 = DIRECTION ( 'NONE',  ( -4.274815082592931898E-19, -0.9999939076577903929, -0.003490651415223739937 ) ) ;
#47543 = ADVANCED_FACE ( 'NONE', ( #124917 ), #83382, .T. ) ;
#47544 = ORIENTED_EDGE ( 'NONE', *, *, #2286, .T. ) ;
#47545 = DIRECTION ( 'NONE',  ( -4.274815082592931898E-19, -0.9999939076577903929, -0.003490651415223739937 ) ) ;
#47546 = EDGE_CURVE ( 'NONE', #44909, #113919, #73877, .T. ) ;
#47547 = CIRCLE ( 'NONE', #78949, 0.06509327318403741736 ) ;
#47548 = EDGE_LOOP ( 'NONE', ( #31247, #69258 ) ) ;
#47549 = CIRCLE ( 'NONE', #66309, 0.1000000000000000472 ) ;
#47550 = ADVANCED_FACE ( 'NONE', ( #34623 ), #104302, .T. ) ;
#47551 = VERTEX_POINT ( 'NONE', #65331 ) ;
#47552 = DIRECTION ( 'NONE',  ( -0.000000000000000000, 1.000000000000000000, -0.000000000000000000 ) ) ;
#47553 = CARTESIAN_POINT ( 'NONE',  ( 7.899999999999923084, 2.500000000000000000, 0.5928203230275495006 ) ) ;
#47554 = DIRECTION ( 'NONE',  ( 0.000000000000000000, 0.000000000000000000, -1.000000000000000000 ) ) ;
#47555 = ORIENTED_EDGE ( 'NONE', *, *, #106364, .F. ) ;
#47556 = ADVANCED_FACE ( 'NONE', ( #105273 ), #68796, .T. ) ;
#47559 = VERTEX_POINT ( 'NONE', #8990 ) ;
#47558 = AXIS2_PLACEMENT_3D ( 'NONE', #67201, #65944, #107152 ) ;
#47557 = AXIS2_PLACEMENT_3D ( 'NONE', #52937, #22206, #113794 ) ;
#47560 = CARTESIAN_POINT ( 'NONE',  ( 6.449999999999930012, 12.50000000000000000, -1.753560074763288679 ) ) ;
#47561 = CIRCLE ( 'NONE', #120708, 0.06509327318403745899 ) ;
#47562 = DIRECTION ( 'NONE',  ( -0.000000000000000000, 1.000000000000000000, -0.000000000000000000 ) ) ;
#47563 = CARTESIAN_POINT ( 'NONE',  ( 4.149999999999938183, 2.500000000000000000, 2.265063509461097357 ) ) ;
#47564 = ORIENTED_EDGE ( 'NONE', *, *, #38958, .T. ) ;
#47565 = EDGE_LOOP ( 'NONE', ( #38008, #62882 ) ) ;
#47566 = CARTESIAN_POINT ( 'NONE',  ( -7.300000000000018474, 2.500000000000000000, 0.3464101615137735735 ) ) ;
#47567 = CONICAL_SURFACE ( 'NONE', #99793, 0.1000000000000002554, 0.003490658503988666988 ) ;
#47568 = ORIENTED_EDGE ( 'NONE', *, *, #63171, .T. ) ;
#47569 = DIRECTION ( 'NONE',  ( -0.000000000000000000, 1.000000000000000000, -0.000000000000000000 ) ) ;
#47570 = AXIS2_PLACEMENT_3D ( 'NONE', #99025, #127835, #9355 ) ;
#47571 = DIRECTION ( 'NONE',  ( 1.000000000000000000, 0.000000000000000000, 0.000000000000000000 ) ) ;
#47572 = ORIENTED_EDGE ( 'NONE', *, *, #26819, .F. ) ;
#47573 = CARTESIAN_POINT ( 'NONE',  ( 14.99999999999989342, 2.500000000000000000, -0.6928203230275541413 ) ) ;
#47574 = PLANE ( 'NONE',  #108915 ) ;
#47575 = DIRECTION ( 'NONE',  ( 0.000000000000000000, -0.9999939076577903929, 0.003490651415223739937 ) ) ;
#47576 = EDGE_CURVE ( 'NONE', #18946, #35145, #125234, .T. ) ;
#47577 = CARTESIAN_POINT ( 'NONE',  ( 10.79999999999991367, 2.500000000000000000, -0.1000000000000023925 ) ) ;
#47578 = ORIENTED_EDGE ( 'NONE', *, *, #122610, .F. ) ;
#47580 = AXIS2_PLACEMENT_3D ( 'NONE', #61858, #51405, #71027 ) ;
#47579 = DIRECTION ( 'NONE',  ( -4.274815082592931898E-19, -0.9999939076577903929, -0.003490651415223739937 ) ) ;
#47581 = AXIS2_PLACEMENT_3D ( 'NONE', #129013, #118508, #89064 ) ;
#47582 = VERTEX_POINT ( 'NONE', #86912 ) ;
#47583 = ORIENTED_EDGE ( 'NONE', *, *, #93315, .T. ) ;
#47584 = DIRECTION ( 'NONE',  ( 0.000000000000000000, -0.9999939076577903929, 0.003490651415223739937 ) ) ;
#47585 = DIRECTION ( 'NONE',  ( 0.000000000000000000, 0.000000000000000000, 1.000000000000000000 ) ) ;
#47586 = CARTESIAN_POINT ( 'NONE',  ( 13.94999999999989626, 2.500000000000000000, 2.511473670974873507 ) ) ;
#47587 = CARTESIAN_POINT ( 'NONE',  ( -9.150000000000009237, 12.50000000000000000, -1.472243186433550122 ) ) ;
#47588 = AXIS2_PLACEMENT_3D ( 'NONE', #31927, #1798, #25153 ) ;
#47590 = AXIS2_PLACEMENT_3D ( 'NONE', #31444, #22278, #1318 ) ;
#47589 = LINE ( 'NONE', #46281, #48965 ) ;
#47591 = CARTESIAN_POINT ( 'NONE',  ( -7.300000000000016698, 2.500000000000000000, -0.3464101615137783474 ) ) ;
#47592 = CIRCLE ( 'NONE', #3660, 0.09999999999999982514 ) ;
#47594 = EDGE_CURVE ( 'NONE', #108189, #52320, #100103, .T. ) ;
#47593 = DIRECTION ( 'NONE',  ( 0.000000000000000000, -0.9999939076577903929, 0.003490651415223739937 ) ) ;
#47595 = DIRECTION ( 'NONE',  ( 0.000000000000000000, 0.000000000000000000, -1.000000000000000000 ) ) ;
#47596 = CARTESIAN_POINT ( 'NONE',  ( 9.149999999999918643, 2.500000000000000000, -6.395190528383301931 ) ) ;
#47597 = CIRCLE ( 'NONE', #127014, 9.000000000000001776 ) ;
#47598 = CONICAL_SURFACE ( 'NONE', #66363, 0.1000000000000002554, 0.003490658503988666988 ) ;
#47599 = FACE_OUTER_BOUND ( 'NONE', #104393, .T. ) ;
#47600 = AXIS2_PLACEMENT_3D ( 'NONE', #126183, #18152, #36535 ) ;
#47601 = ORIENTED_EDGE ( 'NONE', *, *, #12703, .F. ) ;
#47602 = DIRECTION ( 'NONE',  ( 0.000000000000000000, 1.000000000000000000, 0.000000000000000000 ) ) ;
#47603 = EDGE_CURVE ( 'NONE', #46223, #48711, #116810, .T. ) ;
#47604 = DIRECTION ( 'NONE',  ( 0.000000000000000000, 1.000000000000000000, 0.000000000000000000 ) ) ;
#47605 = CARTESIAN_POINT ( 'NONE',  ( -3.550000000000027800, 12.50000000000000000, 6.213873640053558134 ) ) ;
#47606 = CARTESIAN_POINT ( 'NONE',  ( 9.599999999999914380, 12.50000000000000000, -3.637306695894650055 ) ) ;
#47607 = DIRECTION ( 'NONE',  ( -0.000000000000000000, -1.000000000000000000, -0.000000000000000000 ) ) ;
#47608 = ORIENTED_EDGE ( 'NONE', *, *, #123324, .F. ) ;
#47609 = DIRECTION ( 'NONE',  ( 0.000000000000000000, 0.000000000000000000, 1.000000000000000000 ) ) ;
#47611 = AXIS2_PLACEMENT_3D ( 'NONE', #120141, #28535, #69087 ) ;
#47610 = CONICAL_SURFACE ( 'NONE', #97777, 0.09999999999999982514, 0.003490658503988666988 ) ;
#47612 = CARTESIAN_POINT ( 'NONE',  ( 9.599999999999917932, 12.50000000000000000, -0.6928203230275541413 ) ) ;
#47614 = ORIENTED_EDGE ( 'NONE', *, *, #88513, .T. ) ;
#47613 = DIRECTION ( 'NONE',  ( 0.000000000000000000, 0.000000000000000000, 1.000000000000000000 ) ) ;
#47615 = ORIENTED_EDGE ( 'NONE', *, *, #126756, .F. ) ;
#47616 = ORIENTED_EDGE ( 'NONE', *, *, #29198, .T. ) ;
#47617 = ORIENTED_EDGE ( 'NONE', *, *, #105248, .T. ) ;
#47618 = ORIENTED_EDGE ( 'NONE', *, *, #34042, .T. ) ;
#47619 = DIRECTION ( 'NONE',  ( -0.000000000000000000, 1.000000000000000000, -0.000000000000000000 ) ) ;
#47620 = CARTESIAN_POINT ( 'NONE',  ( 1.649999999999951505, 2.500000000000000000, -1.372243186433550033 ) ) ;
#47621 = CARTESIAN_POINT ( 'NONE',  ( -5.000000000000026645, 2.500000000000000000, -3.737306695894649700 ) ) ;
#47622 = CARTESIAN_POINT ( 'NONE',  ( 9.349999999999916156, 12.50000000000000000, -1.883746621131363597 ) ) ;
#47623 = ORIENTED_EDGE ( 'NONE', *, *, #65085, .T. ) ;
#47624 = EDGE_CURVE ( 'NONE', #40083, #9515, #87554, .T. ) ;
#47625 = DIRECTION ( 'NONE',  ( -4.274815082592931898E-19, -0.9999939076577903929, -0.003490651415223739937 ) ) ;
#47626 = ORIENTED_EDGE ( 'NONE', *, *, #9831, .T. ) ;
#47627 = CARTESIAN_POINT ( 'NONE',  ( 23.85240649352905962, -2.660544618042189224, -4.258220037323775742 ) ) ;
#47628 = CARTESIAN_POINT ( 'NONE',  ( 4.149999999999939959, 12.50000000000000000, -2.099970236277064473 ) ) ;
#47629 = DIRECTION ( 'NONE',  ( 0.000000000000000000, 0.000000000000000000, -1.000000000000000000 ) ) ;
#47630 = DIRECTION ( 'NONE',  ( 0.000000000000000000, 0.000000000000000000, 1.000000000000000000 ) ) ;
#47631 = CARTESIAN_POINT ( 'NONE',  ( -1.450000000000035483, 2.500000000000000000, 6.148780366869520897 ) ) ;
#47632 = ADVANCED_FACE ( 'NONE', ( #75798 ), #108595, .T. ) ;
#47633 = ORIENTED_EDGE ( 'NONE', *, *, #78534, .F. ) ;
#47634 = CIRCLE ( 'NONE', #37179, 0.1000000000000000472 ) ;
#47635 = VERTEX_POINT ( 'NONE', #26717 ) ;
#47636 = ORIENTED_EDGE ( 'NONE', *, *, #55513, .F. ) ;
#47637 = VERTEX_POINT ( 'NONE', #18818 ) ;
#47638 = PLANE ( 'NONE',  #19021 ) ;
#47639 = FACE_OUTER_BOUND ( 'NONE', #83791, .T. ) ;
#47640 = ADVANCED_FACE ( 'NONE', ( #56158 ), #127387, .T. ) ;
#47641 = ADVANCED_FACE ( 'NONE', ( #27333 ), #24968, .T. ) ;
#47642 = CARTESIAN_POINT ( 'NONE',  ( -9.350000000000004974, 12.50000000000000000, 6.083687093685483660 ) ) ;
#47643 = EDGE_CURVE ( 'NONE', #121018, #128018, #67919, .T. ) ;
#47644 = FACE_BOUND ( 'NONE', #22078, .T. ) ;
#47645 = ADVANCED_FACE ( 'NONE', ( #96094 ), #67240, .T. ) ;
#47646 = DIRECTION ( 'NONE',  ( 0.000000000000000000, 1.000000000000000000, 0.000000000000000000 ) ) ;
#47647 = DIRECTION ( 'NONE',  ( 0.000000000000000000, 1.000000000000000000, 0.000000000000000000 ) ) ;
#47648 = AXIS2_PLACEMENT_3D ( 'NONE', #43242, #3298, #32134 ) ;
#47649 = CARTESIAN_POINT ( 'NONE',  ( 187.5000000000000000, 0.000000000000000000, 7.700000000000000178 ) ) ;
#47650 = DIRECTION ( 'NONE',  ( 0.000000000000000000, 0.000000000000000000, -1.000000000000000000 ) ) ;
#47651 = AXIS2_PLACEMENT_3D ( 'NONE', #88426, #37423, #107435 ) ;
#47652 = AXIS2_PLACEMENT_3D ( 'NONE', #64426, #84714, #22114 ) ;
#47653 = ADVANCED_FACE ( 'NONE', ( #17521 ), #38491, .T. ) ;
#47654 = CARTESIAN_POINT ( 'NONE',  ( 186.2135416670080588, 4.367472073101518859, -7.564683531249999149 ) ) ;
#47655 = CARTESIAN_POINT ( 'NONE',  ( -1.900000000000034994, 12.50000000000000000, -0.2813168883297409439 ) ) ;
#47656 = EDGE_CURVE ( 'NONE', #106136, #108138, #112809, .T. ) ;
#47657 = DIRECTION ( 'NONE',  ( 0.000000000000000000, -0.000000000000000000, 1.000000000000000000 ) ) ;
#47658 = ADVANCED_FACE ( 'NONE', ( #28660 ), #45909, .T. ) ;
#47659 = AXIS2_PLACEMENT_3D ( 'NONE', #66808, #8528, #38012 ) ;
#47660 = EDGE_CURVE ( 'NONE', #13897, #66518, #79364, .T. ) ;
#47661 = FACE_OUTER_BOUND ( 'NONE', #8313, .T. ) ;
#47662 = ORIENTED_EDGE ( 'NONE', *, *, #111115, .T. ) ;
#47663 = ORIENTED_EDGE ( 'NONE', *, *, #92352, .T. ) ;
#47664 = VERTEX_POINT ( 'NONE', #118312 ) ;
#47665 = EDGE_LOOP ( 'NONE', ( #108365, #893, #19078, #32263 ) ) ;
#47666 = CONICAL_SURFACE ( 'NONE', #89423, 0.1000000000000000472, 0.003490658503988666988 ) ;
#47667 = DIRECTION ( 'NONE',  ( -0.000000000000000000, -1.000000000000000000, -0.000000000000000000 ) ) ;
#47668 = FACE_BOUND ( 'NONE', #59667, .T. ) ;
#47669 = EDGE_CURVE ( 'NONE', #112381, #63537, #77107, .T. ) ;
#47670 = CARTESIAN_POINT ( 'NONE',  ( 4.599999999999939249, 2.500000000000000000, -3.537306695894649966 ) ) ;
#47671 = AXIS2_PLACEMENT_3D ( 'NONE', #35889, #55537, #93041 ) ;
#47672 = STYLED_ITEM ( 'NONE', ( #61731 ), #119481 ) ;
#47673 = ORIENTED_EDGE ( 'NONE', *, *, #66214, .T. ) ;
#47674 = CARTESIAN_POINT ( 'NONE',  ( -12.89999999999999147, 2.500000000000000000, -0.6928203230275500335 ) ) ;
#47675 = CARTESIAN_POINT ( 'NONE',  ( -11.64999999999999858, 2.500000000000000000, -5.802370205355746435 ) ) ;
#47676 = FACE_OUTER_BOUND ( 'NONE', #128054, .T. ) ;
#47677 = VECTOR ( 'NONE', #11961, 1000.000000000000000 ) ;
#47678 = EDGE_LOOP ( 'NONE', ( #55974, #59412 ) ) ;
#47679 = CARTESIAN_POINT ( 'NONE',  ( 9.999999999999911182, 2.500000000000000000, -3.637306695894650055 ) ) ;
#47680 = AXIS2_PLACEMENT_3D ( 'NONE', #73297, #60904, #41927 ) ;
#47681 = CARTESIAN_POINT ( 'NONE',  ( 11.64999999999990443, 2.500000000000000000, -5.802370205355749988 ) ) ;
#47682 = AXIS2_PLACEMENT_3D ( 'NONE', #115358, #34922, #35556 ) ;
#47683 = ORIENTED_EDGE ( 'NONE', *, *, #35732, .F. ) ;
#47684 = DIRECTION ( 'NONE',  ( 0.000000000000000000, -0.9999939076577903929, 0.003490651415223739937 ) ) ;
#47685 = CARTESIAN_POINT ( 'NONE',  ( 3.099999999999945466, 12.50000000000000000, -3.983716857408426293 ) ) ;
#47686 = AXIS2_PLACEMENT_3D ( 'NONE', #64897, #76670, #95025 ) ;
#47687 = AXIS2_PLACEMENT_3D ( 'NONE', #99696, #119971, #78776 ) ;
#47688 = ORIENTED_EDGE ( 'NONE', *, *, #106733, .T. ) ;
#47689 = CARTESIAN_POINT ( 'NONE',  ( -3.750000000000031086, 12.50000000000000000, -5.867463478539787225 ) ) ;
#47690 = DIRECTION ( 'NONE',  ( 0.000000000000000000, 1.000000000000000000, 0.000000000000000000 ) ) ;
#47691 = VERTEX_POINT ( 'NONE', #96725 ) ;
#47692 = DIRECTION ( 'NONE',  ( 0.000000000000000000, 0.000000000000000000, 1.000000000000000000 ) ) ;
#47693 = VERTEX_POINT ( 'NONE', #68561 ) ;
#47694 = ORIENTED_EDGE ( 'NONE', *, *, #26652, .F. ) ;
#47695 = CIRCLE ( 'NONE', #93659, 0.06509327318403745899 ) ;
#47696 = DIRECTION ( 'NONE',  ( 0.000000000000000000, 0.000000000000000000, 1.000000000000000000 ) ) ;
#47697 = ORIENTED_EDGE ( 'NONE', *, *, #38969, .T. ) ;
#47698 = LINE ( 'NONE', #19509, #47106 ) ;
#47699 = FACE_BOUND ( 'NONE', #62110, .T. ) ;
#47700 = ADVANCED_FACE ( 'NONE', ( #47009 ), #58119, .T. ) ;
#47701 = CIRCLE ( 'NONE', #79099, 0.06509327318403745899 ) ;
#47702 = EDGE_LOOP ( 'NONE', ( #47116, #73659, #82972, #41006 ) ) ;
#47704 = EDGE_CURVE ( 'NONE', #58017, #40065, #8350, .T. ) ;
#47703 = CARTESIAN_POINT ( 'NONE',  ( -14.54999999999998472, 12.50000000000000000, -2.230156782645137170 ) ) ;
#47705 = ORIENTED_EDGE ( 'NONE', *, *, #77078, .F. ) ;
#47706 = DIRECTION ( 'NONE',  ( 0.000000000000000000, 0.000000000000000000, -1.000000000000000000 ) ) ;
#47707 = DIRECTION ( 'NONE',  ( -0.000000000000000000, -1.000000000000000000, -0.000000000000000000 ) ) ;
#47708 = DIRECTION ( 'NONE',  ( 0.000000000000000000, 1.000000000000000000, 0.000000000000000000 ) ) ;
#47709 = DIRECTION ( 'NONE',  ( -0.000000000000000000, 1.000000000000000000, -0.000000000000000000 ) ) ;
#47710 = CARTESIAN_POINT ( 'NONE',  ( 10.44999999999991402, 2.500000000000000000, -2.165063509461101710 ) ) ;
#47711 = EDGE_CURVE ( 'NONE', #37437, #44623, #89724, .T. ) ;
#47712 = VERTEX_POINT ( 'NONE', #31872 ) ;
#47713 = ORIENTED_EDGE ( 'NONE', *, *, #72659, .T. ) ;
#47714 = FACE_OUTER_BOUND ( 'NONE', #92721, .T. ) ;
#47715 = DIRECTION ( 'NONE',  ( 0.000000000000000000, 0.000000000000000000, 1.000000000000000000 ) ) ;
#47716 = CARTESIAN_POINT ( 'NONE',  ( 108.0000000000000142, 5.000000000000000000, 0.000000000000000000 ) ) ;
#47718 = EDGE_LOOP ( 'NONE', ( #126506, #39989 ) ) ;
#47717 = VERTEX_POINT ( 'NONE', #118956 ) ;
#47719 = ORIENTED_EDGE ( 'NONE', *, *, #45543, .T. ) ;
#47720 = DIRECTION ( 'NONE',  ( 0.000000000000000000, 1.000000000000000000, 0.000000000000000000 ) ) ;
#47721 = DIRECTION ( 'NONE',  ( 0.000000000000000000, -0.9999939076577903929, 0.003490651415223739937 ) ) ;
#47722 = DIRECTION ( 'NONE',  ( 0.000000000000000000, 0.000000000000000000, 1.000000000000000000 ) ) ;
#47723 = PRODUCT_CONTEXT ( 'NONE', #44700, 'mechanical' ) ;
#47724 = LINE ( 'NONE', #127566, #55686 ) ;
#47725 = DIRECTION ( 'NONE',  ( 0.000000000000000000, 0.000000000000000000, 1.000000000000000000 ) ) ;
#47726 = CIRCLE ( 'NONE', #33070, 0.06509327318403743123 ) ;
#47727 = AXIS2_PLACEMENT_3D ( 'NONE', #61569, #32108, #11146 ) ;
#47728 = CARTESIAN_POINT ( 'NONE',  ( -13.34999999999999076, 12.50000000000000000, 2.857883832488652853 ) ) ;
#47729 = DIRECTION ( 'NONE',  ( 0.000000000000000000, 0.000000000000000000, -1.000000000000000000 ) ) ;
#47730 = CARTESIAN_POINT ( 'NONE',  ( 12.49999999999993605, 12.50000000000000000, -2.276824562219559311E-15 ) ) ;
#47731 = AXIS2_PLACEMENT_3D ( 'NONE', #73119, #113034, #81639 ) ;
#47732 = ORIENTED_EDGE ( 'NONE', *, *, #32557, .F. ) ;
#47734 = ORIENTED_EDGE ( 'NONE', *, *, #12351, .F. ) ;
#47733 = AXIS2_PLACEMENT_3D ( 'NONE', #121761, #122427, #42589 ) ;
#47735 = AXIS2_PLACEMENT_3D ( 'NONE', #122266, #62701, #3766 ) ;
#47736 = CARTESIAN_POINT ( 'NONE',  ( -8.100000000000013856, 2.500000000000000000, -0.3464101615137782364 ) ) ;
#47737 = ORIENTED_EDGE ( 'NONE', *, *, #109122, .F. ) ;
#47738 = ORIENTED_EDGE ( 'NONE', *, *, #52848, .T. ) ;
#47739 = PLANE ( 'NONE',  #271 ) ;
#47740 = LINE ( 'NONE', #87640, #5136 ) ;
#47741 = CARTESIAN_POINT ( 'NONE',  ( -11.04999999999999893, 12.50000000000000000, 1.818653347947321475 ) ) ;
#47742 = AXIS2_PLACEMENT_3D ( 'NONE', #91676, #1995, #44411 ) ;
#47743 = CARTESIAN_POINT ( 'NONE',  ( -5.850000000000019185, 2.500000000000000000, 2.165063509461097713 ) ) ;
#47744 = AXIS2_PLACEMENT_3D ( 'NONE', #22328, #122456, #33438 ) ;
#47745 = CARTESIAN_POINT ( 'NONE',  ( 7.699999999999923794, 12.50000000000000000, -3.983716857408426293 ) ) ;
#47746 = DIRECTION ( 'NONE',  ( -4.274815082592931898E-19, -0.9999939076577903929, -0.003490651415223739937 ) ) ;
#47747 = FACE_OUTER_BOUND ( 'NONE', #89226, .T. ) ;
#47748 = ORIENTED_EDGE ( 'NONE', *, *, #44636, .T. ) ;
#47749 = CARTESIAN_POINT ( 'NONE',  ( -13.34999999999999076, 2.500000000000000000, -2.857883832488651521 ) ) ;
#47750 = LINE ( 'NONE', #16949, #89753 ) ;
#47751 = CIRCLE ( 'NONE', #12219, 0.06509327318403745899 ) ;
#47752 = EDGE_LOOP ( 'NONE', ( #71873, #47373 ) ) ;
#47753 = ORIENTED_EDGE ( 'NONE', *, *, #109122, .T. ) ;
#47754 = EDGE_CURVE ( 'NONE', #103724, #94980, #104396, .T. ) ;
#47755 = CIRCLE ( 'NONE', #108383, 0.09999999999999999167 ) ;
#47756 = ORIENTED_EDGE ( 'NONE', *, *, #90054, .T. ) ;
#47758 = ORIENTED_EDGE ( 'NONE', *, *, #84342, .F. ) ;
#47757 = ADVANCED_FACE ( 'NONE', ( #70498 ), #41714, .T. ) ;
#47759 = CARTESIAN_POINT ( 'NONE',  ( -6.900000000000019007, 2.500000000000000000, -4.676537180435978769 ) ) ;
#47760 = CARTESIAN_POINT ( 'NONE',  ( -13.34999999999999076, 2.500000000000000000, 2.265063509461101354 ) ) ;
#47761 = AXIS2_PLACEMENT_3D ( 'NONE', #107297, #49050, #37289 ) ;
#47762 = VERTEX_POINT ( 'NONE', #40420 ) ;
#47763 = LINE ( 'NONE', #107314, #46443 ) ;
#47764 = DIRECTION ( 'NONE',  ( 0.000000000000000000, 0.000000000000000000, 1.000000000000000000 ) ) ;
#47765 =( GEOMETRIC_REPRESENTATION_CONTEXT ( 3 ) GLOBAL_UNCERTAINTY_ASSIGNED_CONTEXT ( ( #18275 ) ) GLOBAL_UNIT_ASSIGNED_CONTEXT ( ( #98248, #11153, #111956 ) ) REPRESENTATION_CONTEXT ( 'NONE', 'WORKASPACE' ) );
#47766 = DIRECTION ( 'NONE',  ( 0.000000000000000000, 0.000000000000000000, 1.000000000000000000 ) ) ;
#47767 = ORIENTED_EDGE ( 'NONE', *, *, #70730, .T. ) ;
#47768 = EDGE_CURVE ( 'NONE', #77652, #55549, #12441, .T. ) ;
#47769 = CARTESIAN_POINT ( 'NONE',  ( 8.749999999999920064, 2.500000000000000000, -2.857883832488653741 ) ) ;
#47770 = CONICAL_SURFACE ( 'NONE', #116702, 0.1000000000000002554, 0.003490658503988666988 ) ;
#47771 = DIRECTION ( 'NONE',  ( -0.000000000000000000, -1.000000000000000000, -0.000000000000000000 ) ) ;
#47772 = VERTEX_POINT ( 'NONE', #11575 ) ;
#47773 = AXIS2_PLACEMENT_3D ( 'NONE', #18474, #109437, #117285 ) ;
#47774 = VERTEX_POINT ( 'NONE', #39779 ) ;
#47775 = ORIENTED_EDGE ( 'NONE', *, *, #26962, .F. ) ;
#47776 = DIRECTION ( 'NONE',  ( 0.000000000000000000, 0.000000000000000000, -1.000000000000000000 ) ) ;
#47777 = AXIS2_PLACEMENT_3D ( 'NONE', #126403, #116568, #66816 ) ;
#47778 = DIRECTION ( 'NONE',  ( 0.000000000000000000, 0.000000000000000000, 1.000000000000000000 ) ) ;
#47779 = EDGE_CURVE ( 'NONE', #60636, #93446, #18708, .T. ) ;
#47780 = ORIENTED_EDGE ( 'NONE', *, *, #64013, .F. ) ;
#47781 = DIRECTION ( 'NONE',  ( -0.000000000000000000, -1.000000000000000000, -0.000000000000000000 ) ) ;
#47783 = CIRCLE ( 'NONE', #64496, 0.1000000000000002554 ) ;
#47782 = DIRECTION ( 'NONE',  ( 0.000000000000000000, 0.000000000000000000, -1.000000000000000000 ) ) ;
#47784 = DIRECTION ( 'NONE',  ( 0.000000000000000000, 0.000000000000000000, -1.000000000000000000 ) ) ;
#47785 = CARTESIAN_POINT ( 'NONE',  ( -1.650000000000034772, 2.500000000000000000, 6.595190528383296780 ) ) ;
#47786 = ADVANCED_FACE ( 'NONE', ( #19463 ), #121117, .T. ) ;
#47787 = VERTEX_POINT ( 'NONE', #71140 ) ;
#47789 = AXIS2_PLACEMENT_3D ( 'NONE', #46320, #86888, #85602 ) ;
#47788 = AXIS2_PLACEMENT_3D ( 'NONE', #46273, #16790, #35192 ) ;
#47790 = CARTESIAN_POINT ( 'NONE',  ( 10.39999999999991154, 12.50000000000000000, 3.637306695894644726 ) ) ;
#47791 = ORIENTED_EDGE ( 'NONE', *, *, #67874, .F. ) ;
#47792 = ORIENTED_EDGE ( 'NONE', *, *, #122144, .T. ) ;
#47793 = DIRECTION ( 'NONE',  ( 0.000000000000000000, 1.000000000000000000, 0.000000000000000000 ) ) ;
#47794 = ADVANCED_FACE ( 'NONE', ( #48943 ), #14481, .T. ) ;
#47795 = EDGE_CURVE ( 'NONE', #4367, #65655, #91431, .T. ) ;
#47796 = PLANE ( 'NONE',  #87802 ) ;
#47797 = ADVANCED_FACE ( 'NONE', ( #88853 ), #21394, .T. ) ;
#47798 = FACE_BOUND ( 'NONE', #63568, .T. ) ;
#47799 = EDGE_CURVE ( 'NONE', #58927, #22783, #109115, .T. ) ;
#47800 = CARTESIAN_POINT ( 'NONE',  ( -5.000000000000022204, 2.500000000000000000, 3.737306695894644371 ) ) ;
#47801 = DIRECTION ( 'NONE',  ( 0.000000000000000000, 0.000000000000000000, 1.000000000000000000 ) ) ;
#47802 = LINE ( 'NONE', #116523, #119158 ) ;
#47803 = EDGE_CURVE ( 'NONE', #46113, #89857, #58437, .T. ) ;
#47804 = CIRCLE ( 'NONE', #91614, 0.06509327318403745899 ) ;
#47805 = EDGE_LOOP ( 'NONE', ( #18970, #93583 ) ) ;
#47806 = CARTESIAN_POINT ( 'NONE',  ( 11.64999999999990443, 2.500000000000000000, -5.702370205355749455 ) ) ;
#47807 = DIRECTION ( 'NONE',  ( 0.000000000000000000, 1.000000000000000000, 0.000000000000000000 ) ) ;
#47808 = ADVANCED_FACE ( 'NONE', ( #29302 ), #10305, .T. ) ;
#47809 = CARTESIAN_POINT ( 'NONE',  ( 3.549999999999943867, 2.500000000000000000, -1.918653347947326004 ) ) ;
#47810 = DIRECTION ( 'NONE',  ( -0.000000000000000000, -1.000000000000000000, -0.000000000000000000 ) ) ;
#47811 = ORIENTED_EDGE ( 'NONE', *, *, #109535, .T. ) ;
#47812 = DIRECTION ( 'NONE',  ( 0.000000000000000000, -0.000000000000000000, 1.000000000000000000 ) ) ;
#47813 = EDGE_CURVE ( 'NONE', #94018, #51302, #52164, .T. ) ;
#47814 = AXIS2_PLACEMENT_3D ( 'NONE', #128932, #19593, #59552 ) ;
#47815 = ADVANCED_FACE ( 'NONE', ( #89501 ), #75150, .T. ) ;
#47816 = CONICAL_SURFACE ( 'NONE', #95919, 0.09999999999999982514, 0.003490658503988666988 ) ;
#47817 = CARTESIAN_POINT ( 'NONE',  ( -5.850000000000018296, 12.50000000000000000, 7.188010851410848723 ) ) ;
#47818 = AXIS2_PLACEMENT_3D ( 'NONE', #100658, #102599, #3763 ) ;
#47819 = ORIENTED_EDGE ( 'NONE', *, *, #27649, .T. ) ;
#47820 = ORIENTED_EDGE ( 'NONE', *, *, #107023, .F. ) ;
#47821 = PLANE ( 'NONE',  #23079 ) ;
#47822 = EDGE_CURVE ( 'NONE', #97854, #331, #80973, .T. ) ;
#47823 = DIRECTION ( 'NONE',  ( 0.000000000000000000, -0.000000000000000000, 1.000000000000000000 ) ) ;
#47824 = FACE_BOUND ( 'NONE', #49176, .T. ) ;
#47825 = EDGE_CURVE ( 'NONE', #112012, #9827, #60064, .T. ) ;
#47826 = DIRECTION ( 'NONE',  ( -0.000000000000000000, 1.000000000000000000, -0.000000000000000000 ) ) ;
#47827 = AXIS2_PLACEMENT_3D ( 'NONE', #127703, #76032, #116589 ) ;
#47828 = CIRCLE ( 'NONE', #12298, 0.09999999999999982514 ) ;
#47829 = AXIS2_PLACEMENT_3D ( 'NONE', #48867, #128730, #39057 ) ;
#47830 = ORIENTED_EDGE ( 'NONE', *, *, #87616, .T. ) ;
#47831 = CARTESIAN_POINT ( 'NONE',  ( -1.850000000000033396, 2.500000000000000000, -1.818653347947325916 ) ) ;
#47832 = AXIS2_PLACEMENT_3D ( 'NONE', #2110, #40122, #60429 ) ;
#47833 = EDGE_LOOP ( 'NONE', ( #22467, #71697 ) ) ;
#47834 = ORIENTED_EDGE ( 'NONE', *, *, #122741, .T. ) ;
#47835 = CARTESIAN_POINT ( 'NONE',  ( 19.09982477502547127, 0.5559300837585704480, -4.454172625795856710 ) ) ;
#47836 = CARTESIAN_POINT ( 'NONE',  ( 186.2083333333333144, -4.445597072760115509, -7.700000000000001954 ) ) ;
#47837 = AXIS2_PLACEMENT_3D ( 'NONE', #104459, #34453, #4958 ) ;
#47838 = ORIENTED_EDGE ( 'NONE', *, *, #117363, .T. ) ;
#47839 = CARTESIAN_POINT ( 'NONE',  ( 5.599999999999931255, 12.50000000000000000, 3.983716857408420076 ) ) ;
#47840 = CARTESIAN_POINT ( 'NONE',  ( 187.5000000000000000, 0.000000000000000000, 0.000000000000000000 ) ) ;
#47841 = AXIS2_PLACEMENT_3D ( 'NONE', #68674, #127603, #67354 ) ;
#47842 = DIRECTION ( 'NONE',  ( 0.000000000000000000, 1.000000000000000000, 0.000000000000000000 ) ) ;
#47843 = CARTESIAN_POINT ( 'NONE',  ( 1.649999999999951505, 2.500000000000000000, -2.957883832488653830 ) ) ;
#47844 = AXIS2_PLACEMENT_3D ( 'NONE', #121562, #71843, #115438 ) ;
#47845 = ORIENTED_EDGE ( 'NONE', *, *, #44116, .F. ) ;
#47846 = CARTESIAN_POINT ( 'NONE',  ( 12.69999999999989804, 12.50000000000000000, 0.4115034346978109769 ) ) ;
#47847 = CARTESIAN_POINT ( 'NONE',  ( -8.350000000000013856, 2.500000000000000000, -7.288010851410849256 ) ) ;
#47848 = DIRECTION ( 'NONE',  ( 0.000000000000000000, 0.000000000000000000, 1.000000000000000000 ) ) ;
#47849 = CONICAL_SURFACE ( 'NONE', #120998, 0.1000000000000002554, 0.003490658503988666988 ) ;
#47850 = DIRECTION ( 'NONE',  ( -0.000000000000000000, -1.000000000000000000, -0.000000000000000000 ) ) ;
#47851 = ORIENTED_EDGE ( 'NONE', *, *, #26220, .T. ) ;
#47852 = CARTESIAN_POINT ( 'NONE',  ( -8.750000000000008882, 12.50000000000000000, 1.537336459617582918 ) ) ;
#47853 = ORIENTED_EDGE ( 'NONE', *, *, #62722, .F. ) ;
#47854 = CARTESIAN_POINT ( 'NONE',  ( 18.00406198521885770, 1.510509990005263647, 4.944015973543540277 ) ) ;
#47855 = VERTEX_POINT ( 'NONE', #80333 ) ;
#47856 = CARTESIAN_POINT ( 'NONE',  ( -13.54999999999998828, 12.50000000000000000, -2.511473670974875727 ) ) ;
#47857 = CARTESIAN_POINT ( 'NONE',  ( 87.50000000000002842, -6.761363245278262823, 3.308765358479927254 ) ) ;
#47858 = EDGE_CURVE ( 'NONE', #116188, #118850, #63256, .T. ) ;
#47859 = DIRECTION ( 'NONE',  ( 0.000000000000000000, 1.000000000000000000, 0.000000000000000000 ) ) ;
#47860 = CARTESIAN_POINT ( 'NONE',  ( 3.549999999999942091, 2.500000000000000000, 2.511473670974873507 ) ) ;
#47861 = EDGE_LOOP ( 'NONE', ( #122122, #63683, #128204, #42326 ) ) ;
#47862 = AXIS2_PLACEMENT_3D ( 'NONE', #81549, #31179, #33115 ) ;
#47864 = EDGE_CURVE ( 'NONE', #16549, #60383, #102347, .T. ) ;
#47863 = DIRECTION ( 'NONE',  ( -0.000000000000000000, -1.000000000000000000, -0.000000000000000000 ) ) ;
#47865 = DIRECTION ( 'NONE',  ( 0.000000000000000000, 0.000000000000000000, 1.000000000000000000 ) ) ;
#47866 = DIRECTION ( 'NONE',  ( -0.000000000000000000, -1.000000000000000000, -0.000000000000000000 ) ) ;
#47867 = DIRECTION ( 'NONE',  ( 0.000000000000000000, 1.000000000000000000, 0.000000000000000000 ) ) ;
#47868 = CARTESIAN_POINT ( 'NONE',  ( 8.149999999999923972, 12.50000000000000000, 1.883746621131358934 ) ) ;
#47870 = VERTEX_POINT ( 'NONE', #3060 ) ;
#47869 = AXIS2_PLACEMENT_3D ( 'NONE', #77872, #108630, #107984 ) ;
#47871 = VERTEX_POINT ( 'NONE', #34459 ) ;
#47872 = CARTESIAN_POINT ( 'NONE',  ( 1.449999999999950440, 2.500000000000000000, 6.248780366869520542 ) ) ;
#47873 = EDGE_LOOP ( 'NONE', ( #73275, #72267, #2507, #61748 ) ) ;
#47874 = LINE ( 'NONE', #18395, #103676 ) ;
#47876 = ORIENTED_EDGE ( 'NONE', *, *, #65959, .T. ) ;
#47875 = VERTEX_POINT ( 'NONE', #114920 ) ;
#47877 = ORIENTED_EDGE ( 'NONE', *, *, #76135, .T. ) ;
#47878 = CIRCLE ( 'NONE', #123084, 0.1000000000000002554 ) ;
#47879 = FACE_OUTER_BOUND ( 'NONE', #61803, .T. ) ;
#47880 = CARTESIAN_POINT ( 'NONE',  ( -2.500000000000031086, 12.50000000000000000, 3.637306695894644726 ) ) ;
#47881 = CARTESIAN_POINT ( 'NONE',  ( 0.6499999999999543920, 2.500000000000000000, 6.941600689897073018 ) ) ;
#47882 = SURFACE_STYLE_FILL_AREA ( #7931 ) ;
#47883 = AXIS2_PLACEMENT_3D ( 'NONE', #33961, #45079, #45720 ) ;
#47884 = LINE ( 'NONE', #57701, #116224 ) ;
#47885 = CARTESIAN_POINT ( 'NONE',  ( 6.649999999999929301, 2.500000000000000000, -2.165063509461101710 ) ) ;
#47886 = PLANE ( 'NONE',  #72691 ) ;
#47887 = FACE_OUTER_BOUND ( 'NONE', #38455, .T. ) ;
#47888 = CONICAL_SURFACE ( 'NONE', #95992, 0.1000000000000002554, 0.003490658503988666988 ) ;
#47889 = VERTEX_POINT ( 'NONE', #73080 ) ;
#47890 = PLANE ( 'NONE',  #100051 ) ;
#47891 = ORIENTED_EDGE ( 'NONE', *, *, #112731, .T. ) ;
#47892 = AXIS2_PLACEMENT_3D ( 'NONE', #122170, #3669, #123436 ) ;
#47893 = ORIENTED_EDGE ( 'NONE', *, *, #77237, .T. ) ;
#47894 = ORIENTED_EDGE ( 'NONE', *, *, #7111, .F. ) ;
#47895 = ORIENTED_EDGE ( 'NONE', *, *, #51067, .F. ) ;
#47896 = FACE_OUTER_BOUND ( 'NONE', #30621, .T. ) ;
#47897 = ORIENTED_EDGE ( 'NONE', *, *, #69936, .T. ) ;
#47898 = ORIENTED_EDGE ( 'NONE', *, *, #93314, .T. ) ;
#47899 = EDGE_CURVE ( 'NONE', #121477, #23084, #3690, .T. ) ;
#47900 = CARTESIAN_POINT ( 'NONE',  ( 176.5000000000000000, 0.000000000000000000, 0.000000000000000000 ) ) ;
#47901 = DIRECTION ( 'NONE',  ( 0.000000000000000000, 1.000000000000000000, 0.000000000000000000 ) ) ;
#47902 = CARTESIAN_POINT ( 'NONE',  ( -10.40000000000000213, 2.500000000000000000, 3.637306695894644726 ) ) ;
#47903 = CARTESIAN_POINT ( 'NONE',  ( 3.749999999999940492, 2.500000000000000000, 2.857883832488649301 ) ) ;
#47905 = CIRCLE ( 'NONE', #75081, 0.1000000000000002554 ) ;
#47904 = CARTESIAN_POINT ( 'NONE',  ( 9.599999999999914380, 2.500000000000000000, 5.022947341949748790 ) ) ;
#47906 = ORIENTED_EDGE ( 'NONE', *, *, #95780, .T. ) ;
#47907 = DIRECTION ( 'NONE',  ( -0.000000000000000000, 1.000000000000000000, -0.000000000000000000 ) ) ;
#47908 = ORIENTED_EDGE ( 'NONE', *, *, #45876, .F. ) ;
#47910 = DIRECTION ( 'NONE',  ( 0.000000000000000000, 0.000000000000000000, 1.000000000000000000 ) ) ;
#47909 = AXIS2_PLACEMENT_3D ( 'NONE', #54212, #7013, #16191 ) ;
#47911 = VERTEX_POINT ( 'NONE', #54707 ) ;
#47912 = LINE ( 'NONE', #87806, #90150 ) ;
#47913 = ORIENTED_EDGE ( 'NONE', *, *, #63752, .F. ) ;
#47914 = EDGE_CURVE ( 'NONE', #125307, #21757, #73091, .T. ) ;
#47915 = EDGE_CURVE ( 'NONE', #58504, #62036, #4027, .T. ) ;
#47916 = EDGE_LOOP ( 'NONE', ( #121133, #83137 ) ) ;
#47918 = CIRCLE ( 'NONE', #112658, 0.1000000000000002554 ) ;
#47917 = DIRECTION ( 'NONE',  ( -0.000000000000000000, 1.000000000000000000, -0.000000000000000000 ) ) ;
#47919 = CARTESIAN_POINT ( 'NONE',  ( 43.29488422903774847, -3.510951914389875750, -3.940494739282157433 ) ) ;
#47920 = CIRCLE ( 'NONE', #60542, 0.06509327318403745899 ) ;
#47921 = CIRCLE ( 'NONE', #87603, 0.06509327318403745899 ) ;
#47922 = DIRECTION ( 'NONE',  ( 0.000000000000000000, 1.000000000000000000, 0.000000000000000000 ) ) ;
#47923 = FACE_OUTER_BOUND ( 'NONE', #105607, .T. ) ;
#47924 = DIRECTION ( 'NONE',  ( -4.274815082592931898E-19, -0.9999939076577903929, -0.003490651415223739937 ) ) ;
#47925 = ORIENTED_EDGE ( 'NONE', *, *, #95412, .F. ) ;
#47926 = DIRECTION ( 'NONE',  ( 0.000000000000000000, 0.000000000000000000, 1.000000000000000000 ) ) ;
#47927 = DIRECTION ( 'NONE',  ( 0.000000000000000000, -0.9999939076577903929, 0.003490651415223739937 ) ) ;
#47928 = EDGE_CURVE ( 'NONE', #48277, #90721, #77209, .T. ) ;
#47929 = CARTESIAN_POINT ( 'NONE',  ( -3.150000000000030553, 2.500000000000000000, 6.148780366869520009 ) ) ;
#47930 = CARTESIAN_POINT ( 'NONE',  ( -12.29999999999999538, 12.50000000000000000, -0.3464101615137741841 ) ) ;
#47931 = AXIS2_PLACEMENT_3D ( 'NONE', #12685, #119421, #91914 ) ;
#47932 = CARTESIAN_POINT ( 'NONE',  ( 7.499999999999927169, 2.500000000000000000, 3.637306695894644726 ) ) ;
#47933 = AXIS2_PLACEMENT_3D ( 'NONE', #97180, #124229, #38270 ) ;
#47934 = EDGE_LOOP ( 'NONE', ( #67495, #123541, #27488, #93535 ) ) ;
#47935 = ORIENTED_EDGE ( 'NONE', *, *, #96812, .F. ) ;
#47936 = LINE ( 'NONE', #108761, #123993 ) ;
#47937 = ORIENTED_EDGE ( 'NONE', *, *, #90954, .F. ) ;
#47938 = CARTESIAN_POINT ( 'NONE',  ( 14.19999999999989626, 2.500000000000000000, -2.276824562219559311E-15 ) ) ;
#47939 = DIRECTION ( 'NONE',  ( 0.000000000000000000, 1.000000000000000000, 0.000000000000000000 ) ) ;
#47940 = VERTEX_POINT ( 'NONE', #113003 ) ;
#47941 = CARTESIAN_POINT ( 'NONE',  ( 186.5000000000000000, 0.000000000000000000, 7.700000000000000178 ) ) ;
#47942 = DIRECTION ( 'NONE',  ( -0.000000000000000000, -1.000000000000000000, -0.000000000000000000 ) ) ;
#47943 = FACE_OUTER_BOUND ( 'NONE', #116673, .T. ) ;
#47944 = DIRECTION ( 'NONE',  ( 0.000000000000000000, 1.000000000000000000, 0.000000000000000000 ) ) ;
#47945 = ORIENTED_EDGE ( 'NONE', *, *, #5098, .T. ) ;
#47946 = EDGE_CURVE ( 'NONE', #100782, #122978, #2377, .T. ) ;
#47947 = DIRECTION ( 'NONE',  ( 0.000000000000000000, 1.000000000000000000, 0.000000000000000000 ) ) ;
#47948 = DIRECTION ( 'NONE',  ( -0.000000000000000000, -1.000000000000000000, -0.000000000000000000 ) ) ;
#47949 = EDGE_LOOP ( 'NONE', ( #39460, #36873, #26573, #31837 ) ) ;
#47950 = ADVANCED_FACE ( 'NONE', ( #25245 ), #98211, .T. ) ;
#47951 = LINE ( 'NONE', #55190, #107067 ) ;
#47952 = CIRCLE ( 'NONE', #77195, 0.1000000000000000056 ) ;
#47953 = DIRECTION ( 'NONE',  ( 0.000000000000000000, 0.000000000000000000, 1.000000000000000000 ) ) ;
#47954 = ADVANCED_FACE ( 'NONE', ( #82910 ), #52155, .T. ) ;
#47955 = CARTESIAN_POINT ( 'NONE',  ( 11.89999999999990798, 12.50000000000000000, 3.918623584224383727 ) ) ;
#47956 = ORIENTED_EDGE ( 'NONE', *, *, #830, .F. ) ;
#47957 = DIRECTION ( 'NONE',  ( -0.000000000000000000, -1.000000000000000000, -0.000000000000000000 ) ) ;
#47958 = ADVANCED_FACE ( 'NONE', ( #103185 ), #16715, .T. ) ;
#47959 = EDGE_CURVE ( 'NONE', #111595, #17095, #119148, .T. ) ;
#47960 = ORIENTED_EDGE ( 'NONE', *, *, #112377, .F. ) ;
#47962 = AXIS2_PLACEMENT_3D ( 'NONE', #101644, #14359, #32280 ) ;
#47961 = CARTESIAN_POINT ( 'NONE',  ( -8.950000000000008171, 2.500000000000000000, 1.718653347947321386 ) ) ;
#47963 = CARTESIAN_POINT ( 'NONE',  ( 11.64999999999990443, 12.50000000000000000, 1.472243186433545459 ) ) ;
#47964 = EDGE_CURVE ( 'NONE', #42047, #126587, #13499, .T. ) ;
#47965 = EDGE_CURVE ( 'NONE', #39568, #8482, #14582, .T. ) ;
#47966 = CARTESIAN_POINT ( 'NONE',  ( -1.850000000000033396, 2.500000000000000000, -2.611473670974877592 ) ) ;
#47967 = ORIENTED_EDGE ( 'NONE', *, *, #1907, .F. ) ;
#47968 = DIRECTION ( 'NONE',  ( -0.000000000000000000, 1.000000000000000000, -0.000000000000000000 ) ) ;
#47971 = EDGE_CURVE ( 'NONE', #4778, #90560, #123268, .T. ) ;
#47970 = AXIS2_PLACEMENT_3D ( 'NONE', #51517, #29943, #69197 ) ;
#47969 = AXIS2_PLACEMENT_3D ( 'NONE', #111001, #32495, #20718 ) ;
#47972 = CARTESIAN_POINT ( 'NONE',  ( -6.450000000000016165, 12.50000000000000000, 2.446380397790835826 ) ) ;
#47973 = CIRCLE ( 'NONE', #45913, 0.06509327318403741736 ) ;
#47974 = ORIENTED_EDGE ( 'NONE', *, *, #69500, .F. ) ;
#47975 = DIRECTION ( 'NONE',  ( 0.000000000000000000, 0.000000000000000000, 1.000000000000000000 ) ) ;
#47976 = ORIENTED_EDGE ( 'NONE', *, *, #41304, .T. ) ;
#47977 = ADVANCED_FACE ( 'NONE', ( #23987 ), #66807, .T. ) ;
#47978 = CARTESIAN_POINT ( 'NONE',  ( 9.199999999999919353, 12.50000000000000000, -2.276824562219559311E-15 ) ) ;
#47980 = CIRCLE ( 'NONE', #64686, 0.06509327318403745899 ) ;
#47979 = CONICAL_SURFACE ( 'NONE', #70954, 0.09999999999999999167, 0.003490658503988666988 ) ;
#47981 = VERTEX_POINT ( 'NONE', #122190 ) ;
#47982 = DIRECTION ( 'NONE',  ( 0.000000000000000000, 1.000000000000000000, 0.000000000000000000 ) ) ;
#47983 = FACE_OUTER_BOUND ( 'NONE', #115851, .T. ) ;
#47984 = ORIENTED_EDGE ( 'NONE', *, *, #26004, .F. ) ;
#47985 = ORIENTED_EDGE ( 'NONE', *, *, #27051, .T. ) ;
#47986 = CARTESIAN_POINT ( 'NONE',  ( -4.800000000000024691, 12.50000000000000000, 0.2813168883297361700 ) ) ;
#47987 = DIRECTION ( 'NONE',  ( -4.274815082592931898E-19, -0.9999939076577903929, -0.003490651415223739937 ) ) ;
#47988 = VERTEX_POINT ( 'NONE', #44250 ) ;
#47989 = CARTESIAN_POINT ( 'NONE',  ( -10.60000000000000320, 12.50000000000000000, -4.741630453620010677 ) ) ;
#47990 = DIRECTION ( 'NONE',  ( 0.000000000000000000, 1.000000000000000000, 0.000000000000000000 ) ) ;
#47991 = DIRECTION ( 'NONE',  ( 0.000000000000000000, 1.000000000000000000, 0.000000000000000000 ) ) ;
#47992 = CONICAL_SURFACE ( 'NONE', #52105, 0.1000000000000002554, 0.003490658503988666988 ) ;
#47993 = DIRECTION ( 'NONE',  ( 0.000000000000000000, -0.9999939076577903929, 0.003490651415223739937 ) ) ;
#47994 = DIRECTION ( 'NONE',  ( 0.000000000000000000, 0.000000000000000000, 1.000000000000000000 ) ) ;
#47995 = DIRECTION ( 'NONE',  ( -0.000000000000000000, -1.000000000000000000, -0.000000000000000000 ) ) ;
#47996 = VECTOR ( 'NONE', #99132, 1000.000000000000000 ) ;
#47997 = CONICAL_SURFACE ( 'NONE', #64704, 0.1000000000000002554, 0.003490658503988666988 ) ;
#47998 = VERTEX_POINT ( 'NONE', #84823 ) ;
#47999 = ORIENTED_EDGE ( 'NONE', *, *, #19285, .F. ) ;
#48000 = ORIENTED_EDGE ( 'NONE', *, *, #34382, .T. ) ;
#48001 = VERTEX_POINT ( 'NONE', #65164 ) ;
#48002 = CARTESIAN_POINT ( 'NONE',  ( 2.099999999999949463, 2.500000000000000000, -3.737306695894649700 ) ) ;
#48003 = LINE ( 'NONE', #115405, #44887 ) ;
#48004 = DIRECTION ( 'NONE',  ( -0.000000000000000000, 1.000000000000000000, -0.000000000000000000 ) ) ;
#48005 = ORIENTED_EDGE ( 'NONE', *, *, #13351, .T. ) ;
#48006 = FACE_BOUND ( 'NONE', #84582, .T. ) ;
#48007 = ORIENTED_EDGE ( 'NONE', *, *, #9839, .F. ) ;
#48008 = DIRECTION ( 'NONE',  ( -0.000000000000000000, 1.000000000000000000, -0.000000000000000000 ) ) ;
#48009 = DIRECTION ( 'NONE',  ( -4.274815082592931898E-19, -0.9999939076577903929, -0.003490651415223739937 ) ) ;
#48011 = CONICAL_SURFACE ( 'NONE', #129592, 0.09999999999999982514, 0.003490658503988666988 ) ;
#48010 = AXIS2_PLACEMENT_3D ( 'NONE', #3621, #43567, #123388 ) ;
#48012 = CARTESIAN_POINT ( 'NONE',  ( -13.54999999999998828, 2.500000000000000000, 1.818653347947325472 ) ) ;
#48013 = CIRCLE ( 'NONE', #121156, 0.09999999999999999167 ) ;
#48014 = EDGE_CURVE ( 'NONE', #24036, #98383, #33491, .T. ) ;
#48015 = CARTESIAN_POINT ( 'NONE',  ( 14.54999999999989235, 2.500000000000000000, -2.065063509461102065 ) ) ;
#48016 = DIRECTION ( 'NONE',  ( 0.000000000000000000, 1.000000000000000000, 0.000000000000000000 ) ) ;
#48017 = LINE ( 'NONE', #16586, #41251 ) ;
#48018 = CARTESIAN_POINT ( 'NONE',  ( -12.09999999999999609, 12.50000000000000000, -4.330127018922198978 ) ) ;
#48019 = PLANE ( 'NONE',  #93115 ) ;
#48020 = DIRECTION ( 'NONE',  ( 0.000000000000000000, 0.000000000000000000, -1.000000000000000000 ) ) ;
#48021 = CIRCLE ( 'NONE', #12494, 0.06509327318403745899 ) ;
#48022 = FACE_OUTER_BOUND ( 'NONE', #44531, .T. ) ;
#48023 = EDGE_CURVE ( 'NONE', #32647, #92549, #43868, .T. ) ;
#48024 = AXIS2_PLACEMENT_3D ( 'NONE', #120050, #59210, #110851 ) ;
#48025 = ORIENTED_EDGE ( 'NONE', *, *, #100556, .F. ) ;
#48026 = ORIENTED_EDGE ( 'NONE', *, *, #66211, .F. ) ;
#48027 = VECTOR ( 'NONE', #128466, 1000.000000000000000 ) ;
#48028 = EDGE_LOOP ( 'NONE', ( #8412, #101481 ) ) ;
#48029 = ORIENTED_EDGE ( 'NONE', *, *, #124328, .F. ) ;
#48030 = CARTESIAN_POINT ( 'NONE',  ( 16.55874544816221317, -0.4845305829210151960, -6.091953208799018249 ) ) ;
#48031 = CARTESIAN_POINT ( 'NONE',  ( -2.100000000000033396, 2.500000000000000000, -5.022947341949754119 ) ) ;
#48033 = ORIENTED_EDGE ( 'NONE', *, *, #121232, .F. ) ;
#48032 = EDGE_LOOP ( 'NONE', ( #89799, #47380 ) ) ;
#48034 = EDGE_LOOP ( 'NONE', ( #28247, #11136, #115320, #76080 ) ) ;
#48035 = DIRECTION ( 'NONE',  ( 0.000000000000000000, 0.000000000000000000, 1.000000000000000000 ) ) ;
#48036 = LINE ( 'NONE', #77478, #66436 ) ;
#48037 = CARTESIAN_POINT ( 'NONE',  ( -5.200000000000022382, 12.50000000000000000, 0.3464101615137735735 ) ) ;
#48038 = CARTESIAN_POINT ( 'NONE',  ( 0.8499999999999536815, 2.500000000000000000, 5.902370205355745192 ) ) ;
#48039 = VECTOR ( 'NONE', #121272, 1000.000000000000000 ) ;
#48040 = CARTESIAN_POINT ( 'NONE',  ( 0.5999999999999551248, 12.50000000000000000, -4.741630453620016006 ) ) ;
#48041 = DIRECTION ( 'NONE',  ( 0.000000000000000000, 0.000000000000000000, 1.000000000000000000 ) ) ;
#48042 = ORIENTED_EDGE ( 'NONE', *, *, #41010, .T. ) ;
#48043 = PLANE ( 'NONE',  #60170 ) ;
#48044 = ORIENTED_EDGE ( 'NONE', *, *, #13774, .T. ) ;
#48045 = EDGE_LOOP ( 'NONE', ( #34479, #8207 ) ) ;
#48046 = ORIENTED_EDGE ( 'NONE', *, *, #75683, .T. ) ;
#48047 = DIRECTION ( 'NONE',  ( -0.000000000000000000, -1.000000000000000000, -0.000000000000000000 ) ) ;
#48048 = ORIENTED_EDGE ( 'NONE', *, *, #108666, .T. ) ;
#48049 = ORIENTED_EDGE ( 'NONE', *, *, #104781, .F. ) ;
#48050 = CARTESIAN_POINT ( 'NONE',  ( 5.599999999999931255, 2.500000000000000000, 3.883716857408420431 ) ) ;
#48051 = ADVANCED_FACE ( 'NONE', ( #126029 ), #37601, .T. ) ;
#48052 = CARTESIAN_POINT ( 'NONE',  ( -12.04999999999999716, 2.500000000000000000, -6.495190528383298911 ) ) ;
#48053 = CARTESIAN_POINT ( 'NONE',  ( 10.84999999999990905, 2.500000000000000000, 2.857883832488649301 ) ) ;
#48054 = DIRECTION ( 'NONE',  ( 0.000000000000000000, 1.000000000000000000, 0.000000000000000000 ) ) ;
#48055 = DIRECTION ( 'NONE',  ( -4.274815082592931898E-19, -0.9999939076577903929, -0.003490651415223739937 ) ) ;
#48056 = CIRCLE ( 'NONE', #116976, 0.09999999999999982514 ) ;
#48057 = ORIENTED_EDGE ( 'NONE', *, *, #23445, .T. ) ;
#48058 = DIRECTION ( 'NONE',  ( -0.000000000000000000, -1.000000000000000000, -0.000000000000000000 ) ) ;
#48059 = ADVANCED_FACE ( 'NONE', ( #126698 ), #87740, .T. ) ;
#48060 = VERTEX_POINT ( 'NONE', #38320 ) ;
#48061 = DIRECTION ( 'NONE',  ( 0.000000000000000000, 1.000000000000000000, 0.000000000000000000 ) ) ;
#48063 = AXIS2_PLACEMENT_3D ( 'NONE', #44917, #53453, #112369 ) ;
#48062 = CIRCLE ( 'NONE', #11, 0.09999999999999982514 ) ;
#48064 = ORIENTED_EDGE ( 'NONE', *, *, #92781, .T. ) ;
#48065 = CARTESIAN_POINT ( 'NONE',  ( 111.3047543057325584, 7.846687871447191931, -3.765660354317603709 ) ) ;
#48066 = CARTESIAN_POINT ( 'NONE',  ( 5.399999999999936406, 2.500000000000000000, -3.637306695894650055 ) ) ;
#48067 = VERTEX_POINT ( 'NONE', #35734 ) ;
#48069 = EDGE_CURVE ( 'NONE', #35458, #38872, #95300, .T. ) ;
#48068 = CARTESIAN_POINT ( 'NONE',  ( 4.349999999999937472, 2.500000000000000000, 6.941600689897073018 ) ) ;
#48070 = CARTESIAN_POINT ( 'NONE',  ( 10.44999999999991047, 12.50000000000000000, -6.495190528383302464 ) ) ;
#48071 = ADVANCED_FACE ( 'NONE', ( #95941 ), #100284, .T. ) ;
#48072 = VERTEX_POINT ( 'NONE', #78250 ) ;
#48074 = AXIS2_PLACEMENT_3D ( 'NONE', #117148, #67396, #127639 ) ;
#48073 = AXIS2_PLACEMENT_3D ( 'NONE', #55165, #26996, #125812 ) ;
#48075 = ADVANCED_FACE ( 'NONE', ( #37027 ), #114931, .T. ) ;
#48076 = CARTESIAN_POINT ( 'NONE',  ( 1.249999999999952038, 12.50000000000000000, -1.537336459617587581 ) ) ;
#48077 = ORIENTED_EDGE ( 'NONE', *, *, #76204, .F. ) ;
#48078 = EDGE_LOOP ( 'NONE', ( #55559, #107209, #104417, #31414 ) ) ;
#48079 = CARTESIAN_POINT ( 'NONE',  ( 97.50000000000000000, 0.000000000000000000, 0.000000000000000000 ) ) ;
#48080 = DIRECTION ( 'NONE',  ( -0.000000000000000000, -1.000000000000000000, -0.000000000000000000 ) ) ;
#48081 = ADVANCED_FACE ( 'NONE', ( #17354 ), #76950, .T. ) ;
#48082 = CARTESIAN_POINT ( 'NONE',  ( 185.5052083336747444, -6.551208109652278289, 3.782341765624995134 ) ) ;
#48083 = DIRECTION ( 'NONE',  ( 0.000000000000000000, 0.000000000000000000, 1.000000000000000000 ) ) ;
#48084 = DIRECTION ( 'NONE',  ( 0.000000000000000000, 0.000000000000000000, 1.000000000000000000 ) ) ;
#48085 = CARTESIAN_POINT ( 'NONE',  ( 5.849999999999933031, 2.500000000000000000, 7.188010851410848723 ) ) ;
#48086 = VERTEX_POINT ( 'NONE', #76306 ) ;
#48087 = DIRECTION ( 'NONE',  ( 0.000000000000000000, 0.000000000000000000, 1.000000000000000000 ) ) ;
#48088 = CARTESIAN_POINT ( 'NONE',  ( -3.350000000000028955, 2.500000000000000000, 7.288010851410849256 ) ) ;
#48089 = VECTOR ( 'NONE', #46720, 1000.000000000000000 ) ;
#48090 = ORIENTED_EDGE ( 'NONE', *, *, #109409, .F. ) ;
#48091 = DIRECTION ( 'NONE',  ( 0.000000000000000000, 1.000000000000000000, 0.000000000000000000 ) ) ;
#48092 = CARTESIAN_POINT ( 'NONE',  ( -9.400000000000007461, 12.50000000000000000, 0.3464101615137735735 ) ) ;
#48093 = DIRECTION ( 'NONE',  ( 0.000000000000000000, 0.000000000000000000, 1.000000000000000000 ) ) ;
#48094 = CARTESIAN_POINT ( 'NONE',  ( 11.64999999999990798, 12.50000000000000000, 5.802370205355744659 ) ) ;
#48095 = DIRECTION ( 'NONE',  ( 0.000000000000000000, 0.000000000000000000, 1.000000000000000000 ) ) ;
#48096 = ORIENTED_EDGE ( 'NONE', *, *, #51806, .F. ) ;
#48097 = AXIS2_PLACEMENT_3D ( 'NONE', #115703, #65969, #26053 ) ;
#48098 = CARTESIAN_POINT ( 'NONE',  ( 9.349999999999916156, 2.500000000000000000, -1.818653347947326138 ) ) ;
#48099 = CARTESIAN_POINT ( 'NONE',  ( 14.54999999999989235, 2.500000000000000000, -2.065063509461102065 ) ) ;
#48100 = CIRCLE ( 'NONE', #121260, 0.06509327318403745899 ) ;
#48101 = VERTEX_POINT ( 'NONE', #118153 ) ;
#48102 = EDGE_CURVE ( 'NONE', #28983, #97899, #56447, .T. ) ;
#48103 = FACE_OUTER_BOUND ( 'NONE', #32527, .T. ) ;
#48104 = CIRCLE ( 'NONE', #2119, 0.06509327318403745899 ) ;
#48105 = AXIS2_PLACEMENT_3D ( 'NONE', #37346, #58910, #8495 ) ;
#48106 = VERTEX_POINT ( 'NONE', #87393 ) ;
#48107 = ORIENTED_EDGE ( 'NONE', *, *, #78409, .T. ) ;
#48108 = CARTESIAN_POINT ( 'NONE',  ( -12.09999999999999609, 12.50000000000000000, -0.6277270498435126855 ) ) ;
#48109 = EDGE_CURVE ( 'NONE', #13047, #39415, #4117, .T. ) ;
#48110 = EDGE_CURVE ( 'NONE', #45696, #10025, #110733, .T. ) ;
#48111 = VERTEX_POINT ( 'NONE', #127347 ) ;
#48112 = DIRECTION ( 'NONE',  ( 0.000000000000000000, 0.000000000000000000, 1.000000000000000000 ) ) ;
#48114 = EDGE_CURVE ( 'NONE', #64820, #24778, #105101, .T. ) ;
#48113 = CARTESIAN_POINT ( 'NONE',  ( -2.900000000000030553, 12.50000000000000000, 5.022947341949748790 ) ) ;
#48116 = EDGE_CURVE ( 'NONE', #12607, #117167, #85697, .T. ) ;
#48115 = CIRCLE ( 'NONE', #123323, 0.06509327318403745899 ) ;
#48117 = CARTESIAN_POINT ( 'NONE',  ( -2.100000000000033396, 2.500000000000000000, -4.922947341949753586 ) ) ;
#48118 = ORIENTED_EDGE ( 'NONE', *, *, #109246, .F. ) ;
#48119 = PLANE ( 'NONE',  #25755 ) ;
#48120 = ADVANCED_FACE ( 'NONE', ( #16066 ), #104475, .T. ) ;
#48122 = ORIENTED_EDGE ( 'NONE', *, *, #119423, .F. ) ;
#48121 = CARTESIAN_POINT ( 'NONE',  ( 9.799999999999915445, 12.50000000000000000, 3.983716857408420964 ) ) ;
#48123 = CARTESIAN_POINT ( 'NONE',  ( -9.350000000000006750, 12.50000000000000000, -1.818653347947325916 ) ) ;
#48124 = CARTESIAN_POINT ( 'NONE',  ( -10.80000000000000249, 12.50000000000000000, -4.265033745738159965 ) ) ;
#48125 = ORIENTED_EDGE ( 'NONE', *, *, #127445, .F. ) ;
#48126 = ADVANCED_FACE ( 'NONE', ( #127973 ), #7544, .T. ) ;
#48127 = EDGE_CURVE ( 'NONE', #110840, #58034, #94014, .T. ) ;
#48128 = VERTEX_POINT ( 'NONE', #16707 ) ;
#48129 = ORIENTED_EDGE ( 'NONE', *, *, #25479, .T. ) ;
#48130 = CARTESIAN_POINT ( 'NONE',  ( -5.450000000000023270, 12.50000000000000000, -2.099970236277064473 ) ) ;
#48131 = DIRECTION ( 'NONE',  ( 0.000000000000000000, 0.000000000000000000, 1.000000000000000000 ) ) ;
#48132 = DIRECTION ( 'NONE',  ( -4.274815082592931898E-19, -0.9999939076577903929, -0.003490651415223739937 ) ) ;
#48133 = FACE_BOUND ( 'NONE', #23581, .T. ) ;
#48134 = EDGE_LOOP ( 'NONE', ( #22292, #85405, #100527, #17175 ) ) ;
#48135 = FACE_OUTER_BOUND ( 'NONE', #59929, .T. ) ;
#48136 = DIRECTION ( 'NONE',  ( -0.000000000000000000, -1.000000000000000000, -0.000000000000000000 ) ) ;
#48137 = EDGE_LOOP ( 'NONE', ( #38813, #97530 ) ) ;
#48138 = CARTESIAN_POINT ( 'NONE',  ( -11.64999999999999858, 2.500000000000000000, -5.802370205355746435 ) ) ;
#48139 = CARTESIAN_POINT ( 'NONE',  ( 17.49862860983209956, 2.500000000000000000, 4.081131818001135336 ) ) ;
#48141 = CARTESIAN_POINT ( 'NONE',  ( 11.84999999999990727, 12.50000000000000000, 6.906693963081109722 ) ) ;
#48140 = AXIS2_PLACEMENT_3D ( 'NONE', #26478, #4233, #104386 ) ;
#48142 = DIRECTION ( 'NONE',  ( -0.000000000000000000, -1.000000000000000000, -0.000000000000000000 ) ) ;
#48143 = AXIS2_PLACEMENT_3D ( 'NONE', #105826, #15499, #24696 ) ;
#48144 = PLANE ( 'NONE',  #1250 ) ;
#48145 = LINE ( 'NONE', #40927, #2307 ) ;
#48147 = AXIS2_PLACEMENT_3D ( 'NONE', #122031, #32388, #72293 ) ;
#48146 = VECTOR ( 'NONE', #123274, 1000.000000000000000 ) ;
#48148 = ORIENTED_EDGE ( 'NONE', *, *, #75758, .T. ) ;
#48149 = ORIENTED_EDGE ( 'NONE', *, *, #71309, .T. ) ;
#48150 = ORIENTED_EDGE ( 'NONE', *, *, #55734, .T. ) ;
#48151 = ORIENTED_EDGE ( 'NONE', *, *, #123783, .F. ) ;
#48152 = ORIENTED_EDGE ( 'NONE', *, *, #118434, .T. ) ;
#48153 = LINE ( 'NONE', #78916, #111195 ) ;
#48154 = DIRECTION ( 'NONE',  ( 0.000000000000000000, -0.000000000000000000, 1.000000000000000000 ) ) ;
#48155 = ORIENTED_EDGE ( 'NONE', *, *, #123324, .T. ) ;
#48156 = FACE_BOUND ( 'NONE', #30535, .T. ) ;
#48157 = DIRECTION ( 'NONE',  ( 0.000000000000000000, 0.000000000000000000, 1.000000000000000000 ) ) ;
#48158 = CARTESIAN_POINT ( 'NONE',  ( 11.24999999999990941, 2.500000000000000000, -1.372243186433550033 ) ) ;
#48159 = DIRECTION ( 'NONE',  ( -0.000000000000000000, 1.000000000000000000, -0.000000000000000000 ) ) ;
#48160 = DIRECTION ( 'NONE',  ( 0.000000000000000000, 0.000000000000000000, -1.000000000000000000 ) ) ;
#48161 = CARTESIAN_POINT ( 'NONE',  ( 5.849999999999931255, 12.50000000000000000, 2.857883832488649301 ) ) ;
#48162 = ORIENTED_EDGE ( 'NONE', *, *, #92999, .F. ) ;
#48163 = DIRECTION ( 'NONE',  ( 0.000000000000000000, 0.000000000000000000, -1.000000000000000000 ) ) ;
#48164 = ORIENTED_EDGE ( 'NONE', *, *, #16235, .F. ) ;
#48165 = EDGE_CURVE ( 'NONE', #2125, #104031, #91967, .T. ) ;
#48166 = ORIENTED_EDGE ( 'NONE', *, *, #19461, .T. ) ;
#48167 = VERTEX_POINT ( 'NONE', #29774 ) ;
#48168 = CARTESIAN_POINT ( 'NONE',  ( -4.350000000000023626, 12.50000000000000000, -1.818653347947325916 ) ) ;
#48169 = CARTESIAN_POINT ( 'NONE',  ( -8.100000000000010303, 12.50000000000000000, 4.741630453620009789 ) ) ;
#48170 = FACE_OUTER_BOUND ( 'NONE', #89866, .T. ) ;
#48171 = ORIENTED_EDGE ( 'NONE', *, *, #97617, .T. ) ;
#48172 = DIRECTION ( 'NONE',  ( 0.000000000000000000, 0.000000000000000000, 1.000000000000000000 ) ) ;
#48173 = VECTOR ( 'NONE', #122422, 1000.000000000000000 ) ;
#48174 = CARTESIAN_POINT ( 'NONE',  ( 1.049999999999954081, 12.50000000000000000, -6.148780366869526226 ) ) ;
#48175 = AXIS2_PLACEMENT_3D ( 'NONE', #73791, #32623, #92143 ) ;
#48176 = LINE ( 'NONE', #59307, #123034 ) ;
#48177 = CARTESIAN_POINT ( 'NONE',  ( 184.0677083336747160, -4.367472073101514418, -7.564683531250002702 ) ) ;
#48178 = DIRECTION ( 'NONE',  ( 0.000000000000000000, 0.000000000000000000, 1.000000000000000000 ) ) ;
#48179 = DIRECTION ( 'NONE',  ( 0.000000000000000000, 1.000000000000000000, 0.000000000000000000 ) ) ;
#48180 = DIRECTION ( 'NONE',  ( -0.000000000000000000, -1.000000000000000000, -0.000000000000000000 ) ) ;
#48181 = ORIENTED_EDGE ( 'NONE', *, *, #82389, .T. ) ;
#48182 = CARTESIAN_POINT ( 'NONE',  ( -7.500000000000015099, 12.50000000000000000, -0.7579135962115916003 ) ) ;
#48183 = AXIS2_PLACEMENT_3D ( 'NONE', #99305, #20739, #70479 ) ;
#48184 = ORIENTED_EDGE ( 'NONE', *, *, #77817, .T. ) ;
#48185 = ORIENTED_EDGE ( 'NONE', *, *, #105000, .T. ) ;
#48186 = DIRECTION ( 'NONE',  ( 0.000000000000000000, 0.000000000000000000, -1.000000000000000000 ) ) ;
#48187 = CARTESIAN_POINT ( 'NONE',  ( 4.999999999999936939, 12.50000000000000000, -0.6928203230275541413 ) ) ;
#48188 = DIRECTION ( 'NONE',  ( -0.000000000000000000, 1.000000000000000000, -0.000000000000000000 ) ) ;
#48189 = ORIENTED_EDGE ( 'NONE', *, *, #35542, .T. ) ;
#48190 = ORIENTED_EDGE ( 'NONE', *, *, #123460, .F. ) ;
#48191 = CONICAL_SURFACE ( 'NONE', #121342, 0.1000000000000000056, 0.003490658503988666988 ) ;
#48192 = DIRECTION ( 'NONE',  ( 0.000000000000000000, 1.000000000000000000, 0.000000000000000000 ) ) ;
#48193 = AXIS2_PLACEMENT_3D ( 'NONE', #35883, #75791, #126193 ) ;
#48194 = LINE ( 'NONE', #88767, #116358 ) ;
#48195 = DIRECTION ( 'NONE',  ( 0.000000000000000000, 0.000000000000000000, 1.000000000000000000 ) ) ;
#48196 = ORIENTED_EDGE ( 'NONE', *, *, #127729, .F. ) ;
#48197 = ORIENTED_EDGE ( 'NONE', *, *, #215, .F. ) ;
#48198 = DIRECTION ( 'NONE',  ( 0.000000000000000000, 0.000000000000000000, 1.000000000000000000 ) ) ;
#48199 = CIRCLE ( 'NONE', #44013, 0.09999999999999982514 ) ;
#48200 = EDGE_LOOP ( 'NONE', ( #100185, #42595, #45490, #37500 ) ) ;
#48201 = CARTESIAN_POINT ( 'NONE',  ( 11.04999999999990834, 2.500000000000000000, 1.918653347947321564 ) ) ;
#48202 = ADVANCED_FACE ( 'NONE', ( #91274 ), #64767, .T. ) ;
#48203 = DIRECTION ( 'NONE',  ( 0.000000000000000000, -0.9999939076577903929, 0.003490651415223739937 ) ) ;
#48204 = VERTEX_POINT ( 'NONE', #50701 ) ;
#48205 = CARTESIAN_POINT ( 'NONE',  ( 8.749999999999953815, 12.50000000000000000, 6.495190528383297135 ) ) ;
#48206 = CARTESIAN_POINT ( 'NONE',  ( 7.049999999999928768, 2.500000000000000000, 6.495190528383297135 ) ) ;
#48207 = VECTOR ( 'NONE', #108338, 1000.000000000000000 ) ;
#48208 = CARTESIAN_POINT ( 'NONE',  ( -7.499999999999980460, 2.500000000000000000, -4.230127018922201998 ) ) ;
#48209 = EDGE_CURVE ( 'NONE', #87979, #26681, #121202, .T. ) ;
#48210 = DIRECTION ( 'NONE',  ( 0.000000000000000000, 0.000000000000000000, 1.000000000000000000 ) ) ;
#48211 = EDGE_CURVE ( 'NONE', #51042, #27361, #108681, .T. ) ;
#48212 = ORIENTED_EDGE ( 'NONE', *, *, #52723, .F. ) ;
#48213 = CARTESIAN_POINT ( 'NONE',  ( -2.700000000000029932, 2.500000000000000000, -0.4464101615137782142 ) ) ;
#48214 = ADVANCED_FACE ( 'NONE', ( #41551 ), #46007, .T. ) ;
#48215 = ORIENTED_EDGE ( 'NONE', *, *, #81648, .F. ) ;
#48216 = EDGE_CURVE ( 'NONE', #44822, #80384, #18666, .T. ) ;
#48217 = ORIENTED_EDGE ( 'NONE', *, *, #53399, .F. ) ;
#48218 = EDGE_CURVE ( 'NONE', #74651, #48167, #110269, .T. ) ;
#48219 = DIRECTION ( 'NONE',  ( 0.000000000000000000, 1.000000000000000000, 0.000000000000000000 ) ) ;
#48220 = CARTESIAN_POINT ( 'NONE',  ( 107.5000000000000142, -1.500000000000000222, 1.322875655532295136 ) ) ;
#48221 = DIRECTION ( 'NONE',  ( 0.000000000000000000, 0.000000000000000000, -1.000000000000000000 ) ) ;
#48222 = EDGE_CURVE ( 'NONE', #102784, #25279, #10474, .T. ) ;
#48223 = DIRECTION ( 'NONE',  ( 0.000000000000000000, 0.000000000000000000, 1.000000000000000000 ) ) ;
#48224 = DIRECTION ( 'NONE',  ( -0.000000000000000000, -1.000000000000000000, -0.000000000000000000 ) ) ;
#48225 = CARTESIAN_POINT ( 'NONE',  ( -10.65000000000000391, 12.50000000000000000, -6.841600689897075149 ) ) ;
#48226 = DIRECTION ( 'NONE',  ( 0.000000000000000000, 0.000000000000000000, -1.000000000000000000 ) ) ;
#48227 = CARTESIAN_POINT ( 'NONE',  ( -1.650000000000034772, 2.500000000000000000, 1.572243186433545548 ) ) ;
#48228 = CARTESIAN_POINT ( 'NONE',  ( -6.650000000000019007, 2.500000000000000000, -1.372243186433550033 ) ) ;
#48229 = AXIS2_PLACEMENT_3D ( 'NONE', #84089, #86010, #124021 ) ;
#48230 = CIRCLE ( 'NONE', #52427, 0.09999999999999982514 ) ;
#48231 = AXIS2_PLACEMENT_3D ( 'NONE', #33094, #23236, #110339 ) ;
#48232 = EDGE_CURVE ( 'NONE', #61265, #3657, #78897, .T. ) ;
#48233 = FACE_OUTER_BOUND ( 'NONE', #48587, .T. ) ;
#48234 = AXIS2_PLACEMENT_3D ( 'NONE', #59714, #29577, #119246 ) ;
#48235 = EDGE_LOOP ( 'NONE', ( #21375, #58500, #69522, #71074 ) ) ;
#48236 = CARTESIAN_POINT ( 'NONE',  ( 13.94999999999989448, 2.500000000000000000, -2.511473670974877948 ) ) ;
#48237 = CIRCLE ( 'NONE', #121391, 0.06509327318403745899 ) ;
#48238 = LINE ( 'NONE', #109060, #20741 ) ;
#48239 = DIRECTION ( 'NONE',  ( -1.000000000000000000, 0.000000000000000000, 0.000000000000000000 ) ) ;
#48240 = CARTESIAN_POINT ( 'NONE',  ( 2.099999999999950351, 12.50000000000000000, -0.6928203230275541413 ) ) ;
#48241 = DIRECTION ( 'NONE',  ( 0.000000000000000000, -0.9999939076577903929, 0.003490651415223739937 ) ) ;
#48242 = ORIENTED_EDGE ( 'NONE', *, *, #25418, .F. ) ;
#48243 = DIRECTION ( 'NONE',  ( 0.000000000000000000, 0.000000000000000000, 1.000000000000000000 ) ) ;
#48244 = CARTESIAN_POINT ( 'NONE',  ( 185.4583333333333428, 4.445597072760175905, 7.699999999999896261 ) ) ;
#48246 = EDGE_LOOP ( 'NONE', ( #21215, #67121, #101889, #93969 ) ) ;
#48245 = CARTESIAN_POINT ( 'NONE',  ( -6.850000000000013856, 2.500000000000000000, 1.718653347947321386 ) ) ;
#48247 = EDGE_LOOP ( 'NONE', ( #8171, #96298 ) ) ;
#48248 = FACE_OUTER_BOUND ( 'NONE', #12102, .T. ) ;
#48249 = EDGE_LOOP ( 'NONE', ( #40845, #42273 ) ) ;
#48250 = ORIENTED_EDGE ( 'NONE', *, *, #55020, .T. ) ;
#48251 = EDGE_LOOP ( 'NONE', ( #69029, #75652, #20698, #117940 ) ) ;
#48252 = CARTESIAN_POINT ( 'NONE',  ( -11.25000000000000000, 12.50000000000000000, -7.253104124594887736 ) ) ;
#48253 = EDGE_CURVE ( 'NONE', #4956, #46788, #98497, .T. ) ;
#48254 = ADVANCED_FACE ( 'NONE', ( #21237 ), #50213, .T. ) ;
#48255 = DIRECTION ( 'NONE',  ( 0.000000000000000000, 1.000000000000000000, 0.000000000000000000 ) ) ;
#48257 = EDGE_CURVE ( 'NONE', #41439, #59702, #12626, .T. ) ;
#48256 = CARTESIAN_POINT ( 'NONE',  ( -1.322875655532295136, -1.500000000000000222, -5.000000000000004441 ) ) ;
#48258 = CARTESIAN_POINT ( 'NONE',  ( 6.649999999999930189, 2.500000000000000000, 7.088010851410848190 ) ) ;
#48259 = AXIS2_PLACEMENT_3D ( 'NONE', #128427, #28923, #19064 ) ;
#48260 = VERTEX_POINT ( 'NONE', #89973 ) ;
#48261 = AXIS2_PLACEMENT_3D ( 'NONE', #120174, #1669, #41634 ) ;
#48262 = EDGE_CURVE ( 'NONE', #55743, #594, #46094, .T. ) ;
#48263 = DIRECTION ( 'NONE',  ( -0.000000000000000000, -1.000000000000000000, -0.000000000000000000 ) ) ;
#48264 = ORIENTED_EDGE ( 'NONE', *, *, #19506, .T. ) ;
#48265 = CARTESIAN_POINT ( 'NONE',  ( -1.450000000000036371, 2.500000000000000000, 2.411473670974873862 ) ) ;
#48266 = CARTESIAN_POINT ( 'NONE',  ( 14.93814515115567865, -2.500000000000000444, -6.173787963789434841 ) ) ;
#48267 = CARTESIAN_POINT ( 'NONE',  ( 18.20334136264090574, 2.532871263997065636, 4.817802756304448764 ) ) ;
#48268 = CARTESIAN_POINT ( 'NONE',  ( -4.600000000000024514, 12.50000000000000000, 3.637306695894644726 ) ) ;
#48269 = EDGE_CURVE ( 'NONE', #113705, #77714, #125500, .T. ) ;
#48270 = FACE_OUTER_BOUND ( 'NONE', #36132, .T. ) ;
#48271 = AXIS2_PLACEMENT_3D ( 'NONE', #46989, #67898, #16832 ) ;
#48272 = EDGE_CURVE ( 'NONE', #101260, #91108, #119431, .T. ) ;
#48273 = ORIENTED_EDGE ( 'NONE', *, *, #76882, .F. ) ;
#48274 = AXIS2_PLACEMENT_3D ( 'NONE', #125782, #96324, #76063 ) ;
#48275 = ADVANCED_FACE ( 'NONE', ( #99170 ), #20609, .T. ) ;
#48276 = EDGE_CURVE ( 'NONE', #27106, #113976, #69062, .T. ) ;
#48277 = VERTEX_POINT ( 'NONE', #120099 ) ;
#48278 = ORIENTED_EDGE ( 'NONE', *, *, #6194, .F. ) ;
#48279 = ORIENTED_EDGE ( 'NONE', *, *, #34811, .F. ) ;
#48280 = ORIENTED_EDGE ( 'NONE', *, *, #41521, .T. ) ;
#48281 = FACE_OUTER_BOUND ( 'NONE', #65810, .T. ) ;
#48282 = DIRECTION ( 'NONE',  ( -0.000000000000000000, -1.000000000000000000, -0.000000000000000000 ) ) ;
#48283 = FACE_OUTER_BOUND ( 'NONE', #53335, .T. ) ;
#48284 = FACE_BOUND ( 'NONE', #93639, .T. ) ;
#48285 = CARTESIAN_POINT ( 'NONE',  ( -1.450000000000035039, 12.50000000000000000, -2.511473670974877948 ) ) ;
#48286 = DIRECTION ( 'NONE',  ( -0.000000000000000000, 1.000000000000000000, -0.000000000000000000 ) ) ;
#48287 = EDGE_CURVE ( 'NONE', #83720, #86121, #956, .T. ) ;
#48288 = FACE_OUTER_BOUND ( 'NONE', #84963, .T. ) ;
#48289 = DIRECTION ( 'NONE',  ( 0.000000000000000000, 0.000000000000000000, 1.000000000000000000 ) ) ;
#48290 = AXIS2_PLACEMENT_3D ( 'NONE', #1884, #12347, #53581 ) ;
#48291 = AXIS2_PLACEMENT_3D ( 'NONE', #75629, #43631, #46185 ) ;
#48292 = CARTESIAN_POINT ( 'NONE',  ( 185.2968750003414300, 8.734944146203032389, 5.348610694689227483E-16 ) ) ;
#48293 = DIRECTION ( 'NONE',  ( 0.000000000000000000, 0.000000000000000000, -1.000000000000000000 ) ) ;
#48294 = CARTESIAN_POINT ( 'NONE',  ( -1.650000000000034328, 2.500000000000000000, -2.165063509461101710 ) ) ;
#48295 = CONICAL_SURFACE ( 'NONE', #121440, 0.09999999999999982514, 0.003490658503988666988 ) ;
#48296 = FACE_OUTER_BOUND ( 'NONE', #8206, .T. ) ;
#48297 = VERTEX_POINT ( 'NONE', #70996 ) ;
#48298 = AXIS2_PLACEMENT_3D ( 'NONE', #123321, #52015, #93862 ) ;
#48299 = ORIENTED_EDGE ( 'NONE', *, *, #39706, .T. ) ;
#48300 = VERTEX_POINT ( 'NONE', #110899 ) ;
#48301 = EDGE_LOOP ( 'NONE', ( #107340, #33396 ) ) ;
#48302 = DIRECTION ( 'NONE',  ( 0.000000000000000000, -0.000000000000000000, 1.000000000000000000 ) ) ;
#48303 = EDGE_CURVE ( 'NONE', #72180, #4130, #61171, .T. ) ;
#48304 = FACE_BOUND ( 'NONE', #33056, .T. ) ;
#48305 = CARTESIAN_POINT ( 'NONE',  ( -8.100000000000013856, 12.50000000000000000, -4.741630453620015118 ) ) ;
#48306 = ORIENTED_EDGE ( 'NONE', *, *, #7555, .F. ) ;
#48307 = FACE_OUTER_BOUND ( 'NONE', #122275, .T. ) ;
#48308 = PLANE ( 'NONE',  #47314 ) ;
#48309 = DIRECTION ( 'NONE',  ( -0.000000000000000000, -1.000000000000000000, -0.000000000000000000 ) ) ;
#48310 = DIRECTION ( 'NONE',  ( 0.000000000000000000, 0.000000000000000000, 1.000000000000000000 ) ) ;
#48311 = EDGE_LOOP ( 'NONE', ( #13031, #60879, #122369, #52991 ) ) ;
#48312 = DIRECTION ( 'NONE',  ( -1.000000000000000000, -0.000000000000000000, -0.000000000000000000 ) ) ;
#48313 = CARTESIAN_POINT ( 'NONE',  ( 17.50000000000000000, 2.500000000000000000, -2.922290670089280340 ) ) ;
#48314 = ADVANCED_FACE ( 'NONE', ( #43478 ), #58618, .T. ) ;
#48315 = ORIENTED_EDGE ( 'NONE', *, *, #75454, .F. ) ;
#48316 = ORIENTED_EDGE ( 'NONE', *, *, #44375, .T. ) ;
#48317 = AXIS2_PLACEMENT_3D ( 'NONE', #27592, #76717, #96999 ) ;
#48318 = CARTESIAN_POINT ( 'NONE',  ( -7.100000000000017408, 2.500000000000000000, -3.637306695894650055 ) ) ;
#48319 = CONICAL_SURFACE ( 'NONE', #81757, 0.09999999999999982514, 0.003490658503988666988 ) ;
#48320 = FACE_OUTER_BOUND ( 'NONE', #10064, .T. ) ;
#48321 = ORIENTED_EDGE ( 'NONE', *, *, #97288, .F. ) ;
#48322 = CARTESIAN_POINT ( 'NONE',  ( 12.89999999999989733, 2.500000000000000000, -2.385244779468109755E-15 ) ) ;
#48323 = CIRCLE ( 'NONE', #60848, 0.09999999999999982514 ) ;
#48324 = DIRECTION ( 'NONE',  ( 0.000000000000000000, 1.000000000000000000, 0.000000000000000000 ) ) ;
#48325 = ORIENTED_EDGE ( 'NONE', *, *, #94169, .T. ) ;
#48326 = DIRECTION ( 'NONE',  ( -0.000000000000000000, -1.000000000000000000, -0.000000000000000000 ) ) ;
#48327 = ORIENTED_EDGE ( 'NONE', *, *, #111770, .T. ) ;
#48328 = CIRCLE ( 'NONE', #91541, 0.1000000000000002554 ) ;
#48329 = EDGE_LOOP ( 'NONE', ( #87054, #34190, #125213, #28387 ) ) ;
#48330 = EDGE_CURVE ( 'NONE', #14341, #68963, #104316, .T. ) ;
#48331 = DIRECTION ( 'NONE',  ( -0.000000000000000000, 1.000000000000000000, -0.000000000000000000 ) ) ;
#48332 = ORIENTED_EDGE ( 'NONE', *, *, #56500, .T. ) ;
#48333 = CARTESIAN_POINT ( 'NONE',  ( 8.349999999999923261, 2.500000000000000000, 2.065063509461097624 ) ) ;
#48334 = FACE_BOUND ( 'NONE', #118812, .T. ) ;
#48335 = ORIENTED_EDGE ( 'NONE', *, *, #95642, .T. ) ;
#48336 = CARTESIAN_POINT ( 'NONE',  ( 111.9573209325854606, 7.065995906185201569, 3.073256371337414361 ) ) ;
#48337 = ORIENTED_EDGE ( 'NONE', *, *, #29650, .T. ) ;
#48338 = CARTESIAN_POINT ( 'NONE',  ( -4.600000000000024514, 2.500000000000000000, 5.122947341949749323 ) ) ;
#48339 = FACE_OUTER_BOUND ( 'NONE', #102024, .T. ) ;
#48340 = FACE_OUTER_BOUND ( 'NONE', #30443, .T. ) ;
#48341 = DIRECTION ( 'NONE',  ( 0.000000000000000000, 0.000000000000000000, 1.000000000000000000 ) ) ;
#48342 = CARTESIAN_POINT ( 'NONE',  ( -1.445602896647332014E-16, 2.000000000000000000, -1.999999999999989120 ) ) ;
#48343 = VERTEX_POINT ( 'NONE', #63098 ) ;
#48344 = VERTEX_POINT ( 'NONE', #2230 ) ;
#48345 = VERTEX_POINT ( 'NONE', #53929 ) ;
#48346 = CARTESIAN_POINT ( 'NONE',  ( 1.249999999999952038, 12.50000000000000000, 5.867463478539781896 ) ) ;
#48347 = CARTESIAN_POINT ( 'NONE',  ( -13.54999999999998828, 2.500000000000000000, 1.718653347947325383 ) ) ;
#48348 = CARTESIAN_POINT ( 'NONE',  ( 194.5000000000000000, 6.123233995736766282E-16, 5.000000000000000000 ) ) ;
#48350 = VERTEX_POINT ( 'NONE', #54552 ) ;
#48349 = ORIENTED_EDGE ( 'NONE', *, *, #68001, .T. ) ;
#48351 = ORIENTED_EDGE ( 'NONE', *, *, #118536, .T. ) ;
#48352 = DIRECTION ( 'NONE',  ( 0.000000000000000000, -0.9999939076577903929, 0.003490651415223739937 ) ) ;
#48353 = AXIS2_PLACEMENT_3D ( 'NONE', #24245, #75268, #114541 ) ;
#48354 = DIRECTION ( 'NONE',  ( -0.000000000000000000, -1.000000000000000000, -0.000000000000000000 ) ) ;
#48355 = AXIS2_PLACEMENT_3D ( 'NONE', #115475, #105690, #66395 ) ;
#48356 = ADVANCED_FACE ( 'NONE', ( #12062 ), #62816, .T. ) ;
#48357 = APPLICATION_PROTOCOL_DEFINITION ( 'draft international standard', 'automotive_design', 1998, #125709 ) ;
#48358 = DIRECTION ( 'NONE',  ( 0.000000000000000000, 0.000000000000000000, 1.000000000000000000 ) ) ;
#48359 = CARTESIAN_POINT ( 'NONE',  ( -14.14999999999998792, 2.500000000000000000, 2.757883832488653209 ) ) ;
#48360 = FACE_OUTER_BOUND ( 'NONE', #66691, .T. ) ;
#48361 = DIRECTION ( 'NONE',  ( 0.000000000000000000, 0.000000000000000000, 1.000000000000000000 ) ) ;
#48362 = CARTESIAN_POINT ( 'NONE',  ( -9.550000000000006040, 2.500000000000000000, 2.265063509461097357 ) ) ;
#48363 = DIRECTION ( 'NONE',  ( 0.000000000000000000, 1.000000000000000000, 0.000000000000000000 ) ) ;
#48364 = EDGE_CURVE ( 'NONE', #7578, #34866, #77391, .T. ) ;
#48365 = ORIENTED_EDGE ( 'NONE', *, *, #51226, .F. ) ;
#48366 = VECTOR ( 'NONE', #94900, 1000.000000000000000 ) ;
#48367 = EDGE_LOOP ( 'NONE', ( #57164, #59620, #4751, #39184 ) ) ;
#48368 = FACE_OUTER_BOUND ( 'NONE', #93569, .T. ) ;
#48369 = DIRECTION ( 'NONE',  ( 0.000000000000000000, -0.9999939076577903929, 0.003490651415223739937 ) ) ;
#48370 = ADVANCED_FACE ( 'NONE', ( #111555 ), #114138, .T. ) ;
#48371 = ORIENTED_EDGE ( 'NONE', *, *, #87512, .T. ) ;
#48372 = ADVANCED_FACE ( 'NONE', ( #71630 ), #3536, .T. ) ;
#48373 = ORIENTED_EDGE ( 'NONE', *, *, #90892, .T. ) ;
#48374 = EDGE_CURVE ( 'NONE', #74697, #111968, #6342, .T. ) ;
#48375 = CARTESIAN_POINT ( 'NONE',  ( 186.1510416670080588, 4.367472073101518859, -7.564683531249999149 ) ) ;
#48377 = EDGE_CURVE ( 'NONE', #121671, #129577, #37685, .T. ) ;
#48376 = CARTESIAN_POINT ( 'NONE',  ( 13.54999999999989591, 12.50000000000000000, -1.818653347947326138 ) ) ;
#48378 = CARTESIAN_POINT ( 'NONE',  ( 8.749999999999921840, 2.500000000000000000, 2.957883832488649389 ) ) ;
#48379 = CARTESIAN_POINT ( 'NONE',  ( -3.300000000000027800, 12.50000000000000000, -4.330127018922201643 ) ) ;
#48380 = AXIS2_PLACEMENT_3D ( 'NONE', #86086, #64533, #4957 ) ;
#48381 = CARTESIAN_POINT ( 'NONE',  ( -6.250000000000015987, 2.500000000000000000, 5.902370205355745192 ) ) ;
#48382 = LINE ( 'NONE', #107944, #67655 ) ;
#48383 = AXIS2_PLACEMENT_3D ( 'NONE', #8948, #69822, #109073 ) ;
#48384 = CARTESIAN_POINT ( 'NONE',  ( 6.249999999999967137, 2.500000000000000000, 6.595190528383296780 ) ) ;
#48385 = EDGE_CURVE ( 'NONE', #17665, #34432, #110828, .T. ) ;
#48386 = AXIS2_PLACEMENT_3D ( 'NONE', #94631, #65159, #86752 ) ;
#48388 = EDGE_CURVE ( 'NONE', #113423, #123334, #71121, .T. ) ;
#48387 = CARTESIAN_POINT ( 'NONE',  ( -3.350000000000028955, 12.50000000000000000, 2.165063509461097713 ) ) ;
#48389 = EDGE_CURVE ( 'NONE', #98382, #51072, #87836, .T. ) ;
#48390 = EDGE_LOOP ( 'NONE', ( #115647, #45162 ) ) ;
#48391 = AXIS2_PLACEMENT_3D ( 'NONE', #97083, #55860, #26420 ) ;
#48392 = AXIS2_PLACEMENT_3D ( 'NONE', #94723, #44998, #102608 ) ;
#48393 = VERTEX_POINT ( 'NONE', #64385 ) ;
#48394 = EDGE_LOOP ( 'NONE', ( #10076, #19080 ) ) ;
#48395 = ORIENTED_EDGE ( 'NONE', *, *, #56592, .F. ) ;
#48396 = CARTESIAN_POINT ( 'NONE',  ( 3.749999999999976907, 2.500000000000000000, 2.065063509461097624 ) ) ;
#48397 = DIRECTION ( 'NONE',  ( 0.000000000000000000, -0.000000000000000000, 1.000000000000000000 ) ) ;
#48398 = ORIENTED_EDGE ( 'NONE', *, *, #112154, .T. ) ;
#48399 = DIRECTION ( 'NONE',  ( 0.000000000000000000, -0.9999939076577903929, 0.003490651415223739937 ) ) ;
#48400 = CARTESIAN_POINT ( 'NONE',  ( 13.94999999999989271, 2.500000000000000000, -1.718653347947326049 ) ) ;
#48401 = DIRECTION ( 'NONE',  ( 0.000000000000000000, 0.000000000000000000, 1.000000000000000000 ) ) ;
#48403 = ORIENTED_EDGE ( 'NONE', *, *, #79605, .T. ) ;
#48402 = CARTESIAN_POINT ( 'NONE',  ( -12.49999999999995914, 12.50000000000000000, -4.330127018922198978 ) ) ;
#48404 = CARTESIAN_POINT ( 'NONE',  ( 12.09999999999990550, 2.500000000000000000, -5.022947341949754119 ) ) ;
#48405 = CARTESIAN_POINT ( 'NONE',  ( 2.499999999999981792, 2.500000000000000000, 4.430127018922196847 ) ) ;
#48406 = ORIENTED_EDGE ( 'NONE', *, *, #31681, .T. ) ;
#48407 = ORIENTED_EDGE ( 'NONE', *, *, #3494, .F. ) ;
#48408 = ORIENTED_EDGE ( 'NONE', *, *, #55626, .F. ) ;
#48409 = CONICAL_SURFACE ( 'NONE', #21303, 0.09999999999999982514, 0.003490658503988666988 ) ;
#48410 = DIRECTION ( 'NONE',  ( 0.000000000000000000, -0.000000000000000000, 1.000000000000000000 ) ) ;
#48411 = CIRCLE ( 'NONE', #27552, 0.1000000000000002554 ) ;
#48412 = CIRCLE ( 'NONE', #61016, 0.06509327318403743123 ) ;
#48413 = CARTESIAN_POINT ( 'NONE',  ( 12.49999999999990408, 2.500000000000000000, -3.637306695894650055 ) ) ;
#48414 = CIRCLE ( 'NONE', #23357, 0.06509327318403743123 ) ;
#48415 = CIRCLE ( 'NONE', #58795, 0.1000000000000000472 ) ;
#48417 = EDGE_LOOP ( 'NONE', ( #120136, #83448 ) ) ;
#48416 = AXIS2_PLACEMENT_3D ( 'NONE', #20654, #100486, #32429 ) ;
#48418 = DIRECTION ( 'NONE',  ( 0.000000000000000000, 0.000000000000000000, -1.000000000000000000 ) ) ;
#48419 = DIRECTION ( 'NONE',  ( 0.000000000000000000, -0.000000000000000000, 1.000000000000000000 ) ) ;
#48420 = DIRECTION ( 'NONE',  ( 0.000000000000000000, 0.000000000000000000, 1.000000000000000000 ) ) ;
#48421 = DIRECTION ( 'NONE',  ( -0.000000000000000000, -1.000000000000000000, -0.000000000000000000 ) ) ;
#48422 = EDGE_CURVE ( 'NONE', #77184, #47267, #104574, .T. ) ;
#48423 = CIRCLE ( 'NONE', #123709, 0.06509327318403745899 ) ;
#48424 = EDGE_CURVE ( 'NONE', #79874, #64073, #13984, .T. ) ;
#48425 = VERTEX_POINT ( 'NONE', #22554 ) ;
#48426 = CARTESIAN_POINT ( 'NONE',  ( 4.399999999999940847, 2.500000000000000000, -3.983716857408426293 ) ) ;
#48427 = EDGE_CURVE ( 'NONE', #1725, #114203, #64854, .T. ) ;
#48428 = ORIENTED_EDGE ( 'NONE', *, *, #122437, .F. ) ;
#48429 = ORIENTED_EDGE ( 'NONE', *, *, #119582, .T. ) ;
#48430 = DIRECTION ( 'NONE',  ( 0.000000000000000000, 0.000000000000000000, -1.000000000000000000 ) ) ;
#48431 = CARTESIAN_POINT ( 'NONE',  ( -0.8500000000000386136, 12.50000000000000000, 1.407149913249508000 ) ) ;
#48432 = FACE_BOUND ( 'NONE', #8100, .T. ) ;
#48433 = CARTESIAN_POINT ( 'NONE',  ( 10.64999999999990976, 2.500000000000000000, -6.148780366869526226 ) ) ;
#48434 = CARTESIAN_POINT ( 'NONE',  ( 5.849999999999935696, 2.500000000000000000, -7.188010851410854052 ) ) ;
#48435 = EDGE_CURVE ( 'NONE', #80189, #11772, #2166, .T. ) ;
#48436 = CARTESIAN_POINT ( 'NONE',  ( -1.850000000000033396, 2.500000000000000000, -6.841600689897077814 ) ) ;
#48437 = ORIENTED_EDGE ( 'NONE', *, *, #49530, .F. ) ;
#48438 = DIRECTION ( 'NONE',  ( 0.000000000000000000, 1.000000000000000000, 0.000000000000000000 ) ) ;
#48439 = DIRECTION ( 'NONE',  ( -0.000000000000000000, -1.000000000000000000, -0.000000000000000000 ) ) ;
#48440 = LINE ( 'NONE', #49754, #77973 ) ;
#48441 = CARTESIAN_POINT ( 'NONE',  ( -3.350000000000031619, 2.500000000000000000, -7.088010851410853519 ) ) ;
#48442 = ORIENTED_EDGE ( 'NONE', *, *, #114050, .F. ) ;
#48443 = AXIS2_PLACEMENT_3D ( 'NONE', #73832, #74482, #103942 ) ;
#48444 = LINE ( 'NONE', #117810, #996 ) ;
#48445 = CARTESIAN_POINT ( 'NONE',  ( 183.9218750003414016, 0.000000000000000000, 7.564683531250000925 ) ) ;
#48446 = ORIENTED_EDGE ( 'NONE', *, *, #109523, .F. ) ;
#48447 = ORIENTED_EDGE ( 'NONE', *, *, #128860, .F. ) ;
#48448 = DIRECTION ( 'NONE',  ( 0.000000000000000000, -0.9999939076577903929, 0.003490651415223739937 ) ) ;
#48449 = DIRECTION ( 'NONE',  ( 0.000000000000000000, -0.9999939076577903929, 0.003490651415223739937 ) ) ;
#48450 = EDGE_CURVE ( 'NONE', #40507, #46262, #108768, .T. ) ;
#48451 = FACE_BOUND ( 'NONE', #13044, .T. ) ;
#48452 = CIRCLE ( 'NONE', #27498, 0.1000000000000002554 ) ;
#48453 = DIRECTION ( 'NONE',  ( -4.274815082592931898E-19, -0.9999939076577903929, -0.003490651415223739937 ) ) ;
#48454 = CIRCLE ( 'NONE', #407, 0.06509327318403745899 ) ;
#48455 = AXIS2_PLACEMENT_3D ( 'NONE', #14918, #96092, #84978 ) ;
#48456 = ORIENTED_EDGE ( 'NONE', *, *, #78405, .F. ) ;
#48458 = CARTESIAN_POINT ( 'NONE',  ( 1.899999999999951283, 12.50000000000000000, -3.983716857408426293 ) ) ;
#48457 = CONICAL_SURFACE ( 'NONE', #67497, 0.1000000000000002554, 0.003490658503988666988 ) ;
#48459 = VECTOR ( 'NONE', #84553, 1000.000000000000000 ) ;
#48460 = ORIENTED_EDGE ( 'NONE', *, *, #88580, .T. ) ;
#48461 = ORIENTED_EDGE ( 'NONE', *, *, #25363, .T. ) ;
#48462 = CARTESIAN_POINT ( 'NONE',  ( 3.949999999999939782, 2.500000000000000000, 2.511473670974873507 ) ) ;
#48463 = CARTESIAN_POINT ( 'NONE',  ( 185.7916666666666572, 4.445597072760120838, -7.699999999999998401 ) ) ;
#48464 = ORIENTED_EDGE ( 'NONE', *, *, #104111, .T. ) ;
#48466 = CARTESIAN_POINT ( 'NONE',  ( -9.150000000000009237, 2.500000000000000000, -6.595190528383296780 ) ) ;
#48465 = CIRCLE ( 'NONE', #90214, 0.1000000000000002554 ) ;
#48467 = CARTESIAN_POINT ( 'NONE',  ( 187.5000000000000000, 0.000000000000000000, 8.699999999999999289 ) ) ;
#48468 = CIRCLE ( 'NONE', #115340, 0.06509327318403745899 ) ;
#48469 = EDGE_CURVE ( 'NONE', #23517, #15869, #67306, .T. ) ;
#48470 = CONICAL_SURFACE ( 'NONE', #65168, 0.1000000000000000472, 0.003490658503988666988 ) ;
#48471 = AXIS2_PLACEMENT_3D ( 'NONE', #104852, #15170, #123230 ) ;
#48472 = AXIS2_PLACEMENT_3D ( 'NONE', #46227, #107068, #116250 ) ;
#48473 = DIRECTION ( 'NONE',  ( 0.000000000000000000, 0.000000000000000000, 1.000000000000000000 ) ) ;
#48474 = DIRECTION ( 'NONE',  ( 0.000000000000000000, 0.000000000000000000, 1.000000000000000000 ) ) ;
#48475 = ORIENTED_EDGE ( 'NONE', *, *, #62702, .T. ) ;
#48476 = CARTESIAN_POINT ( 'NONE',  ( -10.85000000000000142, 2.500000000000000000, 2.165063509461097713 ) ) ;
#48477 = CIRCLE ( 'NONE', #19219, 0.1000000000000002554 ) ;
#48478 = FACE_OUTER_BOUND ( 'NONE', #73482, .T. ) ;
#48479 = CARTESIAN_POINT ( 'NONE',  ( -9.400000000000009237, 12.50000000000000000, -3.983716857408421852 ) ) ;
#48480 = DIRECTION ( 'NONE',  ( 0.000000000000000000, 0.000000000000000000, -1.000000000000000000 ) ) ;
#48481 = ORIENTED_EDGE ( 'NONE', *, *, #26374, .F. ) ;
#48482 = CARTESIAN_POINT ( 'NONE',  ( 6.249999999999930722, 12.50000000000000000, 1.472243186433545459 ) ) ;
#48483 = ORIENTED_EDGE ( 'NONE', *, *, #81076, .T. ) ;
#48484 = EDGE_CURVE ( 'NONE', #1730, #50100, #125872, .T. ) ;
#48485 = CARTESIAN_POINT ( 'NONE',  ( 7.499999999999925393, 2.500000000000000000, 5.022947341949748790 ) ) ;
#48486 = VERTEX_POINT ( 'NONE', #17858 ) ;
#48487 = DIRECTION ( 'NONE',  ( 0.000000000000000000, 0.000000000000000000, -1.000000000000000000 ) ) ;
#48488 = PLANE ( 'NONE',  #24348 ) ;
#48489 = DIRECTION ( 'NONE',  ( -4.274815082592931898E-19, -0.9999939076577903929, -0.003490651415223739937 ) ) ;
#48490 = DIRECTION ( 'NONE',  ( 0.000000000000000000, 0.000000000000000000, 1.000000000000000000 ) ) ;
#48491 = ORIENTED_EDGE ( 'NONE', *, *, #128451, .T. ) ;
#48492 = DIRECTION ( 'NONE',  ( -0.000000000000000000, -1.000000000000000000, -0.000000000000000000 ) ) ;
#48493 = FACE_OUTER_BOUND ( 'NONE', #26278, .T. ) ;
#48494 = LINE ( 'NONE', #38705, #21397 ) ;
#48495 = EDGE_CURVE ( 'NONE', #92739, #123569, #121621, .T. ) ;
#48496 = PLANE ( 'NONE',  #26562 ) ;
#48497 = DIRECTION ( 'NONE',  ( -0.000000000000000000, 1.000000000000000000, -0.000000000000000000 ) ) ;
#48498 = CARTESIAN_POINT ( 'NONE',  ( -5.850000000000018296, 2.500000000000000000, 7.288010851410849256 ) ) ;
#48499 = ORIENTED_EDGE ( 'NONE', *, *, #67430, .T. ) ;
#48500 = ORIENTED_EDGE ( 'NONE', *, *, #83457, .F. ) ;
#48501 = LINE ( 'NONE', #47872, #63817 ) ;
#48502 = ORIENTED_EDGE ( 'NONE', *, *, #86480, .F. ) ;
#48503 = AXIS2_PLACEMENT_3D ( 'NONE', #10906, #61985, #29303 ) ;
#48504 = DIRECTION ( 'NONE',  ( -0.000000000000000000, -1.000000000000000000, -0.000000000000000000 ) ) ;
#48505 = AXIS2_PLACEMENT_3D ( 'NONE', #6688, #47304, #77404 ) ;
#48506 = AXIS2_PLACEMENT_3D ( 'NONE', #80581, #59673, #11173 ) ;
#48508 = EDGE_LOOP ( 'NONE', ( #39130, #78786, #108101, #33432 ) ) ;
#48507 = ORIENTED_EDGE ( 'NONE', *, *, #111458, .T. ) ;
#48509 = VERTEX_POINT ( 'NONE', #34951 ) ;
#48510 = CARTESIAN_POINT ( 'NONE',  ( 1.049999999999953637, 2.500000000000000000, -1.918653347947326004 ) ) ;
#48511 = DIRECTION ( 'NONE',  ( -0.000000000000000000, -1.000000000000000000, -0.000000000000000000 ) ) ;
#48512 = CONICAL_SURFACE ( 'NONE', #23463, 0.09999999999999982514, 0.003490658503988666988 ) ;
#48514 = CARTESIAN_POINT ( 'NONE',  ( 179.5000000000000000, -1.375000000000000000, 7.634788798650553154 ) ) ;
#48513 = AXIS2_PLACEMENT_3D ( 'NONE', #86380, #15035, #56276 ) ;
#48516 = EDGE_CURVE ( 'NONE', #97511, #36170, #116701, .T. ) ;
#48515 = CIRCLE ( 'NONE', #50550, 0.09999999999999999167 ) ;
#48517 = DIRECTION ( 'NONE',  ( 0.000000000000000000, -0.000000000000000000, 1.000000000000000000 ) ) ;
#48518 = DIRECTION ( 'NONE',  ( -0.000000000000000000, -1.000000000000000000, -0.000000000000000000 ) ) ;
#48519 = AXIS2_PLACEMENT_3D ( 'NONE', #65055, #103065, #13390 ) ;
#48520 = PLANE ( 'NONE',  #35142 ) ;
#48521 = CARTESIAN_POINT ( 'NONE',  ( -9.150000000000005684, 2.500000000000000000, 7.188010851410848723 ) ) ;
#48522 = VECTOR ( 'NONE', #87206, 1000.000000000000000 ) ;
#48523 = LINE ( 'NONE', #88431, #110507 ) ;
#48524 = EDGE_LOOP ( 'NONE', ( #22325, #128470 ) ) ;
#48525 = EDGE_CURVE ( 'NONE', #69489, #126455, #65008, .T. ) ;
#48526 = ORIENTED_EDGE ( 'NONE', *, *, #67223, .F. ) ;
#48527 = VERTEX_POINT ( 'NONE', #25750 ) ;
#48528 = DIRECTION ( 'NONE',  ( 0.000000000000000000, 1.000000000000000000, 0.000000000000000000 ) ) ;
#48529 = EDGE_CURVE ( 'NONE', #12380, #78590, #88149, .T. ) ;
#48530 = EDGE_LOOP ( 'NONE', ( #105757, #67798 ) ) ;
#48531 = EDGE_CURVE ( 'NONE', #1733, #91438, #50614, .T. ) ;
#48532 = VERTEX_POINT ( 'NONE', #7386 ) ;
#48533 = ADVANCED_FACE ( 'NONE', ( #116061 ), #48470, .T. ) ;
#48534 = CARTESIAN_POINT ( 'NONE',  ( 13.34999999999990017, 2.500000000000000000, 1.572243186433545548 ) ) ;
#48535 = EDGE_CURVE ( 'NONE', #384, #91010, #113305, .T. ) ;
#48536 = DIRECTION ( 'NONE',  ( 0.000000000000000000, 0.000000000000000000, 1.000000000000000000 ) ) ;
#48537 = DIRECTION ( 'NONE',  ( 0.000000000000000000, 1.000000000000000000, 0.000000000000000000 ) ) ;
#48538 = DIRECTION ( 'NONE',  ( 0.000000000000000000, 0.000000000000000000, -1.000000000000000000 ) ) ;
#48539 = DIRECTION ( 'NONE',  ( 0.000000000000000000, 0.000000000000000000, 1.000000000000000000 ) ) ;
#48540 = ADVANCED_FACE ( 'NONE', ( #46686 ), #45407, .T. ) ;
#48541 = DIRECTION ( 'NONE',  ( 0.000000000000000000, 0.000000000000000000, 1.000000000000000000 ) ) ;
#48542 = ORIENTED_EDGE ( 'NONE', *, *, #59637, .T. ) ;
#48543 = EDGE_CURVE ( 'NONE', #16181, #120910, #95144, .T. ) ;
#48544 = ADVANCED_FACE ( 'NONE', ( #96409 ), #105613, .T. ) ;
#48545 = PLANE ( 'NONE',  #122408 ) ;
#48546 = EDGE_CURVE ( 'NONE', #38970, #82397, #67597, .T. ) ;
#48547 = VERTEX_POINT ( 'NONE', #27048 ) ;
#48548 = CARTESIAN_POINT ( 'NONE',  ( 15.19999999999989271, 2.500000000000000000, -0.3464101615137783474 ) ) ;
#48549 = EDGE_CURVE ( 'NONE', #19084, #53181, #96566, .T. ) ;
#48550 = EDGE_LOOP ( 'NONE', ( #54235, #98065 ) ) ;
#48551 = CARTESIAN_POINT ( 'NONE',  ( 3.749999999999944045, 2.500000000000000000, -7.088010851410853519 ) ) ;
#48552 = EDGE_LOOP ( 'NONE', ( #85717, #128853 ) ) ;
#48553 = EDGE_LOOP ( 'NONE', ( #113735, #121629, #81596, #4111 ) ) ;
#48554 = EDGE_CURVE ( 'NONE', #37632, #103010, #117480, .T. ) ;
#48555 = CARTESIAN_POINT ( 'NONE',  ( -7.900000000000011013, 12.50000000000000000, 4.957854068765711553 ) ) ;
#48556 = DIRECTION ( 'NONE',  ( 0.000000000000000000, 1.000000000000000000, 0.000000000000000000 ) ) ;
#48557 = AXIS2_PLACEMENT_3D ( 'NONE', #112126, #70264, #59829 ) ;
#48558 = VECTOR ( 'NONE', #40029, 1000.000000000000000 ) ;
#48559 = CARTESIAN_POINT ( 'NONE',  ( 11.04999999999990656, 2.500000000000000000, -6.248780366869526759 ) ) ;
#48560 = AXIS2_PLACEMENT_3D ( 'NONE', #110373, #60651, #112318 ) ;
#48561 = FACE_OUTER_BOUND ( 'NONE', #59751, .T. ) ;
#48562 = LINE ( 'NONE', #127758, #128709 ) ;
#48563 = ORIENTED_EDGE ( 'NONE', *, *, #60748, .T. ) ;
#48564 = CARTESIAN_POINT ( 'NONE',  ( -4.600000000000024514, 2.500000000000000000, -0.7928203230275543412 ) ) ;
#48565 = CARTESIAN_POINT ( 'NONE',  ( 13.09999999999990195, 12.50000000000000000, 4.676537180435972552 ) ) ;
#48566 = FACE_OUTER_BOUND ( 'NONE', #71760, .T. ) ;
#48567 = DIRECTION ( 'NONE',  ( -0.000000000000000000, 1.000000000000000000, -0.000000000000000000 ) ) ;
#48568 = CONICAL_SURFACE ( 'NONE', #123750, 0.1000000000000002554, 0.003490658503988666988 ) ;
#48569 = AXIS2_PLACEMENT_3D ( 'NONE', #40750, #790, #81924 ) ;
#48570 = CARTESIAN_POINT ( 'NONE',  ( 1.649999999999950617, 2.500000000000000000, -2.065063509461102065 ) ) ;
#48571 = ORIENTED_EDGE ( 'NONE', *, *, #52107, .T. ) ;
#48572 = CONICAL_SURFACE ( 'NONE', #102938, 0.1000000000000002554, 0.003490658503988666988 ) ;
#48573 = VECTOR ( 'NONE', #104695, 1000.000000000000000 ) ;
#48574 = CONICAL_SURFACE ( 'NONE', #2566, 0.09999999999999982514, 0.003490658503988666988 ) ;
#48575 = VERTEX_POINT ( 'NONE', #66946 ) ;
#48576 = DIRECTION ( 'NONE',  ( 0.000000000000000000, 1.000000000000000000, 0.000000000000000000 ) ) ;
#48577 = CIRCLE ( 'NONE', #6674, 0.06509327318403745899 ) ;
#48578 = ORIENTED_EDGE ( 'NONE', *, *, #97204, .T. ) ;
#48579 = FACE_OUTER_BOUND ( 'NONE', #38579, .T. ) ;
#48580 = DIRECTION ( 'NONE',  ( -0.000000000000000000, 1.000000000000000000, -0.000000000000000000 ) ) ;
#48581 = CONICAL_SURFACE ( 'NONE', #92484, 0.1000000000000002554, 0.003490658503988666988 ) ;
#48582 = ORIENTED_EDGE ( 'NONE', *, *, #35980, .F. ) ;
#48583 = CARTESIAN_POINT ( 'NONE',  ( 184.5000000000000000, 0.000000000000000000, 7.700000000000000178 ) ) ;
#48584 = DIRECTION ( 'NONE',  ( 0.000000000000000000, 0.000000000000000000, -1.000000000000000000 ) ) ;
#48585 = LINE ( 'NONE', #16518, #77477 ) ;
#48586 = CARTESIAN_POINT ( 'NONE',  ( -1.450000000000035039, 2.500000000000000000, -6.841600689897077814 ) ) ;
#48587 = EDGE_LOOP ( 'NONE', ( #92582, #20587, #58909, #124379 ) ) ;
#48588 = EDGE_CURVE ( 'NONE', #10139, #41152, #35952, .T. ) ;
#48589 = DIRECTION ( 'NONE',  ( 0.000000000000000000, 1.000000000000000000, 0.000000000000000000 ) ) ;
#48590 = EDGE_CURVE ( 'NONE', #105322, #119917, #117317, .T. ) ;
#48591 = VERTEX_POINT ( 'NONE', #107540 ) ;
#48592 = CARTESIAN_POINT ( 'NONE',  ( 10.19999999999991047, 12.50000000000000000, 4.676537180435972552 ) ) ;
#48593 = CARTESIAN_POINT ( 'NONE',  ( 5.399999999999936406, 2.500000000000000000, -5.122947341949753763 ) ) ;
#48594 = CARTESIAN_POINT ( 'NONE',  ( 11.24999999999990763, 2.500000000000000000, -7.288010851410854585 ) ) ;
#48595 = EDGE_CURVE ( 'NONE', #22696, #98598, #57802, .T. ) ;
#48596 = ORIENTED_EDGE ( 'NONE', *, *, #45504, .F. ) ;
#48597 = CARTESIAN_POINT ( 'NONE',  ( -13.74999999999998757, 2.500000000000000000, 1.472243186433549456 ) ) ;
#48598 = AXIS2_PLACEMENT_3D ( 'NONE', #13050, #32095, #23533 ) ;
#48599 = VECTOR ( 'NONE', #77826, 1000.000000000000000 ) ;
#48600 = VERTEX_POINT ( 'NONE', #124607 ) ;
#48601 = CARTESIAN_POINT ( 'NONE',  ( 5.649999999999932854, 12.50000000000000000, 1.818653347947321475 ) ) ;
#48602 = LINE ( 'NONE', #128467, #42567 ) ;
#48603 = DIRECTION ( 'NONE',  ( 0.000000000000000000, 0.000000000000000000, 1.000000000000000000 ) ) ;
#48604 = VERTEX_POINT ( 'NONE', #50536 ) ;
#48606 = CARTESIAN_POINT ( 'NONE',  ( -9.800000000000006040, 2.500000000000000000, 4.776537180435972196 ) ) ;
#48605 = CIRCLE ( 'NONE', #15114, 0.09999999999999982514 ) ;
#48607 = AXIS2_PLACEMENT_3D ( 'NONE', #60799, #109237, #129570 ) ;
#48608 = LINE ( 'NONE', #9318, #32837 ) ;
#48609 = CIRCLE ( 'NONE', #104924, 0.1000000000000002554 ) ;
#48610 = VERTEX_POINT ( 'NONE', #109472 ) ;
#48611 = AXIS2_PLACEMENT_3D ( 'NONE', #66696, #94878, #5191 ) ;
#48612 = DIRECTION ( 'NONE',  ( 0.000000000000000000, 1.000000000000000000, 0.000000000000000000 ) ) ;
#48613 = ORIENTED_EDGE ( 'NONE', *, *, #20634, .F. ) ;
#48614 = CARTESIAN_POINT ( 'NONE',  ( -4.150000000000025224, 2.500000000000000000, 2.857883832488649301 ) ) ;
#48615 = EDGE_LOOP ( 'NONE', ( #83986, #11850, #77320, #9773 ) ) ;
#48616 = CYLINDRICAL_SURFACE ( 'NONE', #83962, 7.700000000000000178 ) ;
#48617 = CARTESIAN_POINT ( 'NONE',  ( -6.249999999999984901, 12.50000000000000000, -6.560283801567339701 ) ) ;
#48618 = VERTEX_POINT ( 'NONE', #70832 ) ;
#48619 = ORIENTED_EDGE ( 'NONE', *, *, #55037, .T. ) ;
#48620 = DIRECTION ( 'NONE',  ( 0.000000000000000000, 0.000000000000000000, 1.000000000000000000 ) ) ;
#48621 = CARTESIAN_POINT ( 'NONE',  ( 11.24999999999990941, 12.50000000000000000, -1.537336459617587581 ) ) ;
#48622 = ORIENTED_EDGE ( 'NONE', *, *, #60248, .F. ) ;
#48623 = CIRCLE ( 'NONE', #44505, 0.1000000000000002554 ) ;
#48625 = EDGE_CURVE ( 'NONE', #52844, #54614, #100770, .T. ) ;
#48624 = CARTESIAN_POINT ( 'NONE',  ( 10.64999999999991331, 2.500000000000000000, -2.611473670974877592 ) ) ;
#48626 = CARTESIAN_POINT ( 'NONE',  ( -13.94999999999998685, 2.500000000000000000, -2.511473670974875727 ) ) ;
#48627 = FACE_OUTER_BOUND ( 'NONE', #94046, .T. ) ;
#48628 = CARTESIAN_POINT ( 'NONE',  ( 103.2649310519763617, 8.549820648965553715, -1.639149876075294276 ) ) ;
#48629 = DIRECTION ( 'NONE',  ( 0.000000000000000000, 0.000000000000000000, 1.000000000000000000 ) ) ;
#48630 = DIRECTION ( 'NONE',  ( 0.000000000000000000, 1.000000000000000000, 0.000000000000000000 ) ) ;
#48631 = CARTESIAN_POINT ( 'NONE',  ( -10.80000000000000071, 12.50000000000000000, 4.395220292106234439 ) ) ;
#48632 = EDGE_LOOP ( 'NONE', ( #20610, #19168, #85086, #94173 ) ) ;
#48633 = VERTEX_POINT ( 'NONE', #38831 ) ;
#48634 = EDGE_LOOP ( 'NONE', ( #59900, #106493 ) ) ;
#48635 = ORIENTED_EDGE ( 'NONE', *, *, #126225, .F. ) ;
#48636 = CARTESIAN_POINT ( 'NONE',  ( -3.350000000000029399, 12.50000000000000000, 6.560283801567334372 ) ) ;
#48637 = DIRECTION ( 'NONE',  ( 0.000000000000000000, 0.000000000000000000, 1.000000000000000000 ) ) ;
#48638 = EDGE_CURVE ( 'NONE', #102323, #127947, #44353, .T. ) ;
#48639 = CARTESIAN_POINT ( 'NONE',  ( -0.8500000000000395017, 2.500000000000000000, 6.395190528383296602 ) ) ;
#48640 = EDGE_LOOP ( 'NONE', ( #90133, #47713, #67779, #37295 ) ) ;
#48641 = FACE_BOUND ( 'NONE', #126463, .T. ) ;
#48642 = ORIENTED_EDGE ( 'NONE', *, *, #52372, .F. ) ;
#48643 = EDGE_CURVE ( 'NONE', #53612, #17715, #73592, .T. ) ;
#48644 = CIRCLE ( 'NONE', #75725, 0.09999999999999982514 ) ;
#48645 = LINE ( 'NONE', #19154, #50063 ) ;
#48646 = DIRECTION ( 'NONE',  ( -1.000000000000000000, -0.000000000000000000, -0.000000000000000000 ) ) ;
#48647 = STYLED_ITEM ( 'NONE', ( #3452 ), #57499 ) ;
#48649 = LINE ( 'NONE', #18533, #105687 ) ;
#48648 = AXIS2_PLACEMENT_3D ( 'NONE', #99037, #61039, #68924 ) ;
#48650 = AXIS2_PLACEMENT_3D ( 'NONE', #909, #128605, #29724 ) ;
#48651 = DIRECTION ( 'NONE',  ( 0.000000000000000000, 0.000000000000000000, -1.000000000000000000 ) ) ;
#48652 = DIRECTION ( 'NONE',  ( 0.000000000000000000, 0.000000000000000000, 1.000000000000000000 ) ) ;
#48653 = CARTESIAN_POINT ( 'NONE',  ( -5.450000000000023270, 12.50000000000000000, -6.495190528383302464 ) ) ;
#48654 = DIRECTION ( 'NONE',  ( 0.000000000000000000, 1.000000000000000000, 0.000000000000000000 ) ) ;
#48655 = DIRECTION ( 'NONE',  ( 0.000000000000000000, 0.000000000000000000, 1.000000000000000000 ) ) ;
#48656 = EDGE_CURVE ( 'NONE', #15598, #80232, #71544, .T. ) ;
#48657 = CARTESIAN_POINT ( 'NONE',  ( 2.049999999999950084, 2.500000000000000000, -6.595190528383302109 ) ) ;
#48658 = CIRCLE ( 'NONE', #121801, 0.06509327318403745899 ) ;
#48659 = DIRECTION ( 'NONE',  ( 0.000000000000000000, 0.000000000000000000, 1.000000000000000000 ) ) ;
#48660 = VERTEX_POINT ( 'NONE', #11260 ) ;
#48661 = EDGE_LOOP ( 'NONE', ( #97904, #33186 ) ) ;
#48662 = ORIENTED_EDGE ( 'NONE', *, *, #124499, .F. ) ;
#48664 = ORIENTED_EDGE ( 'NONE', *, *, #126116, .T. ) ;
#48663 = AXIS2_PLACEMENT_3D ( 'NONE', #79534, #20615, #49445 ) ;
#48665 = AXIS2_PLACEMENT_3D ( 'NONE', #37276, #47097, #117731 ) ;
#48666 = AXIS2_PLACEMENT_3D ( 'NONE', #55585, #44469, #45130 ) ;
#48667 = CARTESIAN_POINT ( 'NONE',  ( -12.89999999999999325, 2.500000000000000000, 0.6928203230275535862 ) ) ;
#48668 = DIRECTION ( 'NONE',  ( 0.000000000000000000, 0.000000000000000000, -1.000000000000000000 ) ) ;
#48670 = EDGE_LOOP ( 'NONE', ( #103540, #58676, #44907, #24934 ) ) ;
#48669 = EDGE_LOOP ( 'NONE', ( #105830, #116758, #95158, #77483 ) ) ;
#48671 = VERTEX_POINT ( 'NONE', #18508 ) ;
#48672 = AXIS2_PLACEMENT_3D ( 'NONE', #58133, #38505, #99346 ) ;
#48673 = DIRECTION ( 'NONE',  ( 0.000000000000000000, 1.000000000000000000, 0.000000000000000000 ) ) ;
#48674 = CARTESIAN_POINT ( 'NONE',  ( -8.749999999999971578, 2.500000000000000000, 6.495190528383297135 ) ) ;
#48675 = CARTESIAN_POINT ( 'NONE',  ( -9.150000000000009237, 2.500000000000000000, 2.065063509461097624 ) ) ;
#48676 = DIRECTION ( 'NONE',  ( 0.000000000000000000, 0.000000000000000000, 1.000000000000000000 ) ) ;
#48677 = DIRECTION ( 'NONE',  ( 0.000000000000000000, 0.000000000000000000, -1.000000000000000000 ) ) ;
#48678 = LINE ( 'NONE', #10039, #18424 ) ;
#48679 = CARTESIAN_POINT ( 'NONE',  ( 7.699999999999925571, 2.500000000000000000, 3.883716857408420431 ) ) ;
#48680 = ORIENTED_EDGE ( 'NONE', *, *, #85936, .F. ) ;
#48681 = CARTESIAN_POINT ( 'NONE',  ( 1.649999999999950617, 2.500000000000000000, 2.165063509461097713 ) ) ;
#48682 = EDGE_LOOP ( 'NONE', ( #73029, #57849 ) ) ;
#48683 = ADVANCED_FACE ( 'NONE', ( #58453 ), #15074, .T. ) ;
#48684 = ORIENTED_EDGE ( 'NONE', *, *, #118875, .T. ) ;
#48685 = EDGE_LOOP ( 'NONE', ( #20593, #36652 ) ) ;
#48686 = DIRECTION ( 'NONE',  ( 0.000000000000000000, 0.000000000000000000, 1.000000000000000000 ) ) ;
#48687 = AXIS2_PLACEMENT_3D ( 'NONE', #68801, #697, #69436 ) ;
#48688 = CONICAL_SURFACE ( 'NONE', #19415, 0.1000000000000000472, 0.003490658503988666988 ) ;
#48689 = EDGE_LOOP ( 'NONE', ( #81262, #98408 ) ) ;
#48690 = EDGE_CURVE ( 'NONE', #119719, #21947, #61089, .T. ) ;
#48691 = ORIENTED_EDGE ( 'NONE', *, *, #14090, .F. ) ;
#48692 = EDGE_CURVE ( 'NONE', #19521, #104314, #84060, .T. ) ;
#48693 = DIRECTION ( 'NONE',  ( -0.000000000000000000, -1.000000000000000000, -0.000000000000000000 ) ) ;
#48694 = CARTESIAN_POINT ( 'NONE',  ( 2.099999999999950351, 12.50000000000000000, -0.06509327318403970719 ) ) ;
#48695 = DIRECTION ( 'NONE',  ( -0.000000000000000000, 1.000000000000000000, -0.000000000000000000 ) ) ;
#48697 = CARTESIAN_POINT ( 'NONE',  ( 14.79999999999989235, 12.50000000000000000, 0.2813168883297361700 ) ) ;
#48696 = CONICAL_SURFACE ( 'NONE', #75862, 0.1000000000000000056, 0.003490658503988666988 ) ;
#48698 = ADVANCED_FACE ( 'NONE', ( #140 ), #69535, .T. ) ;
#48699 = AXIS2_PLACEMENT_3D ( 'NONE', #103115, #13432, #53382 ) ;
#48700 = ADVANCED_FACE ( 'NONE', ( #98345 ), #46402, .T. ) ;
#48701 = CARTESIAN_POINT ( 'NONE',  ( -7.500000000000013323, 12.50000000000000000, 4.957854068765711553 ) ) ;
#48702 = ADVANCED_FACE ( 'NONE', ( #89187 ), #14988, .T. ) ;
#48703 = ORIENTED_EDGE ( 'NONE', *, *, #117512, .T. ) ;
#48704 = DIRECTION ( 'NONE',  ( -0.000000000000000000, -1.000000000000000000, -0.000000000000000000 ) ) ;
#48705 = AXIS2_PLACEMENT_3D ( 'NONE', #117272, #77385, #99611 ) ;
#48707 = EDGE_LOOP ( 'NONE', ( #90925, #71052, #3369, #45090 ) ) ;
#48706 = AXIS2_PLACEMENT_3D ( 'NONE', #29894, #118264, #30561 ) ;
#48708 = CARTESIAN_POINT ( 'NONE',  ( 5.399999999999931966, 2.500000000000000000, 4.430127018922196847 ) ) ;
#48709 = CIRCLE ( 'NONE', #11023, 0.09999999999999982514 ) ;
#48710 = EDGE_CURVE ( 'NONE', #18522, #75910, #86098, .T. ) ;
#48711 = VERTEX_POINT ( 'NONE', #40092 ) ;
#48712 = LINE ( 'NONE', #129223, #66365 ) ;
#48713 = DIRECTION ( 'NONE',  ( 0.000000000000000000, 1.000000000000000000, 0.000000000000000000 ) ) ;
#48714 = AXIS2_PLACEMENT_3D ( 'NONE', #21125, #21795, #72182 ) ;
#48715 = ORIENTED_EDGE ( 'NONE', *, *, #13664, .T. ) ;
#48716 = CIRCLE ( 'NONE', #34036, 0.09999999999999982514 ) ;
#48717 = DIRECTION ( 'NONE',  ( 0.000000000000000000, -0.9999939076577903929, 0.003490651415223739937 ) ) ;
#48718 = CARTESIAN_POINT ( 'NONE',  ( -11.84999999999999787, 12.50000000000000000, -6.776507416713037024 ) ) ;
#48719 = ORIENTED_EDGE ( 'NONE', *, *, #98313, .F. ) ;
#48720 = EDGE_CURVE ( 'NONE', #82761, #69440, #29615, .T. ) ;
#48721 = CIRCLE ( 'NONE', #82052, 0.09999999999999982514 ) ;
#48722 = DIRECTION ( 'NONE',  ( -0.000000000000000000, 1.000000000000000000, -0.000000000000000000 ) ) ;
#48723 = ORIENTED_EDGE ( 'NONE', *, *, #82875, .T. ) ;
#48724 = VERTEX_POINT ( 'NONE', #128492 ) ;
#48725 = FACE_OUTER_BOUND ( 'NONE', #50986, .T. ) ;
#48726 = DIRECTION ( 'NONE',  ( 0.000000000000000000, 1.000000000000000000, 0.000000000000000000 ) ) ;
#48727 = CARTESIAN_POINT ( 'NONE',  ( 184.7135416670080872, 4.367472073101518859, -7.564683531249999149 ) ) ;
#48728 = CARTESIAN_POINT ( 'NONE',  ( -4.150000000000025224, 2.500000000000000000, 5.702370205355745014 ) ) ;
#48729 = CIRCLE ( 'NONE', #121866, 0.06509327318403741736 ) ;
#48730 = DIRECTION ( 'NONE',  ( 0.000000000000000000, 0.000000000000000000, 1.000000000000000000 ) ) ;
#48731 = ORIENTED_EDGE ( 'NONE', *, *, #6056, .F. ) ;
#48732 = CARTESIAN_POINT ( 'NONE',  ( 9.149999999999918643, 12.50000000000000000, -6.495190528383302464 ) ) ;
#48733 = VECTOR ( 'NONE', #59560, 1000.000000000000000 ) ;
#48734 = ORIENTED_EDGE ( 'NONE', *, *, #94708, .T. ) ;
#48735 = VECTOR ( 'NONE', #96415, 1000.000000000000000 ) ;
#48736 = DIRECTION ( 'NONE',  ( 0.000000000000000000, 0.000000000000000000, -1.000000000000000000 ) ) ;
#48737 = DIRECTION ( 'NONE',  ( 0.000000000000000000, 0.000000000000000000, 1.000000000000000000 ) ) ;
#48738 = AXIS2_PLACEMENT_3D ( 'NONE', #64878, #4652, #43978 ) ;
#48739 = ORIENTED_EDGE ( 'NONE', *, *, #89273, .F. ) ;
#48740 = DIRECTION ( 'NONE',  ( 0.000000000000000000, 1.000000000000000000, 0.000000000000000000 ) ) ;
#48741 = DIRECTION ( 'NONE',  ( 0.000000000000000000, 0.000000000000000000, 1.000000000000000000 ) ) ;
#48742 = DIRECTION ( 'NONE',  ( 0.000000000000000000, 1.000000000000000000, 0.000000000000000000 ) ) ;
#48743 = CARTESIAN_POINT ( 'NONE',  ( -11.84999999999999609, 2.500000000000000000, 6.248780366869521430 ) ) ;
#48744 = CIRCLE ( 'NONE', #54983, 0.1000000000000002554 ) ;
#48746 = CIRCLE ( 'NONE', #113581, 0.1000000000000000472 ) ;
#48745 = CARTESIAN_POINT ( 'NONE',  ( -0.6500000000000403233, 2.500000000000000000, 6.048780366869520364 ) ) ;
#48747 = ORIENTED_EDGE ( 'NONE', *, *, #93619, .F. ) ;
#48748 = CIRCLE ( 'NONE', #44525, 0.06509327318403745899 ) ;
#48749 = VECTOR ( 'NONE', #40709, 1000.000000000000000 ) ;
#48750 = EDGE_CURVE ( 'NONE', #65189, #74144, #79858, .T. ) ;
#48751 = CARTESIAN_POINT ( 'NONE',  ( -10.40000000000000213, 2.500000000000000000, -5.022947341949749678 ) ) ;
#48752 = CARTESIAN_POINT ( 'NONE',  ( 5.649999999999932854, 12.50000000000000000, 2.511473670974873507 ) ) ;
#48753 = AXIS2_PLACEMENT_3D ( 'NONE', #108484, #128807, #8988 ) ;
#48754 = VERTEX_POINT ( 'NONE', #110117 ) ;
#48755 = DIRECTION ( 'NONE',  ( -0.000000000000000000, -1.000000000000000000, -0.000000000000000000 ) ) ;
#48756 = EDGE_CURVE ( 'NONE', #29100, #18148, #4611, .T. ) ;
#48757 = VERTEX_POINT ( 'NONE', #40757 ) ;
#48758 = CONICAL_SURFACE ( 'NONE', #90499, 0.1000000000000002554, 0.003490658503988666988 ) ;
#48760 = ORIENTED_EDGE ( 'NONE', *, *, #29847, .T. ) ;
#48759 = CIRCLE ( 'NONE', #44643, 0.06509327318403745899 ) ;
#48761 = CARTESIAN_POINT ( 'NONE',  ( 127.5000000000000000, -1.500000000000000000, -6.000000000000000000 ) ) ;
#48763 = ORIENTED_EDGE ( 'NONE', *, *, #84758, .F. ) ;
#48762 = CIRCLE ( 'NONE', #15273, 0.1000000000000002554 ) ;
#48764 = CARTESIAN_POINT ( 'NONE',  ( 9.599999999999914380, 12.50000000000000000, -3.637306695894650055 ) ) ;
#48765 = DIRECTION ( 'NONE',  ( -4.274815082592931898E-19, -0.9999939076577903929, -0.003490651415223739937 ) ) ;
#48766 = ORIENTED_EDGE ( 'NONE', *, *, #14820, .T. ) ;
#48767 = CARTESIAN_POINT ( 'NONE',  ( 12.29999999999990123, 2.500000000000000000, 0.2464101615137735679 ) ) ;
#48768 = AXIS2_PLACEMENT_3D ( 'NONE', #27879, #26596, #37706 ) ;
#48770 = VERTEX_POINT ( 'NONE', #48621 ) ;
#48769 = DIRECTION ( 'NONE',  ( 0.000000000000000000, -0.9999939076577903929, 0.003490651415223739937 ) ) ;
#48771 = PLANE ( 'NONE',  #31920 ) ;
#48772 = CARTESIAN_POINT ( 'NONE',  ( 129.5000000000000000, -1.000000000000025535, -7.634788798650553154 ) ) ;
#48773 = ORIENTED_EDGE ( 'NONE', *, *, #108514, .T. ) ;
#48774 = VERTEX_POINT ( 'NONE', #28990 ) ;
#48775 = EDGE_LOOP ( 'NONE', ( #109067, #78494, #45399, #32347 ) ) ;
#48776 = CARTESIAN_POINT ( 'NONE',  ( -14.14999999999998792, 12.50000000000000000, -1.537336459617585360 ) ) ;
#48777 = DIRECTION ( 'NONE',  ( -4.274815082592931898E-19, -0.9999939076577903929, -0.003490651415223739937 ) ) ;
#48779 = FACE_OUTER_BOUND ( 'NONE', #34296, .T. ) ;
#48778 = CIRCLE ( 'NONE', #30001, 0.06509327318403745899 ) ;
#48780 = FACE_BOUND ( 'NONE', #12783, .T. ) ;
#48781 = ORIENTED_EDGE ( 'NONE', *, *, #68361, .F. ) ;
#48782 = LINE ( 'NONE', #67087, #82496 ) ;
#48783 = DIRECTION ( 'NONE',  ( -0.000000000000000000, -1.000000000000000000, -0.000000000000000000 ) ) ;
#48784 = VERTEX_POINT ( 'NONE', #80666 ) ;
#48786 = ADVANCED_FACE ( 'NONE', ( #68895 ), #33897, .T. ) ;
#48785 = CARTESIAN_POINT ( 'NONE',  ( -3.350000000000029399, 2.500000000000000000, 6.595190528383296780 ) ) ;
#48788 = LINE ( 'NONE', #38994, #122376 ) ;
#48787 = CIRCLE ( 'NONE', #121940, 2.000000000000000000 ) ;
#48789 = CONICAL_SURFACE ( 'NONE', #44575, 0.09999999999999982514, 0.003490658503988666988 ) ;
#48791 = CIRCLE ( 'NONE', #119884, 0.1000000000000002554 ) ;
#48790 = DIRECTION ( 'NONE',  ( 0.000000000000000000, 0.000000000000000000, 1.000000000000000000 ) ) ;
#48792 = FACE_OUTER_BOUND ( 'NONE', #39761, .T. ) ;
#48793 = DIRECTION ( 'NONE',  ( 0.000000000000000000, 0.000000000000000000, 1.000000000000000000 ) ) ;
#48794 = DIRECTION ( 'NONE',  ( -0.000000000000000000, -1.000000000000000000, -0.000000000000000000 ) ) ;
#48795 = PLANE ( 'NONE',  #12773 ) ;
#48796 = ADVANCED_FACE ( 'NONE', ( #33506 ), #77791, .T. ) ;
#48797 = AXIS2_PLACEMENT_3D ( 'NONE', #94942, #93650, #24260 ) ;
#48798 = AXIS2_PLACEMENT_3D ( 'NONE', #73553, #72925, #102394 ) ;
#48799 = VERTEX_POINT ( 'NONE', #92398 ) ;
#48800 = ORIENTED_EDGE ( 'NONE', *, *, #54720, .T. ) ;
#48801 = ORIENTED_EDGE ( 'NONE', *, *, #65340, .F. ) ;
#48802 = ORIENTED_EDGE ( 'NONE', *, *, #64024, .T. ) ;
#48804 = VERTEX_POINT ( 'NONE', #2726 ) ;
#48803 = CONICAL_SURFACE ( 'NONE', #59181, 0.09999999999999982514, 0.003490658503988666988 ) ;
#48805 = DIRECTION ( 'NONE',  ( 0.000000000000000000, 1.000000000000000000, 0.000000000000000000 ) ) ;
#48806 = CIRCLE ( 'NONE', #52998, 0.06509327318403743123 ) ;
#48807 = ADVANCED_FACE ( 'NONE', ( #43962 ), #101588, .F. ) ;
#48808 = CARTESIAN_POINT ( 'NONE',  ( -6.050000000000017586, 12.50000000000000000, 1.818653347947321475 ) ) ;
#48809 = VERTEX_POINT ( 'NONE', #113987 ) ;
#48810 = FACE_BOUND ( 'NONE', #71192, .T. ) ;
#48811 = EDGE_CURVE ( 'NONE', #22835, #54447, #120843, .T. ) ;
#48812 = CONICAL_SURFACE ( 'NONE', #65508, 0.09999999999999999167, 0.003490658503988666988 ) ;
#48813 = DIRECTION ( 'NONE',  ( -0.000000000000000000, 1.000000000000000000, -0.000000000000000000 ) ) ;
#48814 = ADVANCED_FACE ( 'NONE', ( #91760 ), #102236, .T. ) ;
#48815 = CARTESIAN_POINT ( 'NONE',  ( -5.600000000000020073, 2.500000000000000000, 4.676537180435972552 ) ) ;
#48816 = CARTESIAN_POINT ( 'NONE',  ( -8.550000000000013145, 12.50000000000000000, 2.511473670974873507 ) ) ;
#48817 = FACE_OUTER_BOUND ( 'NONE', #58595, .T. ) ;
#48818 = EDGE_CURVE ( 'NONE', #2356, #55110, #22399, .T. ) ;
#48819 = DIRECTION ( 'NONE',  ( -0.000000000000000000, 1.000000000000000000, -0.000000000000000000 ) ) ;
#48820 = ORIENTED_EDGE ( 'NONE', *, *, #79864, .F. ) ;
#48821 = CIRCLE ( 'NONE', #103090, 0.06509327318403745899 ) ;
#48822 = EDGE_LOOP ( 'NONE', ( #85954, #112178 ) ) ;
#48823 = ORIENTED_EDGE ( 'NONE', *, *, #70989, .T. ) ;
#48824 = ORIENTED_EDGE ( 'NONE', *, *, #79617, .T. ) ;
#48825 = DIRECTION ( 'NONE',  ( -0.000000000000000000, 1.000000000000000000, -0.000000000000000000 ) ) ;
#48826 = DIRECTION ( 'NONE',  ( 0.000000000000000000, 0.000000000000000000, 1.000000000000000000 ) ) ;
#48827 = FACE_OUTER_BOUND ( 'NONE', #114557, .T. ) ;
#48828 = ORIENTED_EDGE ( 'NONE', *, *, #118762, .T. ) ;
#48829 = DIRECTION ( 'NONE',  ( 0.000000000000000000, -0.9999939076577903929, 0.003490651415223739937 ) ) ;
#48830 = AXIS2_PLACEMENT_3D ( 'NONE', #111856, #102031, #91562 ) ;
#48831 = AXIS2_PLACEMENT_3D ( 'NONE', #68902, #28349, #78089 ) ;
#48833 = DIRECTION ( 'NONE',  ( 0.000000000000000000, 0.000000000000000000, -1.000000000000000000 ) ) ;
#48832 = AXIS2_PLACEMENT_3D ( 'NONE', #44236, #35720, #75002 ) ;
#48834 = FACE_OUTER_BOUND ( 'NONE', #17881, .T. ) ;
#48835 = CARTESIAN_POINT ( 'NONE',  ( 184.6093750003413732, 9.264065473108010111E-16, -7.564683531250000925 ) ) ;
#48836 = DIRECTION ( 'NONE',  ( -0.000000000000000000, 1.000000000000000000, -0.000000000000000000 ) ) ;
#48837 = DIRECTION ( 'NONE',  ( 0.000000000000000000, -0.000000000000000000, 1.000000000000000000 ) ) ;
#48838 = DIRECTION ( 'NONE',  ( 7.228014483236698281E-17, -0.000000000000000000, 1.000000000000000000 ) ) ;
#48839 = AXIS2_PLACEMENT_3D ( 'NONE', #102687, #62788, #73241 ) ;
#48840 = EDGE_LOOP ( 'NONE', ( #61032, #82386 ) ) ;
#48841 = PLANE ( 'NONE',  #23273 ) ;
#48842 = AXIS2_PLACEMENT_3D ( 'NONE', #19345, #117530, #27238 ) ;
#48843 = VERTEX_POINT ( 'NONE', #41393 ) ;
#48844 = CIRCLE ( 'NONE', #111520, 0.06509327318403745899 ) ;
#48845 = ADVANCED_FACE ( 'NONE', ( #112700 ), #118784, .T. ) ;
#48846 = ORIENTED_EDGE ( 'NONE', *, *, #109065, .T. ) ;
#48847 = CARTESIAN_POINT ( 'NONE',  ( 8.349999999999919709, 2.500000000000000000, -2.265063509461101798 ) ) ;
#48848 = DIRECTION ( 'NONE',  ( -4.274815082592931898E-19, -0.9999939076577903929, -0.003490651415223739937 ) ) ;
#48849 = CARTESIAN_POINT ( 'NONE',  ( -5.650000000000019895, 12.50000000000000000, 6.213873640053558134 ) ) ;
#48850 = CIRCLE ( 'NONE', #117764, 0.06509327318403745899 ) ;
#48851 = EDGE_LOOP ( 'NONE', ( #87304, #83927 ) ) ;
#48853 = EDGE_CURVE ( 'NONE', #110877, #127992, #45646, .T. ) ;
#48852 = ORIENTED_EDGE ( 'NONE', *, *, #56596, .F. ) ;
#48854 = DIRECTION ( 'NONE',  ( -0.000000000000000000, 1.000000000000000000, -0.000000000000000000 ) ) ;
#48856 = AXIS2_PLACEMENT_3D ( 'NONE', #122651, #11404, #82747 ) ;
#48855 = LINE ( 'NONE', #80241, #34919 ) ;
#48857 = AXIS2_PLACEMENT_3D ( 'NONE', #78599, #118490, #20303 ) ;
#48858 = AXIS2_PLACEMENT_3D ( 'NONE', #49501, #8891, #106459 ) ;
#48859 = ORIENTED_EDGE ( 'NONE', *, *, #1396, .F. ) ;
#48860 = ORIENTED_EDGE ( 'NONE', *, *, #35840, .F. ) ;
#48861 = EDGE_CURVE ( 'NONE', #22448, #33469, #112544, .T. ) ;
#48862 = DIRECTION ( 'NONE',  ( -0.000000000000000000, 1.000000000000000000, -0.000000000000000000 ) ) ;
#48863 = ADVANCED_FACE ( 'NONE', ( #103523 ), #83865, .T. ) ;
#48864 = EDGE_CURVE ( 'NONE', #73617, #58840, #100013, .T. ) ;
#48865 = ORIENTED_EDGE ( 'NONE', *, *, #59941, .T. ) ;
#48866 = AXIS2_PLACEMENT_3D ( 'NONE', #35585, #75484, #124606 ) ;
#48867 = CARTESIAN_POINT ( 'NONE',  ( -6.850000000000013856, 2.500000000000000000, 1.818653347947321475 ) ) ;
#48868 = VERTEX_POINT ( 'NONE', #74057 ) ;
#48869 = DIRECTION ( 'NONE',  ( 0.000000000000000000, 0.000000000000000000, 1.000000000000000000 ) ) ;
#48870 = EDGE_CURVE ( 'NONE', #55120, #32820, #12544, .T. ) ;
#48871 = CARTESIAN_POINT ( 'NONE',  ( 6.849999999999927702, 2.500000000000000000, 2.611473670974873151 ) ) ;
#48872 = DIRECTION ( 'NONE',  ( 0.000000000000000000, 0.000000000000000000, 1.000000000000000000 ) ) ;
#48873 = CARTESIAN_POINT ( 'NONE',  ( -6.250000000000015987, 12.50000000000000000, 1.537336459617582918 ) ) ;
#48874 = ORIENTED_EDGE ( 'NONE', *, *, #15968, .T. ) ;
#48875 = EDGE_CURVE ( 'NONE', #91777, #32532, #53769, .T. ) ;
#48876 = DIRECTION ( 'NONE',  ( -4.274815082592931898E-19, -0.9999939076577903929, -0.003490651415223739937 ) ) ;
#48877 = ADVANCED_FACE ( 'NONE', ( #82601 ), #32223, .T. ) ;
#48878 = VERTEX_POINT ( 'NONE', #93697 ) ;
#48879 = EDGE_LOOP ( 'NONE', ( #53080, #5807, #20091, #106966 ) ) ;
#48880 = VECTOR ( 'NONE', #47575, 1000.000000000000000 ) ;
#48881 = AXIS2_PLACEMENT_3D ( 'NONE', #61534, #102713, #32080 ) ;
#48882 = CARTESIAN_POINT ( 'NONE',  ( -4.150000000000025224, 2.500000000000000000, 6.595190528383296780 ) ) ;
#48883 = DIRECTION ( 'NONE',  ( -4.274815082592931898E-19, -0.9999939076577903929, -0.003490651415223739937 ) ) ;
#48884 = CARTESIAN_POINT ( 'NONE',  ( 7.899999999999921307, 2.500000000000000000, -2.385244779468109755E-15 ) ) ;
#48885 = CARTESIAN_POINT ( 'NONE',  ( 2.499999999999945377, 2.500000000000000000, 5.022947341949748790 ) ) ;
#48886 = CARTESIAN_POINT ( 'NONE',  ( 7.099999999999926814, 12.50000000000000000, -0.7579135962115916003 ) ) ;
#48887 = DIRECTION ( 'NONE',  ( 0.000000000000000000, 1.000000000000000000, 0.000000000000000000 ) ) ;
#48888 = CONICAL_SURFACE ( 'NONE', #128302, 0.1000000000000002554, 0.003490658503988666988 ) ;
#48889 = AXIS2_PLACEMENT_3D ( 'NONE', #83649, #60932, #103291 ) ;
#48890 = PLANE ( 'NONE',  #67730 ) ;
#48891 = AXIS2_PLACEMENT_3D ( 'NONE', #36576, #77127, #7720 ) ;
#48892 = FACE_OUTER_BOUND ( 'NONE', #63112, .T. ) ;
#48894 = AXIS2_PLACEMENT_3D ( 'NONE', #104521, #54771, #115622 ) ;
#48893 = CARTESIAN_POINT ( 'NONE',  ( -7.900000000000014566, 2.500000000000000000, -2.276824562219559311E-15 ) ) ;
#48895 = CONICAL_SURFACE ( 'NONE', #73702, 0.1000000000000002554, 0.003490658503988666988 ) ;
#48896 = CONICAL_SURFACE ( 'NONE', #55144, 0.1000000000000002554, 0.003490658503988666988 ) ;
#48897 = AXIS2_PLACEMENT_3D ( 'NONE', #122571, #91170, #32921 ) ;
#48898 = EDGE_LOOP ( 'NONE', ( #47111, #19356, #79780, #42819 ) ) ;
#48899 = CARTESIAN_POINT ( 'NONE',  ( 9.799999999999918998, 2.500000000000000000, -0.3464101615137782364 ) ) ;
#48900 = CONICAL_SURFACE ( 'NONE', #113634, 0.09999999999999999167, 0.003490658503988666988 ) ;
#48901 = DIRECTION ( 'NONE',  ( -0.000000000000000000, 1.000000000000000000, -0.000000000000000000 ) ) ;
#48902 = CARTESIAN_POINT ( 'NONE',  ( -5.400000000000019895, 12.50000000000000000, -0.6277270498435166823 ) ) ;
#48903 = DIRECTION ( 'NONE',  ( 0.000000000000000000, 0.000000000000000000, 1.000000000000000000 ) ) ;
#48904 = CARTESIAN_POINT ( 'NONE',  ( -0.6500000000000398792, 2.500000000000000000, -6.841600689897078702 ) ) ;
#48905 = VERTEX_POINT ( 'NONE', #81929 ) ;
#48906 = FACE_OUTER_BOUND ( 'NONE', #111680, .T. ) ;
#48907 = CARTESIAN_POINT ( 'NONE',  ( 4.399999999999940847, 2.500000000000000000, -3.883716857408426648 ) ) ;
#48909 = ORIENTED_EDGE ( 'NONE', *, *, #1955, .T. ) ;
#48908 = DIRECTION ( 'NONE',  ( -0.000000000000000000, 1.000000000000000000, -0.000000000000000000 ) ) ;
#48910 = AXIS2_PLACEMENT_3D ( 'NONE', #20426, #60374, #100277 ) ;
#48911 = ORIENTED_EDGE ( 'NONE', *, *, #114820, .T. ) ;
#48912 = CARTESIAN_POINT ( 'NONE',  ( 2.299999999999948752, 2.500000000000000000, -3.983716857408426293 ) ) ;
#48913 = EDGE_CURVE ( 'NONE', #59940, #69598, #104161, .T. ) ;
#48914 = VERTEX_POINT ( 'NONE', #62318 ) ;
#48915 = EDGE_LOOP ( 'NONE', ( #127908, #1045 ) ) ;
#48916 = ORIENTED_EDGE ( 'NONE', *, *, #26500, .T. ) ;
#48917 = FACE_OUTER_BOUND ( 'NONE', #99375, .T. ) ;
#48918 = DIRECTION ( 'NONE',  ( 0.000000000000000000, 0.000000000000000000, 1.000000000000000000 ) ) ;
#48919 = CARTESIAN_POINT ( 'NONE',  ( 0.7999999999999612976, 12.50000000000000000, -1.084202172485504434E-16 ) ) ;
#48920 = CIRCLE ( 'NONE', #113762, 0.06509327318403745899 ) ;
#48921 = LINE ( 'NONE', #108460, #29117 ) ;
#48922 = AXIS2_PLACEMENT_3D ( 'NONE', #94974, #125693, #15082 ) ;
#48923 = EDGE_LOOP ( 'NONE', ( #4637, #53296, #15405, #113166 ) ) ;
#48924 = DIRECTION ( 'NONE',  ( 0.000000000000000000, 1.000000000000000000, 0.000000000000000000 ) ) ;
#48925 = ORIENTED_EDGE ( 'NONE', *, *, #95877, .T. ) ;
#48926 = DIRECTION ( 'NONE',  ( 0.000000000000000000, 0.000000000000000000, -1.000000000000000000 ) ) ;
#48927 = CARTESIAN_POINT ( 'NONE',  ( 15.24415751722251144, -2.474878586409045678, -4.460068884085897523 ) ) ;
#48928 = CARTESIAN_POINT ( 'NONE',  ( 15.44463772192102269, 2.469073678227445168, 4.264595835262002588 ) ) ;
#48929 = CARTESIAN_POINT ( 'NONE',  ( 10.84999999999991260, 2.500000000000000000, -2.165063509461101710 ) ) ;
#48930 = DIRECTION ( 'NONE',  ( -0.000000000000000000, -1.000000000000000000, -0.000000000000000000 ) ) ;
#48931 = EDGE_LOOP ( 'NONE', ( #108214, #35921 ) ) ;
#48932 = EDGE_LOOP ( 'NONE', ( #106326, #66606, #96085, #74787 ) ) ;
#48933 = ORIENTED_EDGE ( 'NONE', *, *, #102290, .F. ) ;
#48934 = ORIENTED_EDGE ( 'NONE', *, *, #34044, .F. ) ;
#48935 = ORIENTED_EDGE ( 'NONE', *, *, #103221, .F. ) ;
#48936 = DIRECTION ( 'NONE',  ( -0.000000000000000000, -1.000000000000000000, -0.000000000000000000 ) ) ;
#48937 = CARTESIAN_POINT ( 'NONE',  ( 10.19999999999991225, 2.500000000000000000, -4.676537180435978769 ) ) ;
#48938 = DIRECTION ( 'NONE',  ( 0.000000000000000000, 1.000000000000000000, 0.000000000000000000 ) ) ;
#48939 = FACE_BOUND ( 'NONE', #9573, .T. ) ;
#48940 = DIRECTION ( 'NONE',  ( 0.000000000000000000, 0.000000000000000000, 1.000000000000000000 ) ) ;
#48941 = CARTESIAN_POINT ( 'NONE',  ( 186.4895833340161175, -4.445597072760115509, -7.700000000000001954 ) ) ;
#48942 = FACE_OUTER_BOUND ( 'NONE', #17064, .T. ) ;
#48943 = FACE_OUTER_BOUND ( 'NONE', #103145, .T. ) ;
#48944 = AXIS2_PLACEMENT_3D ( 'NONE', #97693, #47968, #87859 ) ;
#48945 = AXIS2_PLACEMENT_3D ( 'NONE', #11107, #21591, #39095 ) ;
#48946 = CIRCLE ( 'NONE', #23904, 0.06509327318403743123 ) ;
#48947 = CARTESIAN_POINT ( 'NONE',  ( 11.84999999999990372, 2.500000000000000000, 2.511473670974873507 ) ) ;
#48948 = CARTESIAN_POINT ( 'NONE',  ( -2.950000000000033484, 2.500000000000000000, -6.595190528383302109 ) ) ;
#48949 = AXIS2_PLACEMENT_3D ( 'NONE', #95801, #45426, #63777 ) ;
#48950 = DIRECTION ( 'NONE',  ( 0.000000000000000000, 0.000000000000000000, 1.000000000000000000 ) ) ;
#48951 = CONICAL_SURFACE ( 'NONE', #908, 0.1000000000000000056, 0.003490658503988666988 ) ;
#48952 = EDGE_CURVE ( 'NONE', #91341, #69398, #37235, .T. ) ;
#48953 = DIRECTION ( 'NONE',  ( 0.000000000000000000, 1.000000000000000000, 0.000000000000000000 ) ) ;
#48954 = ORIENTED_EDGE ( 'NONE', *, *, #34308, .T. ) ;
#48955 = ORIENTED_EDGE ( 'NONE', *, *, #115752, .F. ) ;
#48956 = EDGE_LOOP ( 'NONE', ( #76868, #24181 ) ) ;
#48957 = EDGE_LOOP ( 'NONE', ( #127374, #33632, #44144, #110091 ) ) ;
#48958 = DIRECTION ( 'NONE',  ( 0.000000000000000000, 0.000000000000000000, -1.000000000000000000 ) ) ;
#48959 = EDGE_CURVE ( 'NONE', #64702, #16084, #97848, .T. ) ;
#48960 = CARTESIAN_POINT ( 'NONE',  ( -3.150000000000030553, 2.500000000000000000, 6.048780366869520364 ) ) ;
#48961 = FACE_BOUND ( 'NONE', #85376, .T. ) ;
#48962 = EDGE_CURVE ( 'NONE', #68417, #66442, #107219, .T. ) ;
#48963 = CARTESIAN_POINT ( 'NONE',  ( -11.89999999999999503, 2.500000000000000000, 3.983716857408420076 ) ) ;
#48964 = ADVANCED_FACE ( 'NONE', ( #87570 ), #28921, .T. ) ;
#48965 = VECTOR ( 'NONE', #77043, 1000.000000000000000 ) ;
#48966 = ADVANCED_FACE ( 'NONE', ( #79068 ), #102070, .T. ) ;
#48968 = VERTEX_POINT ( 'NONE', #78436 ) ;
#48967 = AXIS2_PLACEMENT_3D ( 'NONE', #19373, #27923, #59344 ) ;
#48970 = AXIS2_PLACEMENT_3D ( 'NONE', #101301, #71842, #29987 ) ;
#48969 = DIRECTION ( 'NONE',  ( 0.000000000000000000, 0.000000000000000000, 1.000000000000000000 ) ) ;
#48971 = LINE ( 'NONE', #88875, #53578 ) ;
#48972 = DIRECTION ( 'NONE',  ( 0.000000000000000000, 0.000000000000000000, 1.000000000000000000 ) ) ;
#48973 = EDGE_CURVE ( 'NONE', #68081, #20474, #47695, .T. ) ;
#48974 = DIRECTION ( 'NONE',  ( 0.000000000000000000, 0.000000000000000000, 1.000000000000000000 ) ) ;
#48975 = ORIENTED_EDGE ( 'NONE', *, *, #3901, .F. ) ;
#48976 = CARTESIAN_POINT ( 'NONE',  ( 3.149999999999946176, 12.50000000000000000, -6.148780366869526226 ) ) ;
#48977 = CIRCLE ( 'NONE', #13444, 0.1000000000000002554 ) ;
#48978 = AXIS2_PLACEMENT_3D ( 'NONE', #4256, #114866, #13445 ) ;
#48979 = CIRCLE ( 'NONE', #126232, 0.09999999999999982514 ) ;
#48981 = EDGE_LOOP ( 'NONE', ( #16233, #68716 ) ) ;
#48980 = AXIS2_PLACEMENT_3D ( 'NONE', #97614, #124668, #7936 ) ;
#48982 = ORIENTED_EDGE ( 'NONE', *, *, #5112, .F. ) ;
#48983 = DIRECTION ( 'NONE',  ( -0.000000000000000000, -1.000000000000000000, -0.000000000000000000 ) ) ;
#48984 = DIRECTION ( 'NONE',  ( 0.000000000000000000, 0.000000000000000000, -1.000000000000000000 ) ) ;
#48985 = EDGE_LOOP ( 'NONE', ( #107616, #86160, #123154, #36793 ) ) ;
#48986 = CONICAL_SURFACE ( 'NONE', #46930, 0.09999999999999982514, 0.003490658503988666988 ) ;
#48987 = VECTOR ( 'NONE', #22163, 1000.000000000000000 ) ;
#48988 = AXIS2_PLACEMENT_3D ( 'NONE', #17861, #78749, #118640 ) ;
#48989 = DIRECTION ( 'NONE',  ( 0.000000000000000000, 1.000000000000000000, 0.000000000000000000 ) ) ;
#48990 = FACE_OUTER_BOUND ( 'NONE', #41688, .T. ) ;
#48991 = VERTEX_POINT ( 'NONE', #118975 ) ;
#48992 = DIRECTION ( 'NONE',  ( 0.000000000000000000, 0.000000000000000000, 1.000000000000000000 ) ) ;
#48994 = EDGE_LOOP ( 'NONE', ( #7965, #48802, #94307, #27443 ) ) ;
#48993 = CONICAL_SURFACE ( 'NONE', #46940, 0.09999999999999999167, 0.003490658503988666988 ) ;
#48995 = DIRECTION ( 'NONE',  ( 0.000000000000000000, 0.000000000000000000, 1.000000000000000000 ) ) ;
#48996 = ORIENTED_EDGE ( 'NONE', *, *, #49037, .F. ) ;
#48997 = PLANE ( 'NONE',  #51319 ) ;
#48998 = FACE_BOUND ( 'NONE', #5620, .T. ) ;
#48999 = ORIENTED_EDGE ( 'NONE', *, *, #91798, .F. ) ;
#49000 = CARTESIAN_POINT ( 'NONE',  ( 110.5253642625963835, 6.372598327064348922, -4.327233595554000445 ) ) ;
#49001 = ORIENTED_EDGE ( 'NONE', *, *, #85274, .T. ) ;
#49002 = CARTESIAN_POINT ( 'NONE',  ( -5.650000000000023448, 2.500000000000000000, -2.611473670974877592 ) ) ;
#49003 = DIRECTION ( 'NONE',  ( 0.000000000000000000, 0.000000000000000000, 1.000000000000000000 ) ) ;
#49004 = CARTESIAN_POINT ( 'NONE',  ( 2.699999999999947331, 12.50000000000000000, -4.676537180435978769 ) ) ;
#49005 = FACE_OUTER_BOUND ( 'NONE', #35710, .T. ) ;
#49006 = DIRECTION ( 'NONE',  ( 0.000000000000000000, 0.000000000000000000, 1.000000000000000000 ) ) ;
#49007 = CIRCLE ( 'NONE', #122162, 0.06509327318403741736 ) ;
#49008 = VERTEX_POINT ( 'NONE', #14467 ) ;
#49009 = ORIENTED_EDGE ( 'NONE', *, *, #55522, .F. ) ;
#49010 = VERTEX_POINT ( 'NONE', #28673 ) ;
#49011 = DIRECTION ( 'NONE',  ( -4.274815082592931898E-19, -0.9999939076577903929, -0.003490651415223739937 ) ) ;
#49012 = DIRECTION ( 'NONE',  ( 0.000000000000000000, -0.000000000000000000, 1.000000000000000000 ) ) ;
#49014 = EDGE_CURVE ( 'NONE', #24765, #27897, #64405, .T. ) ;
#49013 = CARTESIAN_POINT ( 'NONE',  ( 4.599999999999940137, 12.50000000000000000, -5.022947341949754119 ) ) ;
#49016 = EDGE_LOOP ( 'NONE', ( #30052, #83094 ) ) ;
#49015 = VERTEX_POINT ( 'NONE', #69217 ) ;
#49017 = ORIENTED_EDGE ( 'NONE', *, *, #100064, .F. ) ;
#49018 = EDGE_CURVE ( 'NONE', #109103, #73593, #37836, .T. ) ;
#49019 = PLANE ( 'NONE',  #83330 ) ;
#49020 = EDGE_CURVE ( 'NONE', #29970, #128096, #86274, .T. ) ;
#49021 = AXIS2_PLACEMENT_3D ( 'NONE', #18689, #69076, #60580 ) ;
#49022 = FACE_OUTER_BOUND ( 'NONE', #47069, .T. ) ;
#49023 = AXIS2_PLACEMENT_3D ( 'NONE', #53609, #63424, #71968 ) ;
#49024 = CARTESIAN_POINT ( 'NONE',  ( 8.349999999999919709, 2.500000000000000000, -2.165063509461101710 ) ) ;
#49025 = DIRECTION ( 'NONE',  ( 0.000000000000000000, 1.000000000000000000, 0.000000000000000000 ) ) ;
#49026 = DIRECTION ( 'NONE',  ( 0.000000000000000000, 1.000000000000000000, 0.000000000000000000 ) ) ;
#49027 = CARTESIAN_POINT ( 'NONE',  ( -4.400000000000028777, 12.50000000000000000, -4.676537180435978769 ) ) ;
#49028 = CARTESIAN_POINT ( 'NONE',  ( -11.25000000000000178, 12.50000000000000000, -5.737276932171709198 ) ) ;
#49029 = EDGE_CURVE ( 'NONE', #123681, #57299, #3859, .T. ) ;
#49030 = EDGE_CURVE ( 'NONE', #94355, #44902, #97399, .T. ) ;
#49031 = DIRECTION ( 'NONE',  ( 0.000000000000000000, -0.9999939076577903929, 0.003490651415223739937 ) ) ;
#49032 = EDGE_CURVE ( 'NONE', #50883, #108236, #77023, .T. ) ;
#49033 = VERTEX_POINT ( 'NONE', #127515 ) ;
#49035 = ORIENTED_EDGE ( 'NONE', *, *, #17925, .F. ) ;
#49034 = EDGE_CURVE ( 'NONE', #18830, #93842, #93755, .T. ) ;
#49036 = DIRECTION ( 'NONE',  ( 0.000000000000000000, 0.000000000000000000, 1.000000000000000000 ) ) ;
#49037 = EDGE_CURVE ( 'NONE', #63511, #53411, #22658, .T. ) ;
#49038 = CARTESIAN_POINT ( 'NONE',  ( 4.149999999999936406, 2.500000000000000000, 6.395190528383296602 ) ) ;
#49039 = ORIENTED_EDGE ( 'NONE', *, *, #16327, .T. ) ;
#49040 = ORIENTED_EDGE ( 'NONE', *, *, #73994, .T. ) ;
#49041 = CARTESIAN_POINT ( 'NONE',  ( 185.6093750003413732, 9.264065473108010111E-16, -7.564683531250000925 ) ) ;
#49042 = DIRECTION ( 'NONE',  ( 0.000000000000000000, 0.000000000000000000, -1.000000000000000000 ) ) ;
#49043 = DIRECTION ( 'NONE',  ( 0.000000000000000000, 0.000000000000000000, 1.000000000000000000 ) ) ;
#49044 = ADVANCED_FACE ( 'NONE', ( #68579 ), #18440, .T. ) ;
#49045 = LINE ( 'NONE', #79146, #121500 ) ;
#49046 = CIRCLE ( 'NONE', #61558, 0.09999999999999982514 ) ;
#49047 = CARTESIAN_POINT ( 'NONE',  ( 184.5312500006828031, 9.429780353434619030E-16, -7.700000000000000178 ) ) ;
#49048 = AXIS2_PLACEMENT_3D ( 'NONE', #115584, #14787, #35133 ) ;
#49049 = LINE ( 'NONE', #69964, #26003 ) ;
#49050 = DIRECTION ( 'NONE',  ( 0.000000000000000000, 1.000000000000000000, 0.000000000000000000 ) ) ;
#49051 = CIRCLE ( 'NONE', #17623, 0.1000000000000000472 ) ;
#49052 = CIRCLE ( 'NONE', #72115, 0.1000000000000000472 ) ;
#49053 = CARTESIAN_POINT ( 'NONE',  ( -4.800000000000024691, 2.500000000000000000, 0.3464101615137735735 ) ) ;
#49054 = VERTEX_POINT ( 'NONE', #47031 ) ;
#49055 = ORIENTED_EDGE ( 'NONE', *, *, #9016, .F. ) ;
#49056 = VERTEX_POINT ( 'NONE', #47670 ) ;
#49057 = ORIENTED_EDGE ( 'NONE', *, *, #63482, .F. ) ;
#49058 = CARTESIAN_POINT ( 'NONE',  ( -8.150000000000012790, 2.500000000000000000, -1.718653347947326049 ) ) ;
#49059 = LINE ( 'NONE', #129565, #79147 ) ;
#49060 = EDGE_LOOP ( 'NONE', ( #80388, #42594, #104913, #9331 ) ) ;
#49061 = DIRECTION ( 'NONE',  ( 0.000000000000000000, 0.000000000000000000, 1.000000000000000000 ) ) ;
#49062 = CARTESIAN_POINT ( 'NONE',  ( 3.949999999999938005, 2.500000000000000000, 6.841600689897072485 ) ) ;
#49063 = CIRCLE ( 'NONE', #122210, 0.1000000000000002554 ) ;
#49064 = AXIS2_PLACEMENT_3D ( 'NONE', #42278, #13441, #2321 ) ;
#49065 = LINE ( 'NONE', #77849, #118001 ) ;
#49067 = ORIENTED_EDGE ( 'NONE', *, *, #95497, .F. ) ;
#49066 = LINE ( 'NONE', #109911, #43365 ) ;
#49068 = AXIS2_PLACEMENT_3D ( 'NONE', #95230, #55301, #5538 ) ;
#49069 = DIRECTION ( 'NONE',  ( 0.000000000000000000, 0.000000000000000000, -1.000000000000000000 ) ) ;
#49070 = DIRECTION ( 'NONE',  ( -0.000000000000000000, 1.000000000000000000, -0.000000000000000000 ) ) ;
#49071 = VERTEX_POINT ( 'NONE', #48305 ) ;
#49072 = AXIS2_PLACEMENT_3D ( 'NONE', #111118, #10992, #70576 ) ;
#49073 = EDGE_CURVE ( 'NONE', #28513, #29920, #114568, .T. ) ;
#49074 = CIRCLE ( 'NONE', #67828, 0.06509327318403745899 ) ;
#49075 = AXIS2_PLACEMENT_3D ( 'NONE', #54513, #112812, #14585 ) ;
#49076 = ORIENTED_EDGE ( 'NONE', *, *, #44362, .F. ) ;
#49077 = ORIENTED_EDGE ( 'NONE', *, *, #20766, .T. ) ;
#49078 = EDGE_LOOP ( 'NONE', ( #1431, #102473 ) ) ;
#49079 = DIRECTION ( 'NONE',  ( 0.000000000000000000, 0.000000000000000000, 1.000000000000000000 ) ) ;
#49080 = CIRCLE ( 'NONE', #118291, 0.06509327318403741736 ) ;
#49081 = DIRECTION ( 'NONE',  ( 0.000000000000000000, -0.9999939076577903929, 0.003490651415223739937 ) ) ;
#49082 = CARTESIAN_POINT ( 'NONE',  ( 14.99999999999989164, 2.500000000000000000, 0.6928203230275494784 ) ) ;
#49083 = CIRCLE ( 'NONE', #99252, 0.1000000000000002554 ) ;
#49084 = AXIS2_PLACEMENT_3D ( 'NONE', #43178, #52979, #83095 ) ;
#49085 = AXIS2_PLACEMENT_3D ( 'NONE', #97329, #7644, #95396 ) ;
#49086 = EDGE_LOOP ( 'NONE', ( #124160, #14890 ) ) ;
#49087 = DIRECTION ( 'NONE',  ( 0.000000000000000000, -0.000000000000000000, -1.000000000000000000 ) ) ;
#49088 = DIRECTION ( 'NONE',  ( 0.000000000000000000, -0.000000000000000000, 1.000000000000000000 ) ) ;
#49089 = EDGE_CURVE ( 'NONE', #33171, #102865, #18836, .T. ) ;
#49090 = CARTESIAN_POINT ( 'NONE',  ( -8.550000000000014921, 2.500000000000000000, -6.248780366869521430 ) ) ;
#49091 = DIRECTION ( 'NONE',  ( 1.000000000000000000, 0.000000000000000000, 0.000000000000000000 ) ) ;
#49092 = VERTEX_POINT ( 'NONE', #58773 ) ;
#49093 = DIRECTION ( 'NONE',  ( 0.000000000000000000, 0.000000000000000000, 1.000000000000000000 ) ) ;
#49094 = ORIENTED_EDGE ( 'NONE', *, *, #110731, .F. ) ;
#49095 = EDGE_LOOP ( 'NONE', ( #124256, #56400, #43620, #67947 ) ) ;
#49096 = PLANE ( 'NONE',  #16224 ) ;
#49097 = DIRECTION ( 'NONE',  ( -0.000000000000000000, 1.000000000000000000, -0.000000000000000000 ) ) ;
#49098 = FACE_BOUND ( 'NONE', #79508, .T. ) ;
#49099 = DIRECTION ( 'NONE',  ( -4.274815082592931898E-19, -0.9999939076577903929, -0.003490651415223739937 ) ) ;
#49100 = CONICAL_SURFACE ( 'NONE', #74133, 0.1000000000000000056, 0.003490658503988666988 ) ;
#49101 = DIRECTION ( 'NONE',  ( 0.000000000000000000, 0.000000000000000000, 1.000000000000000000 ) ) ;
#49102 = PLANE ( 'NONE',  #56456 ) ;
#49103 = EDGE_LOOP ( 'NONE', ( #35193, #57057, #66304, #36764 ) ) ;
#49104 = FACE_OUTER_BOUND ( 'NONE', #85836, .T. ) ;
#49105 = DIRECTION ( 'NONE',  ( 0.000000000000000000, 0.000000000000000000, 1.000000000000000000 ) ) ;
#49106 = CARTESIAN_POINT ( 'NONE',  ( -12.89999999999999147, 2.500000000000000000, 4.230127018922196669 ) ) ;
#49107 = DIRECTION ( 'NONE',  ( 0.000000000000000000, -0.000000000000000000, 1.000000000000000000 ) ) ;
#49108 = VERTEX_POINT ( 'NONE', #96741 ) ;
#49109 = AXIS2_PLACEMENT_3D ( 'NONE', #19323, #68432, #109661 ) ;
#49110 = CONICAL_SURFACE ( 'NONE', #59590, 0.1000000000000002554, 0.003490658503988666988 ) ;
#49111 = DIRECTION ( 'NONE',  ( 0.000000000000000000, 1.000000000000000000, 0.000000000000000000 ) ) ;
#49112 = EDGE_CURVE ( 'NONE', #64688, #61872, #7966, .T. ) ;
#49113 = FACE_OUTER_BOUND ( 'NONE', #771, .T. ) ;
#49114 = VERTEX_POINT ( 'NONE', #1766 ) ;
#49115 = ORIENTED_EDGE ( 'NONE', *, *, #123838, .T. ) ;
#49116 = DIRECTION ( 'NONE',  ( 0.000000000000000000, 0.000000000000000000, 1.000000000000000000 ) ) ;
#49117 = DIRECTION ( 'NONE',  ( 0.000000000000000000, 0.000000000000000000, 1.000000000000000000 ) ) ;
#49118 = FACE_BOUND ( 'NONE', #57384, .T. ) ;
#49119 = EDGE_CURVE ( 'NONE', #125645, #86214, #108315, .T. ) ;
#49120 = CARTESIAN_POINT ( 'NONE',  ( 1.699999999999951994, 2.500000000000000000, -4.330127018922201643 ) ) ;
#49121 = CIRCLE ( 'NONE', #82566, 0.1000000000000002554 ) ;
#49122 = VERTEX_POINT ( 'NONE', #70514 ) ;
#49123 = FACE_OUTER_BOUND ( 'NONE', #92791, .T. ) ;
#49124 = CIRCLE ( 'NONE', #59602, 0.06509327318403745899 ) ;
#49125 = ADVANCED_FACE ( 'NONE', ( #20783 ), #72829, .T. ) ;
#49126 = EDGE_CURVE ( 'NONE', #109569, #17430, #125041, .T. ) ;
#49127 = ORIENTED_EDGE ( 'NONE', *, *, #124788, .F. ) ;
#49128 = CARTESIAN_POINT ( 'NONE',  ( 12.09999999999990550, 2.500000000000000000, 3.537306695894645081 ) ) ;
#49129 = ADVANCED_FACE ( 'NONE', ( #50886 ), #129378, .T. ) ;
#49130 = ADVANCED_FACE ( 'NONE', ( #99349 ), #24797, .T. ) ;
#49131 = CARTESIAN_POINT ( 'NONE',  ( 184.2135416670080588, 4.367472073101518859, -7.564683531249999149 ) ) ;
#49132 = ADVANCED_FACE ( 'NONE', ( #71819 ), #2400, .T. ) ;
#49133 = EDGE_LOOP ( 'NONE', ( #122299, #105879 ) ) ;
#49134 = DIRECTION ( 'NONE',  ( 0.000000000000000000, 0.000000000000000000, 1.000000000000000000 ) ) ;
#49135 = DIRECTION ( 'NONE',  ( -1.000000000000000000, -0.000000000000000000, -0.000000000000000000 ) ) ;
#49136 = AXIS2_PLACEMENT_3D ( 'NONE', #57631, #99494, #9813 ) ;
#49137 = AXIS2_PLACEMENT_3D ( 'NONE', #89996, #99846, #316 ) ;
#49138 = DIRECTION ( 'NONE',  ( 0.000000000000000000, 1.000000000000000000, 0.000000000000000000 ) ) ;
#49140 = ADVANCED_FACE ( 'NONE', ( #82286 ), #129474, .T. ) ;
#49139 = FACE_OUTER_BOUND ( 'NONE', #108080, .T. ) ;
#49141 = EDGE_CURVE ( 'NONE', #66521, #107226, #50248, .T. ) ;
#49142 = ADVANCED_FACE ( 'NONE', ( #122209 ), #60413, .T. ) ;
#49143 = EDGE_LOOP ( 'NONE', ( #153, #31503, #36017, #68767 ) ) ;
#49144 = CARTESIAN_POINT ( 'NONE',  ( 2.899999999999946620, 12.50000000000000000, -5.022947341949754119 ) ) ;
#49145 = CARTESIAN_POINT ( 'NONE',  ( 0.6499999999999561684, 2.500000000000000000, -1.918653347947325782 ) ) ;
#49146 = CARTESIAN_POINT ( 'NONE',  ( 13.74999999999989697, 2.500000000000000000, 2.757883832488649656 ) ) ;
#49147 = DIRECTION ( 'NONE',  ( -4.274815082592931898E-19, -0.9999939076577903929, -0.003490651415223739937 ) ) ;
#49148 = ORIENTED_EDGE ( 'NONE', *, *, #119846, .F. ) ;
#49149 = VERTEX_POINT ( 'NONE', #60712 ) ;
#49150 = CARTESIAN_POINT ( 'NONE',  ( 15.83209681635555377, 2.500000000000000000, 5.404881881984148428 ) ) ;
#49151 = AXIS2_PLACEMENT_3D ( 'NONE', #115135, #25484, #34034 ) ;
#49152 = ORIENTED_EDGE ( 'NONE', *, *, #20185, .T. ) ;
#49153 = CARTESIAN_POINT ( 'NONE',  ( -7.900000000000014566, 12.50000000000000000, -2.276824562219559311E-15 ) ) ;
#49154 = DIRECTION ( 'NONE',  ( -0.000000000000000000, -1.000000000000000000, -0.000000000000000000 ) ) ;
#49155 = CARTESIAN_POINT ( 'NONE',  ( -9.150000000000005684, 2.500000000000000000, 7.088010851410848190 ) ) ;
#49157 = CARTESIAN_POINT ( 'NONE',  ( -1.050000000000037792, 2.500000000000000000, 6.048780366869520364 ) ) ;
#49156 = AXIS2_PLACEMENT_3D ( 'NONE', #58223, #107941, #66077 ) ;
#49158 = ORIENTED_EDGE ( 'NONE', *, *, #21934, .T. ) ;
#49159 = CONICAL_SURFACE ( 'NONE', #61767, 0.1000000000000002554, 0.003490658503988666988 ) ;
#49160 = CARTESIAN_POINT ( 'NONE',  ( 13.34999999999990017, 2.500000000000000000, 2.065063509461097624 ) ) ;
#49161 = LINE ( 'NONE', #119164, #66877 ) ;
#49162 = CARTESIAN_POINT ( 'NONE',  ( 5.849999999999933920, 12.50000000000000000, 6.495190528383297135 ) ) ;
#49163 = AXIS2_PLACEMENT_3D ( 'NONE', #38, #20334, #19690 ) ;
#49164 = CARTESIAN_POINT ( 'NONE',  ( 184.5677083336747444, -4.367472073101514418, -7.564683531250002702 ) ) ;
#49165 = DIRECTION ( 'NONE',  ( 0.000000000000000000, -0.9999939076577903929, 0.003490651415223739937 ) ) ;
#49166 = PLANE ( 'NONE',  #66217 ) ;
#49167 = ORIENTED_EDGE ( 'NONE', *, *, #2846, .F. ) ;
#49169 = ORIENTED_EDGE ( 'NONE', *, *, #63007, .T. ) ;
#49168 = VECTOR ( 'NONE', #44463, 1000.000000000000000 ) ;
#49171 = CARTESIAN_POINT ( 'NONE',  ( -5.850000000000022737, 12.50000000000000000, -6.495190528383302464 ) ) ;
#49170 = CONICAL_SURFACE ( 'NONE', #57472, 0.09999999999999999167, 0.003490658503988666988 ) ;
#49172 = ORIENTED_EDGE ( 'NONE', *, *, #46927, .F. ) ;
#49173 = CARTESIAN_POINT ( 'NONE',  ( 107.6614812150378953, 5.855766388782979170, 4.999999999999952927 ) ) ;
#49176 = EDGE_LOOP ( 'NONE', ( #111303, #61206 ) ) ;
#49175 = EDGE_LOOP ( 'NONE', ( #81360, #96452 ) ) ;
#49174 = AXIS2_PLACEMENT_3D ( 'NONE', #62746, #55493, #53561 ) ;
#49177 = ORIENTED_EDGE ( 'NONE', *, *, #108373, .F. ) ;
#49178 = DIRECTION ( 'NONE',  ( 0.000000000000000000, -0.000000000000000000, 1.000000000000000000 ) ) ;
#49179 = EDGE_CURVE ( 'NONE', #64508, #87351, #33223, .T. ) ;
#49180 = AXIS2_PLACEMENT_3D ( 'NONE', #44860, #83498, #112942 ) ;
#49182 = CIRCLE ( 'NONE', #57478, 0.06509327318403745899 ) ;
#49181 = CARTESIAN_POINT ( 'NONE',  ( 179.5000000000000000, 0.6250000000000000000, 7.634788798650556707 ) ) ;
#49183 = DIRECTION ( 'NONE',  ( -0.000000000000000000, -1.000000000000000000, -0.000000000000000000 ) ) ;
#49184 = ADVANCED_FACE ( 'NONE', ( #29965 ), #102160, .T. ) ;
#49185 = DIRECTION ( 'NONE',  ( 0.000000000000000000, 0.000000000000000000, 1.000000000000000000 ) ) ;
#49186 = DIRECTION ( 'NONE',  ( -0.000000000000000000, 1.000000000000000000, -0.000000000000000000 ) ) ;
#49187 = AXIS2_PLACEMENT_3D ( 'NONE', #395, #11523, #90733 ) ;
#49188 = DIRECTION ( 'NONE',  ( -4.274815082592931898E-19, -0.9999939076577903929, -0.003490651415223739937 ) ) ;
#49189 = DIRECTION ( 'NONE',  ( 0.000000000000000000, 0.000000000000000000, 1.000000000000000000 ) ) ;
#49190 = ADVANCED_FACE ( 'NONE', ( #19479 ), #41540, .T. ) ;
#49191 = CARTESIAN_POINT ( 'NONE',  ( -10.00000000000000533, 12.50000000000000000, -5.022947341949749678 ) ) ;
#49192 = EDGE_LOOP ( 'NONE', ( #2861, #35322 ) ) ;
#49193 = ADVANCED_FACE ( 'NONE', ( #101269 ), #41089, .T. ) ;
#49194 = ORIENTED_EDGE ( 'NONE', *, *, #31488, .F. ) ;
#49195 = EDGE_CURVE ( 'NONE', #64554, #43896, #120905, .T. ) ;
#49196 = DIRECTION ( 'NONE',  ( 0.000000000000000000, 0.000000000000000000, 1.000000000000000000 ) ) ;
#49197 = ORIENTED_EDGE ( 'NONE', *, *, #73347, .T. ) ;
#49198 = EDGE_LOOP ( 'NONE', ( #27794, #5107, #98809, #18739 ) ) ;
#49199 = DIRECTION ( 'NONE',  ( -4.274815082592931898E-19, -0.9999939076577903929, -0.003490651415223739937 ) ) ;
#49200 = AXIS2_PLACEMENT_3D ( 'NONE', #75503, #38173, #76169 ) ;
#49201 = EDGE_CURVE ( 'NONE', #27399, #48060, #109807, .T. ) ;
#49202 = DIRECTION ( 'NONE',  ( -4.274815082592931898E-19, -0.9999939076577903929, -0.003490651415223739937 ) ) ;
#49203 = PLANE ( 'NONE',  #35893 ) ;
#49204 = LINE ( 'NONE', #71373, #95022 ) ;
#49205 = DIRECTION ( 'NONE',  ( 0.000000000000000000, -0.9999939076577903929, 0.003490651415223739937 ) ) ;
#49206 = ORIENTED_EDGE ( 'NONE', *, *, #27416, .F. ) ;
#49207 = AXIS2_PLACEMENT_3D ( 'NONE', #55723, #65542, #115257 ) ;
#49208 = AXIS2_PLACEMENT_3D ( 'NONE', #114173, #55255, #104348 ) ;
#49209 = VECTOR ( 'NONE', #111721, 1000.000000000000000 ) ;
#49210 = VERTEX_POINT ( 'NONE', #21418 ) ;
#49211 = DIRECTION ( 'NONE',  ( -0.000000000000000000, 1.000000000000000000, -0.000000000000000000 ) ) ;
#49212 = ORIENTED_EDGE ( 'NONE', *, *, #70626, .T. ) ;
#49213 = DIRECTION ( 'NONE',  ( 0.000000000000000000, 0.000000000000000000, -1.000000000000000000 ) ) ;
#49214 = EDGE_LOOP ( 'NONE', ( #52904, #31692, #13433, #37798 ) ) ;
#49215 = ADVANCED_FACE ( 'NONE', ( #31894 ), #93841, .T. ) ;
#49216 = ORIENTED_EDGE ( 'NONE', *, *, #52059, .F. ) ;
#49217 = DIRECTION ( 'NONE',  ( 0.000000000000000000, 1.000000000000000000, 0.000000000000000000 ) ) ;
#49218 = LINE ( 'NONE', #70134, #50601 ) ;
#49219 = AXIS2_PLACEMENT_3D ( 'NONE', #64840, #13149, #123749 ) ;
#49220 = DIRECTION ( 'NONE',  ( -0.000000000000000000, -1.000000000000000000, -0.000000000000000000 ) ) ;
#49221 = DIRECTION ( 'NONE',  ( -0.000000000000000000, -1.000000000000000000, -0.000000000000000000 ) ) ;
#49222 = CIRCLE ( 'NONE', #111994, 0.06509327318403745899 ) ;
#49223 = CARTESIAN_POINT ( 'NONE',  ( -7.950000000000009059, 12.50000000000000000, 6.495190528383297135 ) ) ;
#49224 = VERTEX_POINT ( 'NONE', #124126 ) ;
#49225 = DIRECTION ( 'NONE',  ( -4.274815082592931898E-19, -0.9999939076577903929, -0.003490651415223739937 ) ) ;
#49226 = DIRECTION ( 'NONE',  ( 0.000000000000000000, 0.000000000000000000, -1.000000000000000000 ) ) ;
#49227 = CARTESIAN_POINT ( 'NONE',  ( 13.74999999999993427, 2.500000000000000000, 2.065063509461097624 ) ) ;
#49228 = LINE ( 'NONE', #28283, #101656 ) ;
#49229 = DIRECTION ( 'NONE',  ( -4.274815082592931898E-19, -0.9999939076577903929, -0.003490651415223739937 ) ) ;
#49230 = VERTEX_POINT ( 'NONE', #73730 ) ;
#49231 = CONICAL_SURFACE ( 'NONE', #107700, 0.1000000000000000472, 0.003490658503988666988 ) ;
#49232 = AXIS2_PLACEMENT_3D ( 'NONE', #8067, #37549, #99036 ) ;
#49233 = EDGE_CURVE ( 'NONE', #99389, #55154, #29010, .T. ) ;
#49234 = EDGE_LOOP ( 'NONE', ( #3816, #5135, #61436, #56946 ) ) ;
#49235 = CARTESIAN_POINT ( 'NONE',  ( -1.650000000000034328, 2.500000000000000000, -2.757883832488654097 ) ) ;
#49236 = VERTEX_POINT ( 'NONE', #84197 ) ;
#49237 = DIRECTION ( 'NONE',  ( 0.000000000000000000, 0.000000000000000000, 1.000000000000000000 ) ) ;
#49238 = CARTESIAN_POINT ( 'NONE',  ( 2.499999999999947153, 12.50000000000000000, -3.702399969078687292 ) ) ;
#49239 = ORIENTED_EDGE ( 'NONE', *, *, #78258, .F. ) ;
#49240 = CARTESIAN_POINT ( 'NONE',  ( 13.34999999999990017, 2.500000000000000000, 2.065063509461097624 ) ) ;
#49241 = FACE_OUTER_BOUND ( 'NONE', #48985, .T. ) ;
#49242 = EDGE_CURVE ( 'NONE', #10224, #82327, #114941, .T. ) ;
#49243 = DIRECTION ( 'NONE',  ( 0.000000000000000000, 1.000000000000000000, 0.000000000000000000 ) ) ;
#49244 = VECTOR ( 'NONE', #18251, 1000.000000000000000 ) ;
#49245 = DIRECTION ( 'NONE',  ( 0.000000000000000000, 0.000000000000000000, 1.000000000000000000 ) ) ;
#49246 = EDGE_LOOP ( 'NONE', ( #86440, #127359, #110430, #94128 ) ) ;
#49247 = DIRECTION ( 'NONE',  ( 0.000000000000000000, 1.000000000000000000, 0.000000000000000000 ) ) ;
#49248 = AXIS2_PLACEMENT_3D ( 'NONE', #94424, #45353, #85262 ) ;
#49249 = ORIENTED_EDGE ( 'NONE', *, *, #106971, .T. ) ;
#49250 = CARTESIAN_POINT ( 'NONE',  ( 21.23528140090949634, 2.699413673072310171, -2.293764360948883141 ) ) ;
#49251 = FACE_OUTER_BOUND ( 'NONE', #56069, .T. ) ;
#49252 = CARTESIAN_POINT ( 'NONE',  ( 0.6499999999999566125, 2.500000000000000000, -6.148780366869526226 ) ) ;
#49253 = VERTEX_POINT ( 'NONE', #22731 ) ;
#49254 = AXIS2_PLACEMENT_3D ( 'NONE', #115986, #54486, #105531 ) ;
#49255 = CARTESIAN_POINT ( 'NONE',  ( 1.649999999999950617, 2.500000000000000000, -2.165063509461101710 ) ) ;
#49256 = CONICAL_SURFACE ( 'NONE', #59728, 0.1000000000000002554, 0.003490658503988666988 ) ;
#49257 = ORIENTED_EDGE ( 'NONE', *, *, #44869, .T. ) ;
#49258 = DIRECTION ( 'NONE',  ( 0.000000000000000000, 0.000000000000000000, 1.000000000000000000 ) ) ;
#49259 = DIRECTION ( 'NONE',  ( -0.000000000000000000, 1.000000000000000000, -0.000000000000000000 ) ) ;
#49260 = DIRECTION ( 'NONE',  ( 0.000000000000000000, 1.000000000000000000, 0.000000000000000000 ) ) ;
#49261 = ORIENTED_EDGE ( 'NONE', *, *, #122072, .F. ) ;
#49262 = AXIS2_PLACEMENT_3D ( 'NONE', #36968, #38927, #106968 ) ;
#49263 = VECTOR ( 'NONE', #99035, 1000.000000000000000 ) ;
#49264 = CARTESIAN_POINT ( 'NONE',  ( 7.699999999999923794, 2.500000000000000000, 4.776537180435972196 ) ) ;
#49266 = ADVANCED_FACE ( 'NONE', ( #73103 ), #44273, .T. ) ;
#49265 = CIRCLE ( 'NONE', #118202, 0.06509327318403745899 ) ;
#49267 = LINE ( 'NONE', #117301, #11877 ) ;
#49268 = CONICAL_SURFACE ( 'NONE', #74382, 0.1000000000000002554, 0.003490658503988666988 ) ;
#49269 = ORIENTED_EDGE ( 'NONE', *, *, #100239, .F. ) ;
#49270 = PLANE ( 'NONE',  #34283 ) ;
#49271 = ORIENTED_EDGE ( 'NONE', *, *, #89737, .T. ) ;
#49272 = LINE ( 'NONE', #79999, #124779 ) ;
#49273 = ADVANCED_FACE ( 'NONE', ( #113673 ), #74388, .T. ) ;
#49274 = EDGE_LOOP ( 'NONE', ( #46981, #20468, #100656, #14778 ) ) ;
#49275 = DIRECTION ( 'NONE',  ( -0.000000000000000000, -1.000000000000000000, -0.000000000000000000 ) ) ;
#49276 = CARTESIAN_POINT ( 'NONE',  ( 183.9609375001707008, 0.000000000000000000, 7.632341765625000107 ) ) ;
#49277 = ADVANCED_FACE ( 'NONE', ( #14159 ), #85426, .T. ) ;
#49278 = ORIENTED_EDGE ( 'NONE', *, *, #112240, .F. ) ;
#49279 = ADVANCED_FACE ( 'NONE', ( #102550 ), #14310, .T. ) ;
#49280 = ORIENTED_EDGE ( 'NONE', *, *, #120476, .F. ) ;
#49281 = EDGE_CURVE ( 'NONE', #67302, #12498, #43693, .T. ) ;
#49282 = EDGE_CURVE ( 'NONE', #66379, #55337, #54132, .T. ) ;
#49283 = CARTESIAN_POINT ( 'NONE',  ( -1.650000000000035216, 12.50000000000000000, -5.802370205355749988 ) ) ;
#49284 = CARTESIAN_POINT ( 'NONE',  ( -3.550000000000030909, 2.500000000000000000, -6.741600689897078169 ) ) ;
#49285 = AXIS2_PLACEMENT_3D ( 'NONE', #65535, #7897, #26269 ) ;
#49286 = ORIENTED_EDGE ( 'NONE', *, *, #105533, .F. ) ;
#49287 = DIRECTION ( 'NONE',  ( 0.000000000000000000, -0.000000000000000000, 1.000000000000000000 ) ) ;
#49288 = CARTESIAN_POINT ( 'NONE',  ( -6.900000000000019007, 2.500000000000000000, -3.983716857408426293 ) ) ;
#49289 = ADVANCED_FACE ( 'NONE', ( #94025 ), #43029, .T. ) ;
#49290 = CARTESIAN_POINT ( 'NONE',  ( 104.9451419649933115, 7.743416704392222627, -3.971277570916745603 ) ) ;
#49291 = DIRECTION ( 'NONE',  ( -0.000000000000000000, -1.000000000000000000, -0.000000000000000000 ) ) ;
#49292 = ADVANCED_FACE ( 'NONE', ( #3078 ), #108409, .T. ) ;
#49293 = CARTESIAN_POINT ( 'NONE',  ( -6.450000000000014388, 2.500000000000000000, 6.048780366869521252 ) ) ;
#49294 = AXIS2_PLACEMENT_3D ( 'NONE', #29493, #127683, #97577 ) ;
#49295 = DIRECTION ( 'NONE',  ( 0.000000000000000000, 0.000000000000000000, 1.000000000000000000 ) ) ;
#49296 = EDGE_CURVE ( 'NONE', #16549, #128756, #5629, .T. ) ;
#49297 = AXIS2_PLACEMENT_3D ( 'NONE', #107705, #9505, #18019 ) ;
#49298 = EDGE_CURVE ( 'NONE', #66944, #120047, #87472, .T. ) ;
#49299 = EDGE_CURVE ( 'NONE', #58340, #93836, #83579, .T. ) ;
#49300 = EDGE_LOOP ( 'NONE', ( #44582, #30647, #92229, #80880 ) ) ;
#49301 = VECTOR ( 'NONE', #42681, 1000.000000000000000 ) ;
#49302 = EDGE_LOOP ( 'NONE', ( #58732, #81418 ) ) ;
#49303 = ORIENTED_EDGE ( 'NONE', *, *, #69301, .F. ) ;
#49304 = ORIENTED_EDGE ( 'NONE', *, *, #62863, .T. ) ;
#49305 = DIRECTION ( 'NONE',  ( -0.000000000000000000, -1.000000000000000000, -0.000000000000000000 ) ) ;
#49306 = DIRECTION ( 'NONE',  ( 0.000000000000000000, 0.000000000000000000, -1.000000000000000000 ) ) ;
#49307 = CARTESIAN_POINT ( 'NONE',  ( -3.550000000000030909, 2.500000000000000000, -6.841600689897078702 ) ) ;
#49308 = ORIENTED_EDGE ( 'NONE', *, *, #67223, .T. ) ;
#49309 = FACE_BOUND ( 'NONE', #74299, .T. ) ;
#49310 = ORIENTED_EDGE ( 'NONE', *, *, #58323, .T. ) ;
#49311 = EDGE_CURVE ( 'NONE', #77153, #21611, #94663, .T. ) ;
#49312 = DIRECTION ( 'NONE',  ( 0.000000000000000000, 0.000000000000000000, -1.000000000000000000 ) ) ;
#49313 = DIRECTION ( 'NONE',  ( 0.000000000000000000, -0.000000000000000000, 1.000000000000000000 ) ) ;
#49314 = AXIS2_PLACEMENT_3D ( 'NONE', #71958, #33332, #22866 ) ;
#49315 = LINE ( 'NONE', #59118, #13724 ) ;
#49316 = CARTESIAN_POINT ( 'NONE',  ( -1.250000000000035749, 2.500000000000000000, -7.188010851410854052 ) ) ;
#49317 = AXIS2_PLACEMENT_3D ( 'NONE', #90338, #19695, #89715 ) ;
#49318 = DIRECTION ( 'NONE',  ( 0.000000000000000000, 0.000000000000000000, -1.000000000000000000 ) ) ;
#49319 = FACE_OUTER_BOUND ( 'NONE', #35657, .T. ) ;
#49320 = LINE ( 'NONE', #59123, #72880 ) ;
#49321 = CARTESIAN_POINT ( 'NONE',  ( 10.84999999999990905, 12.50000000000000000, -6.495190528383302464 ) ) ;
#49322 = DIRECTION ( 'NONE',  ( -0.000000000000000000, -1.000000000000000000, -0.000000000000000000 ) ) ;
#49323 = CARTESIAN_POINT ( 'NONE',  ( 6.649999999999931966, 12.50000000000000000, -5.867463478539787225 ) ) ;
#49324 = AXIS2_PLACEMENT_3D ( 'NONE', #47343, #47990, #97716 ) ;
#49325 = ORIENTED_EDGE ( 'NONE', *, *, #100274, .F. ) ;
#49326 = VERTEX_POINT ( 'NONE', #124780 ) ;
#49327 = CONICAL_SURFACE ( 'NONE', #114142, 0.1000000000000002554, 0.003490658503988666988 ) ;
#49328 = VERTEX_POINT ( 'NONE', #25265 ) ;
#49329 = VERTEX_POINT ( 'NONE', #35130 ) ;
#49330 = CARTESIAN_POINT ( 'NONE',  ( 17.50000000000000355, -2.500000000000059064, -3.093179327514925081 ) ) ;
#49331 = DIRECTION ( 'NONE',  ( 0.000000000000000000, -0.000000000000000000, 1.000000000000000000 ) ) ;
#49332 = PRODUCT_DEFINITION_CONTEXT ( 'detailed design', #24625, 'design' ) ;
#49334 = ORIENTED_EDGE ( 'NONE', *, *, #78766, .T. ) ;
#49333 = ORIENTED_EDGE ( 'NONE', *, *, #83995, .T. ) ;
#49335 = ORIENTED_EDGE ( 'NONE', *, *, #84854, .F. ) ;
#49336 = CARTESIAN_POINT ( 'NONE',  ( -3.950000000000025491, 2.500000000000000000, 6.248780366869521430 ) ) ;
#49337 = DIRECTION ( 'NONE',  ( 0.000000000000000000, 0.000000000000000000, 1.000000000000000000 ) ) ;
#49338 = DIRECTION ( 'NONE',  ( 0.000000000000000000, 0.000000000000000000, 1.000000000000000000 ) ) ;
#49339 = CARTESIAN_POINT ( 'NONE',  ( -11.05000000000000249, 12.50000000000000000, -1.883746621131359600 ) ) ;
#49340 = CARTESIAN_POINT ( 'NONE',  ( -8.350000000000013856, 12.50000000000000000, -5.802370205355744659 ) ) ;
#49341 = DIRECTION ( 'NONE',  ( 0.000000000000000000, -0.9999939076577903929, 0.003490651415223739937 ) ) ;
#49342 = DIRECTION ( 'NONE',  ( 0.000000000000000000, 0.000000000000000000, 1.000000000000000000 ) ) ;
#49343 = ORIENTED_EDGE ( 'NONE', *, *, #9125, .T. ) ;
#49344 = DIRECTION ( 'NONE',  ( 0.000000000000000000, 0.000000000000000000, -1.000000000000000000 ) ) ;
#49345 = EDGE_LOOP ( 'NONE', ( #112301, #4628 ) ) ;
#49346 = ADVANCED_FACE ( 'NONE', ( #75035 ), #114669, .T. ) ;
#49348 = ORIENTED_EDGE ( 'NONE', *, *, #18456, .F. ) ;
#49347 = AXIS2_PLACEMENT_3D ( 'NONE', #47362, #87268, #127221 ) ;
#49349 = VERTEX_POINT ( 'NONE', #103203 ) ;
#49350 = CIRCLE ( 'NONE', #80730, 0.09999999999999982514 ) ;
#49351 = EDGE_CURVE ( 'NONE', #11954, #118880, #27214, .T. ) ;
#49352 = CARTESIAN_POINT ( 'NONE',  ( -13.09999999999999076, 2.500000000000000000, 4.776537180435972196 ) ) ;
#49353 = EDGE_LOOP ( 'NONE', ( #77562, #66023 ) ) ;
#49354 = VERTEX_POINT ( 'NONE', #37054 ) ;
#49355 = CARTESIAN_POINT ( 'NONE',  ( 6.899999999999928413, 12.50000000000000000, 3.983716857408420964 ) ) ;
#49356 = EDGE_CURVE ( 'NONE', #10762, #108113, #47783, .T. ) ;
#49357 = CARTESIAN_POINT ( 'NONE',  ( 13.14999999999990088, 2.500000000000000000, 2.511473670974873507 ) ) ;
#49358 = CARTESIAN_POINT ( 'NONE',  ( -2.950000000000030376, 12.50000000000000000, 6.495190528383297135 ) ) ;
#49359 = CARTESIAN_POINT ( 'NONE',  ( -10.60000000000000142, 12.50000000000000000, 3.983716857408420964 ) ) ;
#49360 = CARTESIAN_POINT ( 'NONE',  ( -10.85000000000000142, 2.500000000000000000, -7.188010851410850499 ) ) ;
#49361 = EDGE_LOOP ( 'NONE', ( #11164, #81998, #5625, #116468 ) ) ;
#49362 = DIRECTION ( 'NONE',  ( 0.000000000000000000, 0.000000000000000000, 1.000000000000000000 ) ) ;
#49363 = AXIS2_PLACEMENT_3D ( 'NONE', #23115, #74159, #83957 ) ;
#49364 = ORIENTED_EDGE ( 'NONE', *, *, #127886, .T. ) ;
#49365 = CARTESIAN_POINT ( 'NONE',  ( -1.450000000000035927, 12.50000000000000000, -1.753560074763288679 ) ) ;
#49366 = CIRCLE ( 'NONE', #93262, 0.1000000000000002554 ) ;
#49367 = VERTEX_POINT ( 'NONE', #18034 ) ;
#49368 = CARTESIAN_POINT ( 'NONE',  ( 112.9336158378006445, 8.661976086582759748, 0.8288528769330567592 ) ) ;
#49369 = DIRECTION ( 'NONE',  ( 0.000000000000000000, 0.000000000000000000, 1.000000000000000000 ) ) ;
#49370 = VECTOR ( 'NONE', #30724, 1000.000000000000000 ) ;
#49371 = ORIENTED_EDGE ( 'NONE', *, *, #28587, .T. ) ;
#49372 = DIRECTION ( 'NONE',  ( 0.000000000000000000, 0.000000000000000000, 1.000000000000000000 ) ) ;
#49373 = DIRECTION ( 'NONE',  ( 0.000000000000000000, 0.000000000000000000, 1.000000000000000000 ) ) ;
#49374 = ORIENTED_EDGE ( 'NONE', *, *, #80298, .T. ) ;
#49375 = DIRECTION ( 'NONE',  ( 0.000000000000000000, 0.000000000000000000, -1.000000000000000000 ) ) ;
#49376 = ORIENTED_EDGE ( 'NONE', *, *, #52657, .T. ) ;
#49377 = ORIENTED_EDGE ( 'NONE', *, *, #46421, .F. ) ;
#49378 = PLANE ( 'NONE',  #16234 ) ;
#49379 = DIRECTION ( 'NONE',  ( 0.000000000000000000, 1.000000000000000000, 0.000000000000000000 ) ) ;
#49380 = CARTESIAN_POINT ( 'NONE',  ( 185.0885416670080872, -6.551208109652273848, -3.782341765625003571 ) ) ;
#49381 = AXIS2_PLACEMENT_3D ( 'NONE', #124955, #25438, #5802 ) ;
#49382 = DIRECTION ( 'NONE',  ( 0.000000000000000000, 0.000000000000000000, 1.000000000000000000 ) ) ;
#49383 = LINE ( 'NONE', #81415, #39530 ) ;
#49384 = ORIENTED_EDGE ( 'NONE', *, *, #18401, .T. ) ;
#49385 = CIRCLE ( 'NONE', #53856, 0.1000000000000002554 ) ;
#49386 = CARTESIAN_POINT ( 'NONE',  ( 187.5000000000000000, 0.000000000000000000, 0.000000000000000000 ) ) ;
#49387 = AXIS2_PLACEMENT_3D ( 'NONE', #64100, #14964, #83745 ) ;
#49388 = AXIS2_PLACEMENT_3D ( 'NONE', #91767, #110753, #32872 ) ;
#49389 = ORIENTED_EDGE ( 'NONE', *, *, #90027, .T. ) ;
#49390 = DIRECTION ( 'NONE',  ( 0.000000000000000000, 1.000000000000000000, 0.000000000000000000 ) ) ;
#49391 = DIRECTION ( 'NONE',  ( -1.000000000000000000, -0.000000000000000000, -0.000000000000000000 ) ) ;
#49392 = CONICAL_SURFACE ( 'NONE', #3311, 0.1000000000000002554, 0.003490658503988666988 ) ;
#49393 = ADVANCED_FACE ( 'NONE', ( #8852 ), #45732, .T. ) ;
#49394 = DIRECTION ( 'NONE',  ( -0.000000000000000000, -1.000000000000000000, -0.000000000000000000 ) ) ;
#49395 = DIRECTION ( 'NONE',  ( 0.000000000000000000, 0.000000000000000000, 1.000000000000000000 ) ) ;
#49396 = CARTESIAN_POINT ( 'NONE',  ( 7.099999999999928590, 2.500000000000000000, 4.330127018922196314 ) ) ;
#49397 = EDGE_CURVE ( 'NONE', #71725, #2601, #16458, .T. ) ;
#49398 = DIRECTION ( 'NONE',  ( -0.000000000000000000, -1.000000000000000000, -0.000000000000000000 ) ) ;
#49399 = DIRECTION ( 'NONE',  ( 0.000000000000000000, -0.000000000000000000, 1.000000000000000000 ) ) ;
#49400 = EDGE_LOOP ( 'NONE', ( #108259, #48684 ) ) ;
#49401 = AXIS2_PLACEMENT_3D ( 'NONE', #124913, #7047, #7698 ) ;
#49402 = CARTESIAN_POINT ( 'NONE',  ( 184.4583333333333144, 4.445597072760201662, 7.699999999999855405 ) ) ;
#49404 = AXIS2_PLACEMENT_3D ( 'NONE', #115261, #67452, #106751 ) ;
#49403 = AXIS2_PLACEMENT_3D ( 'NONE', #60751, #119027, #20177 ) ;
#49405 = DIRECTION ( 'NONE',  ( 0.000000000000000000, 0.000000000000000000, 1.000000000000000000 ) ) ;
#49406 = EDGE_CURVE ( 'NONE', #119162, #50950, #5995, .T. ) ;
#49407 = ORIENTED_EDGE ( 'NONE', *, *, #68631, .F. ) ;
#49408 = DIRECTION ( 'NONE',  ( 0.000000000000000000, 1.000000000000000000, 0.000000000000000000 ) ) ;
#49409 = VERTEX_POINT ( 'NONE', #117498 ) ;
#49410 = ORIENTED_EDGE ( 'NONE', *, *, #92749, .T. ) ;
#49411 = DIRECTION ( 'NONE',  ( -0.000000000000000000, -1.000000000000000000, -0.000000000000000000 ) ) ;
#49412 = EDGE_LOOP ( 'NONE', ( #70532, #100273 ) ) ;
#49413 = DIRECTION ( 'NONE',  ( 0.000000000000000000, 0.000000000000000000, 1.000000000000000000 ) ) ;
#49414 = FACE_OUTER_BOUND ( 'NONE', #121774, .T. ) ;
#49415 = ORIENTED_EDGE ( 'NONE', *, *, #107631, .F. ) ;
#49416 = CARTESIAN_POINT ( 'NONE',  ( -1.900000000000034106, 2.500000000000000000, 0.2464101615137735679 ) ) ;
#49418 = ORIENTED_EDGE ( 'NONE', *, *, #28434, .F. ) ;
#49417 = FACE_OUTER_BOUND ( 'NONE', #118905, .T. ) ;
#49419 = DIRECTION ( 'NONE',  ( 0.000000000000000000, -0.000000000000000000, 1.000000000000000000 ) ) ;
#49420 = DIRECTION ( 'NONE',  ( 0.000000000000000000, 0.000000000000000000, 1.000000000000000000 ) ) ;
#49421 = VERTEX_POINT ( 'NONE', #16087 ) ;
#49422 = ADVANCED_FACE ( 'NONE', ( #98517 ), #79188, .T. ) ;
#49423 = AXIS2_PLACEMENT_3D ( 'NONE', #44635, #115270, #25620 ) ;
#49424 = VERTEX_POINT ( 'NONE', #116872 ) ;
#49425 = AXIS2_PLACEMENT_3D ( 'NONE', #82394, #61467, #21525 ) ;
#49426 = ORIENTED_EDGE ( 'NONE', *, *, #54930, .T. ) ;
#49427 = FACE_OUTER_BOUND ( 'NONE', #25255, .T. ) ;
#49428 = CARTESIAN_POINT ( 'NONE',  ( -5.000000000000024869, 12.50000000000000000, -5.022947341949754119 ) ) ;
#49429 = DIRECTION ( 'NONE',  ( -4.274815082592931898E-19, -0.9999939076577903929, -0.003490651415223739937 ) ) ;
#49430 = EDGE_CURVE ( 'NONE', #32296, #63903, #62464, .T. ) ;
#49431 = EDGE_CURVE ( 'NONE', #107157, #86066, #93938, .T. ) ;
#49432 = FACE_BOUND ( 'NONE', #53225, .T. ) ;
#49433 = VERTEX_POINT ( 'NONE', #96584 ) ;
#49434 = ADVANCED_FACE ( 'NONE', ( #88719 ), #6269, .T. ) ;
#49435 = EDGE_CURVE ( 'NONE', #83925, #44623, #56023, .T. ) ;
#49436 = CARTESIAN_POINT ( 'NONE',  ( -5.400000000000019895, 2.500000000000000000, 4.330127018922196314 ) ) ;
#49437 = DIRECTION ( 'NONE',  ( -0.000000000000000000, 1.000000000000000000, -0.000000000000000000 ) ) ;
#49438 = VERTEX_POINT ( 'NONE', #126718 ) ;
#49440 = CONICAL_SURFACE ( 'NONE', #66135, 0.1000000000000002554, 0.003490658503988666988 ) ;
#49439 = CONICAL_SURFACE ( 'NONE', #45323, 0.09999999999999982514, 0.003490658503988666988 ) ;
#49441 = CARTESIAN_POINT ( 'NONE',  ( -10.65000000000000391, 12.50000000000000000, -6.148780366869522673 ) ) ;
#49442 = CARTESIAN_POINT ( 'NONE',  ( 16.56576425165007649, 1.499999999999997113, 6.084390597445792359 ) ) ;
#49443 = ADVANCED_FACE ( 'NONE', ( #27868 ), #73006, .T. ) ;
#49444 = CARTESIAN_POINT ( 'NONE',  ( 10.64999999999991331, 2.500000000000000000, -1.718653347947325827 ) ) ;
#49445 = DIRECTION ( 'NONE',  ( 0.000000000000000000, -0.000000000000000000, 1.000000000000000000 ) ) ;
#49446 = CARTESIAN_POINT ( 'NONE',  ( 12.04999999999990834, 2.500000000000000000, -2.265063509461101798 ) ) ;
#49447 = EDGE_CURVE ( 'NONE', #13831, #122621, #121030, .T. ) ;
#49448 = DIRECTION ( 'NONE',  ( 0.000000000000000000, -0.000000000000000000, 1.000000000000000000 ) ) ;
#49449 = PLANE ( 'NONE',  #110971 ) ;
#49451 = CIRCLE ( 'NONE', #78695, 0.06509327318403745899 ) ;
#49450 = VECTOR ( 'NONE', #93801, 1000.000000000000000 ) ;
#49452 = CIRCLE ( 'NONE', #30675, 0.09999999999999982514 ) ;
#49453 = EDGE_CURVE ( 'NONE', #41372, #27226, #110656, .T. ) ;
#49454 = ORIENTED_EDGE ( 'NONE', *, *, #59969, .F. ) ;
#49455 = VERTEX_POINT ( 'NONE', #108352 ) ;
#49456 = ORIENTED_EDGE ( 'NONE', *, *, #102783, .T. ) ;
#49457 = VERTEX_POINT ( 'NONE', #38346 ) ;
#49458 = VERTEX_POINT ( 'NONE', #78277 ) ;
#49459 = CARTESIAN_POINT ( 'NONE',  ( -1.700000000000034817, 12.50000000000000000, -0.06509327318403980434 ) ) ;
#49460 = DIRECTION ( 'NONE',  ( 0.000000000000000000, 0.000000000000000000, 1.000000000000000000 ) ) ;
#49461 = ORIENTED_EDGE ( 'NONE', *, *, #105912, .T. ) ;
#49462 = EDGE_CURVE ( 'NONE', #20554, #41081, #12357, .T. ) ;
#49463 = FACE_BOUND ( 'NONE', #29452, .T. ) ;
#49464 = EDGE_CURVE ( 'NONE', #32613, #52515, #70946, .T. ) ;
#49465 = CARTESIAN_POINT ( 'NONE',  ( 6.649999999999928413, 2.500000000000000000, 1.572243186433545548 ) ) ;
#49466 = DIRECTION ( 'NONE',  ( -0.000000000000000000, -1.000000000000000000, -0.000000000000000000 ) ) ;
#49467 = CARTESIAN_POINT ( 'NONE',  ( 3.099999999999945466, 12.50000000000000000, -3.983716857408426293 ) ) ;
#49468 = FACE_OUTER_BOUND ( 'NONE', #3592, .T. ) ;
#49469 = DIRECTION ( 'NONE',  ( 0.000000000000000000, 1.000000000000000000, 0.000000000000000000 ) ) ;
#49470 = CARTESIAN_POINT ( 'NONE',  ( 1.049999999999954525, 12.50000000000000000, 1.818653347947321475 ) ) ;
#49472 = EDGE_LOOP ( 'NONE', ( #102431, #94586, #119839, #33036 ) ) ;
#49471 = CIRCLE ( 'NONE', #89154, 0.1000000000000000472 ) ;
#49473 = ORIENTED_EDGE ( 'NONE', *, *, #31854, .T. ) ;
#49474 = AXIS2_PLACEMENT_3D ( 'NONE', #69028, #70332, #38974 ) ;
#49475 = ORIENTED_EDGE ( 'NONE', *, *, #63034, .T. ) ;
#49476 = EDGE_LOOP ( 'NONE', ( #63425, #89381 ) ) ;
#49477 = CARTESIAN_POINT ( 'NONE',  ( 11.75764115802644660, 2.500000000000000000, 7.679135278744413817 ) ) ;
#49478 = CONICAL_SURFACE ( 'NONE', #122623, 0.09999999999999999167, 0.003490658503988666988 ) ;
#49479 = CARTESIAN_POINT ( 'NONE',  ( 17.50000000000000000, -2.500000000000000000, -3.999999999999998224 ) ) ;
#49480 = EDGE_LOOP ( 'NONE', ( #75606, #35477, #62674, #86650 ) ) ;
#49481 = CARTESIAN_POINT ( 'NONE',  ( 7.299999999999927880, 2.500000000000000000, 3.883716857408421319 ) ) ;
#49482 = AXIS2_PLACEMENT_3D ( 'NONE', #75339, #55067, #88200 ) ;
#49483 = AXIS2_PLACEMENT_3D ( 'NONE', #94334, #45256, #64240 ) ;
#49484 = CARTESIAN_POINT ( 'NONE',  ( -9.800000000000006040, 2.500000000000000000, 4.576537180435972019 ) ) ;
#49485 = CIRCLE ( 'NONE', #122628, 0.1000000000000000472 ) ;
#49486 = DIRECTION ( 'NONE',  ( 0.000000000000000000, 0.000000000000000000, 1.000000000000000000 ) ) ;
#49487 = CARTESIAN_POINT ( 'NONE',  ( 183.8593750003413732, 0.000000000000000000, 7.564683531250000925 ) ) ;
#49488 = CARTESIAN_POINT ( 'NONE',  ( 6.449999999999933564, 2.500000000000000000, -6.741600689897078169 ) ) ;
#49489 = FACE_OUTER_BOUND ( 'NONE', #25623, .T. ) ;
#49490 = PLANE ( 'NONE',  #68442 ) ;
#49491 = ORIENTED_EDGE ( 'NONE', *, *, #63612, .F. ) ;
#49492 = DIRECTION ( 'NONE',  ( -0.000000000000000000, 1.000000000000000000, -0.000000000000000000 ) ) ;
#49493 = AXIS2_PLACEMENT_3D ( 'NONE', #88850, #31235, #85300 ) ;
#49494 = EDGE_LOOP ( 'NONE', ( #45953, #77295 ) ) ;
#49495 = EDGE_CURVE ( 'NONE', #18199, #1500, #16542, .T. ) ;
#49497 = AXIS2_PLACEMENT_3D ( 'NONE', #109991, #58326, #129012 ) ;
#49496 = CIRCLE ( 'NONE', #91329, 0.09999999999999982514 ) ;
#49498 = VERTEX_POINT ( 'NONE', #86775 ) ;
#49499 = PLANE ( 'NONE',  #71965 ) ;
#49500 = EDGE_CURVE ( 'NONE', #101537, #53806, #52086, .T. ) ;
#49501 = CARTESIAN_POINT ( 'NONE',  ( -7.700000000000014388, 2.500000000000000000, -4.676537180435977881 ) ) ;
#49502 = DIRECTION ( 'NONE',  ( 0.000000000000000000, 1.000000000000000000, 0.000000000000000000 ) ) ;
#49503 = EDGE_LOOP ( 'NONE', ( #115595, #104295 ) ) ;
#49504 = ORIENTED_EDGE ( 'NONE', *, *, #64210, .T. ) ;
#49505 = LINE ( 'NONE', #29846, #5805 ) ;
#49506 = DIRECTION ( 'NONE',  ( -4.274815082592931898E-19, -0.9999939076577903929, -0.003490651415223739937 ) ) ;
#49507 = CARTESIAN_POINT ( 'NONE',  ( 2.099999999999948574, 12.50000000000000000, 3.572213422710607489 ) ) ;
#49508 = ORIENTED_EDGE ( 'NONE', *, *, #89171, .T. ) ;
#49509 = CARTESIAN_POINT ( 'NONE',  ( 6.449999999999928235, 12.50000000000000000, 2.446380397790835826 ) ) ;
#49510 = EDGE_LOOP ( 'NONE', ( #110638, #106823, #37989, #97161 ) ) ;
#49511 = CARTESIAN_POINT ( 'NONE',  ( 2.099999999999950351, 12.50000000000000000, -0.6928203230275541413 ) ) ;
#49512 = ORIENTED_EDGE ( 'NONE', *, *, #37021, .T. ) ;
#49513 = CARTESIAN_POINT ( 'NONE',  ( -1.700000000000034817, 2.500000000000000000, -2.385244779468109755E-15 ) ) ;
#49514 = LINE ( 'NONE', #40990, #102756 ) ;
#49515 = DIRECTION ( 'NONE',  ( 0.000000000000000000, -0.000000000000000000, 1.000000000000000000 ) ) ;
#49516 = CARTESIAN_POINT ( 'NONE',  ( -4.150000000000027889, 12.50000000000000000, -7.188010851410854052 ) ) ;
#49517 = ORIENTED_EDGE ( 'NONE', *, *, #35268, .F. ) ;
#49518 = FACE_OUTER_BOUND ( 'NONE', #86267, .T. ) ;
#49519 = AXIS2_PLACEMENT_3D ( 'NONE', #86723, #74489, #124239 ) ;
#49520 = ORIENTED_EDGE ( 'NONE', *, *, #28007, .F. ) ;
#49521 = EDGE_LOOP ( 'NONE', ( #103823, #34540 ) ) ;
#49522 = CARTESIAN_POINT ( 'NONE',  ( -0.4500000000000397571, 12.50000000000000000, -2.165063509461101710 ) ) ;
#49523 = CARTESIAN_POINT ( 'NONE',  ( 15.19999999999989093, 2.500000000000000000, 0.3464101615137735735 ) ) ;
#49524 = CARTESIAN_POINT ( 'NONE',  ( 18.09027855933934603, 2.526462839860887488, 2.685672775344559504 ) ) ;
#49525 = LINE ( 'NONE', #31182, #31258 ) ;
#49526 = DIRECTION ( 'NONE',  ( 0.000000000000000000, 0.000000000000000000, 1.000000000000000000 ) ) ;
#49529 = VECTOR ( 'NONE', #82607, 1000.000000000000000 ) ;
#49528 = DIRECTION ( 'NONE',  ( -0.000000000000000000, -1.000000000000000000, -0.000000000000000000 ) ) ;
#49527 = VECTOR ( 'NONE', #7189, 1000.000000000000000 ) ;
#49530 = EDGE_CURVE ( 'NONE', #22326, #22783, #24886, .T. ) ;
#49531 = CARTESIAN_POINT ( 'NONE',  ( -5.400000000000019895, 2.500000000000000000, 3.637306695894644726 ) ) ;
#49532 = DIRECTION ( 'NONE',  ( -4.274815082592931898E-19, -0.9999939076577903929, -0.003490651415223739937 ) ) ;
#49533 = DIRECTION ( 'NONE',  ( 0.000000000000000000, 1.000000000000000000, 0.000000000000000000 ) ) ;
#49534 = CIRCLE ( 'NONE', #128964, 0.06509327318403745899 ) ;
#49536 = CONICAL_SURFACE ( 'NONE', #51593, 0.1000000000000002554, 0.003490658503988666988 ) ;
#49535 = CIRCLE ( 'NONE', #18116, 0.06509327318403745899 ) ;
#49537 = EDGE_CURVE ( 'NONE', #29893, #29014, #69727, .T. ) ;
#49538 = CIRCLE ( 'NONE', #101757, 0.1000000000000000472 ) ;
#49539 = ORIENTED_EDGE ( 'NONE', *, *, #36254, .F. ) ;
#49540 = PLANE ( 'NONE',  #106935 ) ;
#49541 = EDGE_CURVE ( 'NONE', #80196, #92392, #313, .T. ) ;
#49542 = CARTESIAN_POINT ( 'NONE',  ( -11.64999999999999680, 2.500000000000000000, 2.265063509461097357 ) ) ;
#49544 = ADVANCED_FACE ( 'NONE', ( #128681 ), #47888, .T. ) ;
#49543 = FACE_OUTER_BOUND ( 'NONE', #129427, .T. ) ;
#49545 = PLANE ( 'NONE',  #71519 ) ;
#49546 = DIRECTION ( 'NONE',  ( -0.000000000000000000, -1.000000000000000000, -0.000000000000000000 ) ) ;
#49547 = ORIENTED_EDGE ( 'NONE', *, *, #74992, .T. ) ;
#49548 = CARTESIAN_POINT ( 'NONE',  ( -0.2000000000000399791, 2.500000000000000000, -4.676537180435977881 ) ) ;
#49549 = CARTESIAN_POINT ( 'NONE',  ( 12.29999999999990656, 12.50000000000000000, -4.676537180435977881 ) ) ;
#49551 = ORIENTED_EDGE ( 'NONE', *, *, #60657, .T. ) ;
#49550 = LINE ( 'NONE', #118919, #4523 ) ;
#49552 = EDGE_CURVE ( 'NONE', #24359, #115574, #127299, .T. ) ;
#49553 = CIRCLE ( 'NONE', #41159, 0.06509327318403745899 ) ;
#49554 = CIRCLE ( 'NONE', #41242, 0.06509327318403743123 ) ;
#49555 = EDGE_LOOP ( 'NONE', ( #124644, #62224, #49212, #104317 ) ) ;
#49556 = CONICAL_SURFACE ( 'NONE', #30782, 0.1000000000000002554, 0.003490658503988666988 ) ;
#49557 = CARTESIAN_POINT ( 'NONE',  ( 1.049999999999954969, 2.500000000000000000, -6.741600689897077281 ) ) ;
#49558 = CIRCLE ( 'NONE', #72549, 0.1000000000000002554 ) ;
#49559 = EDGE_LOOP ( 'NONE', ( #110531, #67326, #81021, #66876 ) ) ;
#49560 = ORIENTED_EDGE ( 'NONE', *, *, #86041, .F. ) ;
#49561 = ORIENTED_EDGE ( 'NONE', *, *, #74581, .F. ) ;
#49562 = DIRECTION ( 'NONE',  ( -4.274815082592931898E-19, -0.9999939076577903929, -0.003490651415223739937 ) ) ;
#49563 = CARTESIAN_POINT ( 'NONE',  ( 14.34999999999989662, 2.500000000000000000, 2.511473670974873507 ) ) ;
#49564 = FACE_OUTER_BOUND ( 'NONE', #35427, .T. ) ;
#49565 = AXIS2_PLACEMENT_3D ( 'NONE', #52180, #92090, #12870 ) ;
#49566 = DIRECTION ( 'NONE',  ( -4.274815082592931898E-19, -0.9999939076577903929, -0.003490651415223739937 ) ) ;
#49567 = ORIENTED_EDGE ( 'NONE', *, *, #9383, .F. ) ;
#49568 = VECTOR ( 'NONE', #61631, 1000.000000000000000 ) ;
#49569 = CARTESIAN_POINT ( 'NONE',  ( 184.5416666666666572, -4.445597072760039126, 7.700000000000142286 ) ) ;
#49570 = EDGE_LOOP ( 'NONE', ( #23610, #90687, #31176, #89184 ) ) ;
#49571 = CARTESIAN_POINT ( 'NONE',  ( -0.6500000000000398792, 12.50000000000000000, -6.841600689897078702 ) ) ;
#49572 = CARTESIAN_POINT ( 'NONE',  ( 15.24415751722802526, 2.474878586408650438, 4.460068884075454321 ) ) ;
#49573 = CARTESIAN_POINT ( 'NONE',  ( 7.299999999999926104, 12.50000000000000000, -0.2813168883297408329 ) ) ;
#49574 = CONICAL_SURFACE ( 'NONE', #80872, 0.1000000000000002554, 0.003490658503988666988 ) ;
#49575 = CARTESIAN_POINT ( 'NONE',  ( 1.049999999999954525, 12.50000000000000000, 1.818653347947321475 ) ) ;
#49576 = CIRCLE ( 'NONE', #45374, 0.06509327318403745899 ) ;
#49577 = ORIENTED_EDGE ( 'NONE', *, *, #95664, .T. ) ;
#49578 = EDGE_CURVE ( 'NONE', #100057, #79205, #102255, .T. ) ;
#49580 = AXIS2_PLACEMENT_3D ( 'NONE', #45767, #65385, #126900 ) ;
#49579 = AXIS2_PLACEMENT_3D ( 'NONE', #10813, #110960, #43549 ) ;
#49581 = ORIENTED_EDGE ( 'NONE', *, *, #123623, .T. ) ;
#49582 = ORIENTED_EDGE ( 'NONE', *, *, #5483, .F. ) ;
#49583 = VERTEX_POINT ( 'NONE', #61197 ) ;
#49584 = VERTEX_POINT ( 'NONE', #39651 ) ;
#49585 = CARTESIAN_POINT ( 'NONE',  ( -10.20000000000000462, 2.500000000000000000, -4.676537180435973440 ) ) ;
#49586 = DIRECTION ( 'NONE',  ( -0.000000000000000000, 1.000000000000000000, -0.000000000000000000 ) ) ;
#49587 = FACE_OUTER_BOUND ( 'NONE', #64968, .T. ) ;
#49588 = EDGE_CURVE ( 'NONE', #42202, #10139, #20635, .T. ) ;
#49589 = FACE_BOUND ( 'NONE', #35880, .T. ) ;
#49590 = DIRECTION ( 'NONE',  ( -0.000000000000000000, -1.000000000000000000, -0.000000000000000000 ) ) ;
#49591 = CARTESIAN_POINT ( 'NONE',  ( 187.1562500006828316, 8.891194145520236347, 5.444286225454521982E-16 ) ) ;
#49592 = EDGE_CURVE ( 'NONE', #120278, #125645, #29174, .T. ) ;
#49593 = LINE ( 'NONE', #47649, #76128 ) ;
#49594 = DIRECTION ( 'NONE',  ( 0.000000000000000000, 0.000000000000000000, 1.000000000000000000 ) ) ;
#49595 = ADVANCED_FACE ( 'NONE', ( #19988 ), #41640, .T. ) ;
#49596 = DIRECTION ( 'NONE',  ( 0.000000000000000000, 0.000000000000000000, 1.000000000000000000 ) ) ;
#49597 = EDGE_CURVE ( 'NONE', #58191, #97339, #110920, .T. ) ;
#49598 = DIRECTION ( 'NONE',  ( -0.000000000000000000, 1.000000000000000000, -0.000000000000000000 ) ) ;
#49599 = EDGE_CURVE ( 'NONE', #74569, #66767, #91782, .T. ) ;
#49600 = AXIS2_PLACEMENT_3D ( 'NONE', #22118, #52199, #79095 ) ;
#49601 = LINE ( 'NONE', #8353, #24060 ) ;
#49602 = ADVANCED_FACE ( 'NONE', ( #108982 ), #1892, .T. ) ;
#49603 = DIRECTION ( 'NONE',  ( -0.000000000000000000, 1.000000000000000000, -0.000000000000000000 ) ) ;
#49604 = EDGE_CURVE ( 'NONE', #119959, #88710, #125236, .T. ) ;
#49605 = EDGE_LOOP ( 'NONE', ( #51281, #25938 ) ) ;
#49606 = ORIENTED_EDGE ( 'NONE', *, *, #87238, .T. ) ;
#49607 = VERTEX_POINT ( 'NONE', #49465 ) ;
#49608 = ORIENTED_EDGE ( 'NONE', *, *, #8614, .F. ) ;
#49609 = CARTESIAN_POINT ( 'NONE',  ( 2.099999999999950351, 2.500000000000000000, -4.430127018922202176 ) ) ;
#49610 = PLANE ( 'NONE',  #109293 ) ;
#49611 = FACE_BOUND ( 'NONE', #47177, .T. ) ;
#49612 = EDGE_CURVE ( 'NONE', #116018, #118459, #4032, .T. ) ;
#49613 = DIRECTION ( 'NONE',  ( -0.000000000000000000, -1.000000000000000000, -0.000000000000000000 ) ) ;
#49614 = AXIS2_PLACEMENT_3D ( 'NONE', #1808, #50934, #10968 ) ;
#49615 = VECTOR ( 'NONE', #60507, 1000.000000000000000 ) ;
#49616 = ORIENTED_EDGE ( 'NONE', *, *, #63284, .F. ) ;
#49617 = LINE ( 'NONE', #71823, #74006 ) ;
#49618 = DIRECTION ( 'NONE',  ( -4.274815082592931898E-19, -0.9999939076577903929, -0.003490651415223739937 ) ) ;
#49619 = CARTESIAN_POINT ( 'NONE',  ( 13.34999999999989662, 2.500000000000000000, -2.065063509461102065 ) ) ;
#49620 = FACE_OUTER_BOUND ( 'NONE', #43629, .T. ) ;
#49621 = ORIENTED_EDGE ( 'NONE', *, *, #98739, .F. ) ;
#49622 = DIRECTION ( 'NONE',  ( 0.000000000000000000, 0.000000000000000000, -1.000000000000000000 ) ) ;
#49623 = CIRCLE ( 'NONE', #53803, 0.1000000000000002554 ) ;
#49624 = VECTOR ( 'NONE', #12598, 1000.000000000000000 ) ;
#49625 = ORIENTED_EDGE ( 'NONE', *, *, #13084, .F. ) ;
#49626 = EDGE_LOOP ( 'NONE', ( #37446, #85560 ) ) ;
#49627 = CARTESIAN_POINT ( 'NONE',  ( 10.79999999999991012, 2.500000000000000000, 4.430127018922196847 ) ) ;
#49628 = DIRECTION ( 'NONE',  ( -0.000000000000000000, 1.000000000000000000, -0.000000000000000000 ) ) ;
#49629 = EDGE_LOOP ( 'NONE', ( #125150, #33913, #88769, #37746 ) ) ;
#49631 = CONICAL_SURFACE ( 'NONE', #95585, 0.1000000000000002554, 0.003490658503988666988 ) ;
#49630 = CIRCLE ( 'NONE', #66326, 2.750000000000002665 ) ;
#49632 = CIRCLE ( 'NONE', #85208, 0.09999999999999982514 ) ;
#49633 = CARTESIAN_POINT ( 'NONE',  ( -6.250000000000019540, 2.500000000000000000, -7.288010851410854585 ) ) ;
#49634 = DIRECTION ( 'NONE',  ( -4.274815082592931898E-19, -0.9999939076577903929, -0.003490651415223739937 ) ) ;
#49635 = ORIENTED_EDGE ( 'NONE', *, *, #75707, .F. ) ;
#49636 = DIRECTION ( 'NONE',  ( 0.000000000000000000, 0.000000000000000000, 1.000000000000000000 ) ) ;
#49637 = VERTEX_POINT ( 'NONE', #29803 ) ;
#49638 = CARTESIAN_POINT ( 'NONE',  ( -6.850000000000013856, 2.500000000000000000, 2.611473670974873151 ) ) ;
#49639 = VERTEX_POINT ( 'NONE', #99844 ) ;
#49640 = CARTESIAN_POINT ( 'NONE',  ( 186.6562500006828031, 8.891194145520236347, 5.444286225454521982E-16 ) ) ;
#49641 = FACE_BOUND ( 'NONE', #19905, .T. ) ;
#49642 = CIRCLE ( 'NONE', #83368, 0.1000000000000002554 ) ;
#49643 = ORIENTED_EDGE ( 'NONE', *, *, #47499, .F. ) ;
#49644 = EDGE_CURVE ( 'NONE', #125681, #33832, #18619, .T. ) ;
#49645 = CARTESIAN_POINT ( 'NONE',  ( 108.3415395100210503, 5.863329682499133888, 4.991179557506976394 ) ) ;
#49646 = ORIENTED_EDGE ( 'NONE', *, *, #40239, .F. ) ;
#49647 = DIRECTION ( 'NONE',  ( 0.000000000000000000, 0.000000000000000000, 1.000000000000000000 ) ) ;
#49648 = DIRECTION ( 'NONE',  ( -4.274815082592931898E-19, -0.9999939076577903929, -0.003490651415223739937 ) ) ;
#49649 = DIRECTION ( 'NONE',  ( -0.000000000000000000, 1.000000000000000000, -0.000000000000000000 ) ) ;
#49650 = DIRECTION ( 'NONE',  ( 0.000000000000000000, 1.000000000000000000, 0.000000000000000000 ) ) ;
#49652 = AXIS2_PLACEMENT_3D ( 'NONE', #47059, #37244, #54289 ) ;
#49651 = PLANE ( 'NONE',  #66307 ) ;
#49653 = ORIENTED_EDGE ( 'NONE', *, *, #51023, .F. ) ;
#49654 = ORIENTED_EDGE ( 'NONE', *, *, #43202, .F. ) ;
#49655 = ADVANCED_FACE ( 'NONE', ( #31109 ), #10162, .T. ) ;
#49656 = ORIENTED_EDGE ( 'NONE', *, *, #41052, .T. ) ;
#49657 = CARTESIAN_POINT ( 'NONE',  ( 4.149999999999939959, 2.500000000000000000, -6.495190528383302464 ) ) ;
#49658 = AXIS2_PLACEMENT_3D ( 'NONE', #80138, #120060, #62441 ) ;
#49659 = CARTESIAN_POINT ( 'NONE',  ( -2.700000000000030820, 2.500000000000000000, 0.4464101615137735513 ) ) ;
#49660 = DIRECTION ( 'NONE',  ( 0.000000000000000000, 0.000000000000000000, 1.000000000000000000 ) ) ;
#49662 = EDGE_LOOP ( 'NONE', ( #99726, #111475, #1182, #121593 ) ) ;
#49661 = VERTEX_POINT ( 'NONE', #81484 ) ;
#49663 = ORIENTED_EDGE ( 'NONE', *, *, #52950, .F. ) ;
#49664 = CARTESIAN_POINT ( 'NONE',  ( -11.05000000000000071, 2.500000000000000000, -6.941600689897075682 ) ) ;
#49665 = CONICAL_SURFACE ( 'NONE', #53749, 0.1000000000000002554, 0.003490658503988666988 ) ;
#49666 = CIRCLE ( 'NONE', #53751, 0.1000000000000002554 ) ;
#49667 = DIRECTION ( 'NONE',  ( 0.000000000000000000, 0.000000000000000000, 1.000000000000000000 ) ) ;
#49668 = AXIS2_PLACEMENT_3D ( 'NONE', #54336, #55624, #64791 ) ;
#49669 = CONICAL_SURFACE ( 'NONE', #57968, 0.09999999999999999167, 0.003490658503988666988 ) ;
#49670 = ITEM_DEFINED_TRANSFORMATION ( 'NONE', 'NONE', #75552,  #108296 ) ;
#49671 = DIRECTION ( 'NONE',  ( 0.000000000000000000, -0.9999939076577903929, 0.003490651415223739937 ) ) ;
#49672 = DIRECTION ( 'NONE',  ( 0.000000000000000000, 1.000000000000000000, 0.000000000000000000 ) ) ;
#49673 = CARTESIAN_POINT ( 'NONE',  ( -0.2000000000000347888, 2.500000000000000000, 0.3464101615137758494 ) ) ;
#49674 = CARTESIAN_POINT ( 'NONE',  ( 13.94999999999989448, 2.500000000000000000, -2.611473670974877592 ) ) ;
#49675 = LINE ( 'NONE', #58203, #117790 ) ;
#49676 = AXIS2_PLACEMENT_3D ( 'NONE', #100032, #58187, #98719 ) ;
#49677 = CARTESIAN_POINT ( 'NONE',  ( -4.800000000000026468, 2.500000000000000000, -4.576537180435978236 ) ) ;
#49678 = ORIENTED_EDGE ( 'NONE', *, *, #58002, .T. ) ;
#49679 = ORIENTED_EDGE ( 'NONE', *, *, #81655, .F. ) ;
#49680 = CARTESIAN_POINT ( 'NONE',  ( -1.850000000000033396, 12.50000000000000000, -6.841600689897077814 ) ) ;
#49682 = CIRCLE ( 'NONE', #1529, 0.06509327318403745899 ) ;
#49681 = VECTOR ( 'NONE', #35648, 1000.000000000000000 ) ;
#49683 = CARTESIAN_POINT ( 'NONE',  ( 10.39999999999991509, 2.500000000000000000, 0.5928203230275495006 ) ) ;
#49684 = EDGE_LOOP ( 'NONE', ( #101744, #28834 ) ) ;
#49685 = ORIENTED_EDGE ( 'NONE', *, *, #127482, .T. ) ;
#49686 = CARTESIAN_POINT ( 'NONE',  ( 14.14999999999989733, 12.50000000000000000, 2.792790559304612064 ) ) ;
#49687 = DIRECTION ( 'NONE',  ( -0.000000000000000000, -1.000000000000000000, -0.000000000000000000 ) ) ;
#49688 = CARTESIAN_POINT ( 'NONE',  ( -2.100000000000034284, 2.500000000000000000, 0.09999999999999761857 ) ) ;
#49689 = DIRECTION ( 'NONE',  ( -0.000000000000000000, 1.000000000000000000, -0.000000000000000000 ) ) ;
#49690 = EDGE_CURVE ( 'NONE', #41939, #55594, #85522, .T. ) ;
#49691 = LINE ( 'NONE', #39872, #53257 ) ;
#49692 = CARTESIAN_POINT ( 'NONE',  ( -9.550000000000006040, 12.50000000000000000, 2.165063509461097713 ) ) ;
#49693 = DIRECTION ( 'NONE',  ( 0.000000000000000000, 0.000000000000000000, -1.000000000000000000 ) ) ;
#49694 = VECTOR ( 'NONE', #5158, 1000.000000000000000 ) ;
#49695 = LINE ( 'NONE', #59528, #43719 ) ;
#49696 = EDGE_CURVE ( 'NONE', #81742, #88394, #82786, .T. ) ;
#49697 = ORIENTED_EDGE ( 'NONE', *, *, #116381, .F. ) ;
#49698 = ORIENTED_EDGE ( 'NONE', *, *, #89643, .F. ) ;
#49699 = ADVANCED_FACE ( 'NONE', ( #3561 ), #114165, .T. ) ;
#49700 = ORIENTED_EDGE ( 'NONE', *, *, #73844, .F. ) ;
#49701 = ORIENTED_EDGE ( 'NONE', *, *, #93672, .F. ) ;
#49702 = ADVANCED_FACE ( 'NONE', ( #13375 ), #89730, .T. ) ;
#49703 = DIRECTION ( 'NONE',  ( 0.000000000000000000, -0.000000000000000000, 1.000000000000000000 ) ) ;
#49704 = DIRECTION ( 'NONE',  ( 0.000000000000000000, 0.000000000000000000, -1.000000000000000000 ) ) ;
#49705 = ORIENTED_EDGE ( 'NONE', *, *, #71297, .F. ) ;
#49706 = VECTOR ( 'NONE', #8725, 1000.000000000000000 ) ;
#49707 = DIRECTION ( 'NONE',  ( 0.000000000000000000, 0.000000000000000000, 1.000000000000000000 ) ) ;
#49709 = CARTESIAN_POINT ( 'NONE',  ( 186.0729166673494603, 4.445597072760091528, -7.700000000000049916 ) ) ;
#49708 = AXIS2_PLACEMENT_3D ( 'NONE', #31053, #61133, #91882 ) ;
#49710 = ADVANCED_FACE ( 'NONE', ( #112233 ), #56271, .T. ) ;
#49711 = DIRECTION ( 'NONE',  ( 0.000000000000000000, -1.000000000000000000, -0.000000000000000000 ) ) ;
#49713 = EDGE_LOOP ( 'NONE', ( #111226, #120189 ) ) ;
#49712 = CARTESIAN_POINT ( 'NONE',  ( -11.05000000000000071, 2.500000000000000000, 2.411473670974873862 ) ) ;
#49714 = ADVANCED_FACE ( 'NONE', ( #42875 ), #43781, .T. ) ;
#49715 = CARTESIAN_POINT ( 'NONE',  ( 0.6499999999999561684, 2.500000000000000000, -1.718653347947325827 ) ) ;
#49716 = AXIS2_PLACEMENT_3D ( 'NONE', #12460, #129216, #62862 ) ;
#49717 = DIRECTION ( 'NONE',  ( 0.000000000000000000, 1.000000000000000000, 0.000000000000000000 ) ) ;
#49718 = VERTEX_POINT ( 'NONE', #32411 ) ;
#49719 = CONICAL_SURFACE ( 'NONE', #95672, 0.1000000000000002554, 0.003490658503988666988 ) ;
#49720 = AXIS2_PLACEMENT_3D ( 'NONE', #58502, #8705, #100978 ) ;
#49721 = ORIENTED_EDGE ( 'NONE', *, *, #74503, .T. ) ;
#49722 = ORIENTED_EDGE ( 'NONE', *, *, #125528, .F. ) ;
#49723 = VERTEX_POINT ( 'NONE', #33671 ) ;
#49724 = CARTESIAN_POINT ( 'NONE',  ( -13.94999999999998685, 12.50000000000000000, -2.511473670974875727 ) ) ;
#49725 = DIRECTION ( 'NONE',  ( 0.000000000000000000, 0.000000000000000000, 1.000000000000000000 ) ) ;
#49726 = FACE_OUTER_BOUND ( 'NONE', #62051, .T. ) ;
#49727 = AXIS2_PLACEMENT_3D ( 'NONE', #99527, #39331, #49785 ) ;
#49728 = ORIENTED_EDGE ( 'NONE', *, *, #47388, .F. ) ;
#49729 = AXIS2_PLACEMENT_3D ( 'NONE', #118736, #79477, #10078 ) ;
#49730 = CARTESIAN_POINT ( 'NONE',  ( 108.0000000000000142, 9.000000000000001776, 0.000000000000000000 ) ) ;
#49731 = DIRECTION ( 'NONE',  ( -0.000000000000000000, 1.000000000000000000, -0.000000000000000000 ) ) ;
#49732 = CARTESIAN_POINT ( 'NONE',  ( 5.399999999999933742, 2.500000000000000000, 0.09999999999999761857 ) ) ;
#49733 = CARTESIAN_POINT ( 'NONE',  ( -14.99999999999994671, 2.500000000000000000, 0.000000000000000000 ) ) ;
#49734 = EDGE_LOOP ( 'NONE', ( #103242, #73821, #113415, #51794 ) ) ;
#49735 = CIRCLE ( 'NONE', #1677, 0.06509327318403745899 ) ;
#49736 = DIRECTION ( 'NONE',  ( -0.000000000000000000, 1.000000000000000000, -0.000000000000000000 ) ) ;
#49737 = AXIS2_PLACEMENT_3D ( 'NONE', #66368, #106296, #56541 ) ;
#49738 = ORIENTED_EDGE ( 'NONE', *, *, #11726, .F. ) ;
#49739 = EDGE_LOOP ( 'NONE', ( #8918, #114856 ) ) ;
#49740 = DIRECTION ( 'NONE',  ( 0.000000000000000000, 1.000000000000000000, 0.000000000000000000 ) ) ;
#49741 = DIRECTION ( 'NONE',  ( -4.274815082592931898E-19, -0.9999939076577903929, -0.003490651415223739937 ) ) ;
#49742 = FACE_BOUND ( 'NONE', #73172, .T. ) ;
#49743 = VECTOR ( 'NONE', #20510, 1000.000000000000000 ) ;
#49744 = DIRECTION ( 'NONE',  ( 0.000000000000000000, -0.9999939076577903929, 0.003490651415223739937 ) ) ;
#49745 = CARTESIAN_POINT ( 'NONE',  ( 8.099999999999923261, 2.500000000000000000, -3.883716857408426648 ) ) ;
#49746 = AXIS2_PLACEMENT_3D ( 'NONE', #62216, #11152, #51108 ) ;
#49747 = FACE_OUTER_BOUND ( 'NONE', #7886, .T. ) ;
#49748 = CIRCLE ( 'NONE', #35172, 0.06509327318403745899 ) ;
#49749 = EDGE_CURVE ( 'NONE', #79243, #22283, #54576, .T. ) ;
#49750 = EDGE_LOOP ( 'NONE', ( #99341, #126650, #48734, #60320 ) ) ;
#49751 = EDGE_CURVE ( 'NONE', #80732, #114635, #12447, .T. ) ;
#49752 = PLANE ( 'NONE',  #67241 ) ;
#49753 = CARTESIAN_POINT ( 'NONE',  ( -11.89999999999999503, 2.500000000000000000, 3.983716857408420076 ) ) ;
#49754 = CARTESIAN_POINT ( 'NONE',  ( -8.950000000000009948, 2.500000000000000000, -1.918653347947326004 ) ) ;
#49755 = ADVANCED_FACE ( 'NONE', ( #15289 ), #25128, .T. ) ;
#49757 = LINE ( 'NONE', #90950, #23963 ) ;
#49756 = AXIS2_PLACEMENT_3D ( 'NONE', #59291, #50738, #69077 ) ;
#49758 = ORIENTED_EDGE ( 'NONE', *, *, #21592, .F. ) ;
#49759 = EDGE_CURVE ( 'NONE', #129270, #110798, #93878, .T. ) ;
#49760 = CARTESIAN_POINT ( 'NONE',  ( 184.5000000000000000, 0.000000000000000000, -7.699999999999999289 ) ) ;
#49761 = AXIS2_PLACEMENT_3D ( 'NONE', #111864, #109267, #81737 ) ;
#49762 = DIRECTION ( 'NONE',  ( -0.000000000000000000, 1.000000000000000000, -0.000000000000000000 ) ) ;
#49763 = EDGE_CURVE ( 'NONE', #105720, #129537, #37606, .T. ) ;
#49764 = VERTEX_POINT ( 'NONE', #23858 ) ;
#49765 = EDGE_LOOP ( 'NONE', ( #79838, #42319, #16021, #91199 ) ) ;
#49766 = DIRECTION ( 'NONE',  ( 0.000000000000000000, 0.000000000000000000, 1.000000000000000000 ) ) ;
#49767 = CIRCLE ( 'NONE', #108233, 0.06509327318403745899 ) ;
#49768 = FACE_BOUND ( 'NONE', #17895, .T. ) ;
#49769 = DIRECTION ( 'NONE',  ( 0.000000000000000000, -0.9999939076577903929, 0.003490651415223739937 ) ) ;
#49770 = EDGE_CURVE ( 'NONE', #94750, #129385, #14583, .T. ) ;
#49773 = EDGE_CURVE ( 'NONE', #47419, #72591, #85610, .T. ) ;
#49772 = CIRCLE ( 'NONE', #39319, 0.06509327318403745899 ) ;
#49771 = COLOUR_RGB ( '', 0.09019608, 0.27058824, 0.51372549) ;
#49774 = DIRECTION ( 'NONE',  ( -0.000000000000000000, -1.000000000000000000, -0.000000000000000000 ) ) ;
#49775 = ORIENTED_EDGE ( 'NONE', *, *, #46411, .T. ) ;
#49776 = CARTESIAN_POINT ( 'NONE',  ( -10.60000000000000142, 12.50000000000000000, 4.676537180435972552 ) ) ;
#49777 = CARTESIAN_POINT ( 'NONE',  ( 184.3333333333333144, 6.668395609140177704, -3.849999999999998312 ) ) ;
#49778 = VERTEX_POINT ( 'NONE', #112877 ) ;
#49779 = DIRECTION ( 'NONE',  ( -0.000000000000000000, -1.000000000000000000, -0.000000000000000000 ) ) ;
#49780 = CARTESIAN_POINT ( 'NONE',  ( -2.300000000000032685, 12.50000000000000000, -4.611443907251940644 ) ) ;
#49781 = CARTESIAN_POINT ( 'NONE',  ( 6.449999999999930012, 12.50000000000000000, -1.818653347947326138 ) ) ;
#49782 = FACE_OUTER_BOUND ( 'NONE', #110340, .T. ) ;
#49783 = ORIENTED_EDGE ( 'NONE', *, *, #96856, .F. ) ;
#49784 = PLANE ( 'NONE',  #101048 ) ;
#49785 = DIRECTION ( 'NONE',  ( 0.000000000000000000, 0.000000000000000000, -1.000000000000000000 ) ) ;
#49786 = VECTOR ( 'NONE', #105329, 1000.000000000000000 ) ;
#49787 = CARTESIAN_POINT ( 'NONE',  ( 6.249999999999930722, 12.50000000000000000, 1.407149913249508000 ) ) ;
#49788 = CARTESIAN_POINT ( 'NONE',  ( 0.1999999999999562961, 2.500000000000000000, 4.676537180435972552 ) ) ;
#49789 = EDGE_LOOP ( 'NONE', ( #43751, #122665, #81726, #54689 ) ) ;
#49790 = AXIS2_PLACEMENT_3D ( 'NONE', #102563, #13539, #60726 ) ;
#49791 = EDGE_LOOP ( 'NONE', ( #2410, #56800, #3973, #39134 ) ) ;
#49792 = DIRECTION ( 'NONE',  ( -0.000000000000000000, 1.000000000000000000, -0.000000000000000000 ) ) ;
#49793 = EDGE_LOOP ( 'NONE', ( #35878, #21003 ) ) ;
#49794 = CARTESIAN_POINT ( 'NONE',  ( -3.100000000000028511, 2.500000000000000000, -4.676537180435977881 ) ) ;
#49795 = CARTESIAN_POINT ( 'NONE',  ( 87.50000000000000000, -7.499999999999999112, -0.6928095518838432998 ) ) ;
#49796 = VECTOR ( 'NONE', #98903, 1000.000000000000000 ) ;
#49797 = AXIS2_PLACEMENT_3D ( 'NONE', #128453, #129103, #58417 ) ;
#49798 = CARTESIAN_POINT ( 'NONE',  ( -13.14999999999999147, 12.50000000000000000, -1.753560074763286458 ) ) ;
#49799 = ORIENTED_EDGE ( 'NONE', *, *, #119973, .T. ) ;
#49800 = DIRECTION ( 'NONE',  ( 0.000000000000000000, 0.000000000000000000, -1.000000000000000000 ) ) ;
#49801 = CARTESIAN_POINT ( 'NONE',  ( 0.8499999999999545697, 2.500000000000000000, -1.372243186433550033 ) ) ;
#49802 = FACE_OUTER_BOUND ( 'NONE', #85839, .T. ) ;
#49803 = DIRECTION ( 'NONE',  ( 1.000000000000000000, 0.000000000000000000, 0.000000000000000000 ) ) ;
#49804 = DIRECTION ( 'NONE',  ( 0.000000000000000000, 0.000000000000000000, 1.000000000000000000 ) ) ;
#49805 = FACE_OUTER_BOUND ( 'NONE', #51997, .T. ) ;
#49806 = AXIS2_PLACEMENT_3D ( 'NONE', #86250, #76453, #93516 ) ;
#49807 = ORIENTED_EDGE ( 'NONE', *, *, #73366, .F. ) ;
#49808 = EDGE_CURVE ( 'NONE', #19578, #29149, #62646, .T. ) ;
#49810 = EDGE_LOOP ( 'NONE', ( #11473, #6070, #16987, #15811 ) ) ;
#49809 = CIRCLE ( 'NONE', #53999, 0.1000000000000002554 ) ;
#49811 = CARTESIAN_POINT ( 'NONE',  ( 8.749999999999923617, 2.500000000000000000, 1.372243186433545370 ) ) ;
#49812 = VERTEX_POINT ( 'NONE', #104339 ) ;
#49813 = CARTESIAN_POINT ( 'NONE',  ( 4.399999999999937295, 2.500000000000000000, 4.576537180435972019 ) ) ;
#49815 = ORIENTED_EDGE ( 'NONE', *, *, #58631, .T. ) ;
#49814 = EDGE_LOOP ( 'NONE', ( #52707, #78546, #127854, #32440 ) ) ;
#49816 = ORIENTED_EDGE ( 'NONE', *, *, #2589, .F. ) ;
#49817 = FACE_OUTER_BOUND ( 'NONE', #73827, .T. ) ;
#49819 = DIRECTION ( 'NONE',  ( 0.000000000000000000, 0.000000000000000000, -1.000000000000000000 ) ) ;
#49818 = AXIS2_PLACEMENT_3D ( 'NONE', #73918, #85018, #35296 ) ;
#49820 = DIRECTION ( 'NONE',  ( -0.000000000000000000, -1.000000000000000000, -0.000000000000000000 ) ) ;
#49821 =( NAMED_UNIT ( * ) SI_UNIT ( $, .STERADIAN. ) SOLID_ANGLE_UNIT ( ) );
#49822 = DIRECTION ( 'NONE',  ( 0.000000000000000000, 0.000000000000000000, -1.000000000000000000 ) ) ;
#49823 = CARTESIAN_POINT ( 'NONE',  ( -6.250000000000019540, 2.500000000000000000, -2.757883832488654097 ) ) ;
#49824 = CARTESIAN_POINT ( 'NONE',  ( 2.899999999999944844, 2.500000000000000000, 3.737306695894644371 ) ) ;
#49825 = CARTESIAN_POINT ( 'NONE',  ( 127.5000000000000000, -2.000000000000000000, -4.999999999999998224 ) ) ;
#49826 = AXIS2_PLACEMENT_3D ( 'NONE', #87176, #117931, #127133 ) ;
#49827 = LINE ( 'NONE', #70737, #100997 ) ;
#49828 = DIRECTION ( 'NONE',  ( 0.000000000000000000, 0.000000000000000000, 1.000000000000000000 ) ) ;
#49829 = EDGE_LOOP ( 'NONE', ( #108292, #59947 ) ) ;
#49830 = VECTOR ( 'NONE', #21500, 1000.000000000000000 ) ;
#49831 = ORIENTED_EDGE ( 'NONE', *, *, #23877, .T. ) ;
#49832 = COLOUR_RGB ( '', 0.31764706, 0.68627451, 0.89019608) ;
#49833 = LINE ( 'NONE', #70744, #125913 ) ;
#49834 = EDGE_LOOP ( 'NONE', ( #66733, #49970 ) ) ;
#49835 = VERTEX_POINT ( 'NONE', #104959 ) ;
#49836 = DIRECTION ( 'NONE',  ( -0.000000000000000000, -1.000000000000000000, -0.000000000000000000 ) ) ;
#49837 = VECTOR ( 'NONE', #96159, 1000.000000000000000 ) ;
#49839 = CONICAL_SURFACE ( 'NONE', #102058, 0.1000000000000000472, 0.003490658503988666988 ) ;
#49838 = LINE ( 'NONE', #70114, #119368 ) ;
#49840 = DIRECTION ( 'NONE',  ( -4.274815082592931898E-19, -0.9999939076577903929, -0.003490651415223739937 ) ) ;
#49841 = CARTESIAN_POINT ( 'NONE',  ( 162.5000000000000000, 0.5000000000000000000, 7.499999999999994671 ) ) ;
#49842 = CARTESIAN_POINT ( 'NONE',  ( -3.100000000000028955, 2.500000000000000000, 4.776537180435972196 ) ) ;
#49843 = ORIENTED_EDGE ( 'NONE', *, *, #107776, .T. ) ;
#49844 = CIRCLE ( 'NONE', #114663, 0.06509327318403745899 ) ;
#49845 = ORIENTED_EDGE ( 'NONE', *, *, #113657, .T. ) ;
#49846 = DIRECTION ( 'NONE',  ( 0.000000000000000000, -0.000000000000000000, 1.000000000000000000 ) ) ;
#49847 = EDGE_CURVE ( 'NONE', #115142, #55580, #100286, .T. ) ;
#49848 = VERTEX_POINT ( 'NONE', #23192 ) ;
#49849 = DIRECTION ( 'NONE',  ( 0.000000000000000000, 1.000000000000000000, 0.000000000000000000 ) ) ;
#49850 = ORIENTED_EDGE ( 'NONE', *, *, #57066, .T. ) ;
#49851 = AXIS2_PLACEMENT_3D ( 'NONE', #98677, #17538, #57488 ) ;
#49852 = EDGE_CURVE ( 'NONE', #29412, #41537, #123269, .T. ) ;
#49853 = VERTEX_POINT ( 'NONE', #72950 ) ;
#49854 = ADVANCED_FACE ( 'NONE', ( #63123 ), #81422, .T. ) ;
#49855 = CARTESIAN_POINT ( 'NONE',  ( -3.350000000000028511, 2.500000000000000000, 1.472243186433545459 ) ) ;
#49856 = DIRECTION ( 'NONE',  ( 0.000000000000000000, 0.000000000000000000, 1.000000000000000000 ) ) ;
#49858 = AXIS2_PLACEMENT_3D ( 'NONE', #28961, #100891, #109441 ) ;
#49857 = AXIS2_PLACEMENT_3D ( 'NONE', #38070, #80421, #17771 ) ;
#49859 = CARTESIAN_POINT ( 'NONE',  ( -5.000000000000024869, 2.500000000000000000, -5.022947341949754119 ) ) ;
#49860 = DIRECTION ( 'NONE',  ( 0.000000000000000000, 1.000000000000000000, 0.000000000000000000 ) ) ;
#49861 = EDGE_CURVE ( 'NONE', #87429, #41083, #43874, .T. ) ;
#49862 = CARTESIAN_POINT ( 'NONE',  ( -10.60000000000000142, 2.500000000000000000, 4.083716857408421497 ) ) ;
#49864 = VERTEX_POINT ( 'NONE', #125894 ) ;
#49863 = EDGE_CURVE ( 'NONE', #87369, #66203, #95167, .T. ) ;
#49865 = DIRECTION ( 'NONE',  ( 0.000000000000000000, -0.9999939076577903929, 0.003490651415223739937 ) ) ;
#49866 = DIRECTION ( 'NONE',  ( 0.000000000000000000, -0.000000000000000000, 1.000000000000000000 ) ) ;
#49867 = EDGE_CURVE ( 'NONE', #124699, #54263, #77455, .T. ) ;
#49868 = DIRECTION ( 'NONE',  ( -0.000000000000000000, -1.000000000000000000, -0.000000000000000000 ) ) ;
#49869 = EDGE_CURVE ( 'NONE', #99646, #36161, #118019, .T. ) ;
#49870 = ADVANCED_FACE ( 'NONE', ( #85967 ), #125268, .T. ) ;
#49871 = CARTESIAN_POINT ( 'NONE',  ( -3.749999999999991118, 2.500000000000000000, 2.065063509461097624 ) ) ;
#49872 = DIRECTION ( 'NONE',  ( 0.000000000000000000, 1.000000000000000000, 0.000000000000000000 ) ) ;
#49873 = ORIENTED_EDGE ( 'NONE', *, *, #26028, .F. ) ;
#49874 = ORIENTED_EDGE ( 'NONE', *, *, #22119, .T. ) ;
#49875 = AXIS2_PLACEMENT_3D ( 'NONE', #33359, #43820, #14318 ) ;
#49876 = CARTESIAN_POINT ( 'NONE',  ( 4.999999999999936939, 2.500000000000000000, -0.5928203230275541635 ) ) ;
#49877 = EDGE_CURVE ( 'NONE', #127950, #40372, #87656, .T. ) ;
#49878 = VERTEX_POINT ( 'NONE', #7410 ) ;
#49879 = CARTESIAN_POINT ( 'NONE',  ( 17.28960762337861468, -1.567482926518892761, 5.035524966326045515 ) ) ;
#49880 = DIRECTION ( 'NONE',  ( 0.000000000000000000, 0.000000000000000000, 1.000000000000000000 ) ) ;
#49881 = AXIS2_PLACEMENT_3D ( 'NONE', #20396, #60336, #100249 ) ;
#49882 = AXIS2_PLACEMENT_3D ( 'NONE', #98728, #9721, #67983 ) ;
#49883 = VERTEX_POINT ( 'NONE', #17883 ) ;
#49884 = CARTESIAN_POINT ( 'NONE',  ( 11.24999999999990763, 12.50000000000000000, -7.188010851410854052 ) ) ;
#49885 = CARTESIAN_POINT ( 'NONE',  ( 5.399999999999934630, 2.500000000000000000, -0.6928203230275542523 ) ) ;
#49886 = LINE ( 'NONE', #30893, #106803 ) ;
#49887 = FACE_OUTER_BOUND ( 'NONE', #102541, .T. ) ;
#49888 = AXIS2_PLACEMENT_3D ( 'NONE', #80222, #21960, #60594 ) ;
#49889 = CIRCLE ( 'NONE', #54073, 0.09999999999999982514 ) ;
#49890 = CONICAL_SURFACE ( 'NONE', #60270, 0.09999999999999982514, 0.003490658503988666988 ) ;
#49891 = DIRECTION ( 'NONE',  ( -4.274815082592931898E-19, -0.9999939076577903929, -0.003490651415223739937 ) ) ;
#49892 = ORIENTED_EDGE ( 'NONE', *, *, #61117, .F. ) ;
#49893 = CARTESIAN_POINT ( 'NONE',  ( 32.15747589919253357, 2.842529944137248243, -4.549402827138433913 ) ) ;
#49894 = DIRECTION ( 'NONE',  ( -0.000000000000000000, -1.000000000000000000, -0.000000000000000000 ) ) ;
#49895 = CIRCLE ( 'NONE', #62512, 0.06509327318403745899 ) ;
#49896 = CARTESIAN_POINT ( 'NONE',  ( 2.499999999999947153, 12.50000000000000000, 0.6928203230275494784 ) ) ;
#49897 = CONICAL_SURFACE ( 'NONE', #66597, 0.09999999999999982514, 0.003490658503988666988 ) ;
#49898 = ORIENTED_EDGE ( 'NONE', *, *, #106491, .F. ) ;
#49899 = CARTESIAN_POINT ( 'NONE',  ( -6.700000000000019718, 2.500000000000000000, 0.09999999999999761857 ) ) ;
#49900 = EDGE_CURVE ( 'NONE', #38154, #103846, #18712, .T. ) ;
#49901 = ORIENTED_EDGE ( 'NONE', *, *, #91687, .T. ) ;
#49902 = EDGE_CURVE ( 'NONE', #34505, #93321, #102349, .T. ) ;
#49903 = CARTESIAN_POINT ( 'NONE',  ( -2.500000000000032419, 2.500000000000000000, 0.6928203230275494784 ) ) ;
#49904 = CARTESIAN_POINT ( 'NONE',  ( 8.349999999999919709, 12.50000000000000000, 5.802370205355744659 ) ) ;
#49905 = CARTESIAN_POINT ( 'NONE',  ( 7.049999999999928768, 12.50000000000000000, 6.495190528383297135 ) ) ;
#49906 = EDGE_CURVE ( 'NONE', #7038, #103959, #94021, .T. ) ;
#49907 = EDGE_LOOP ( 'NONE', ( #26408, #59256 ) ) ;
#49908 = AXIS2_PLACEMENT_3D ( 'NONE', #90156, #18854, #60102 ) ;
#49909 = CARTESIAN_POINT ( 'NONE',  ( 12.29999999999990479, 2.500000000000000000, 4.676537180435972552 ) ) ;
#49910 = EDGE_CURVE ( 'NONE', #79180, #12963, #28367, .T. ) ;
#49911 = CARTESIAN_POINT ( 'NONE',  ( 185.3229166673494888, -4.445597072760063107, 7.700000000000102318 ) ) ;
#49912 = AXIS2_PLACEMENT_3D ( 'NONE', #127849, #67627, #97103 ) ;
#49913 = AXIS2_PLACEMENT_3D ( 'NONE', #38768, #78679, #79326 ) ;
#49914 = EDGE_LOOP ( 'NONE', ( #112964, #110283 ) ) ;
#49915 = DIRECTION ( 'NONE',  ( -4.274815082592931898E-19, -0.9999939076577903929, -0.003490651415223739937 ) ) ;
#49916 = EDGE_CURVE ( 'NONE', #124473, #4878, #96434, .T. ) ;
#49917 = ORIENTED_EDGE ( 'NONE', *, *, #32334, .F. ) ;
#49918 = CARTESIAN_POINT ( 'NONE',  ( 9.799999999999913669, 2.500000000000000000, -4.083716857408426826 ) ) ;
#49919 = EDGE_CURVE ( 'NONE', #67022, #126753, #35610, .T. ) ;
#49920 = EDGE_CURVE ( 'NONE', #50581, #20221, #14485, .T. ) ;
#49921 = EDGE_CURVE ( 'NONE', #53157, #79956, #47973, .T. ) ;
#49922 = ORIENTED_EDGE ( 'NONE', *, *, #115005, .T. ) ;
#49923 = COLOUR_RGB ( '', 0.31764706, 0.68627451, 0.89019608) ;
#49924 = DIRECTION ( 'NONE',  ( 0.000000000000000000, 0.000000000000000000, 1.000000000000000000 ) ) ;
#49925 = DIRECTION ( 'NONE',  ( 0.000000000000000000, -0.9999939076577903929, 0.003490651415223739937 ) ) ;
#49926 = ORIENTED_EDGE ( 'NONE', *, *, #7040, .F. ) ;
#49927 = ORIENTED_EDGE ( 'NONE', *, *, #34382, .F. ) ;
#49928 = PLANE ( 'NONE',  #20616 ) ;
#49929 = CARTESIAN_POINT ( 'NONE',  ( 8.949999999999921130, 2.500000000000000000, -6.841600689897078702 ) ) ;
#49930 = AXIS2_PLACEMENT_3D ( 'NONE', #110818, #31011, #31632 ) ;
#49931 = ORIENTED_EDGE ( 'NONE', *, *, #76219, .T. ) ;
#49932 = EDGE_CURVE ( 'NONE', #129526, #99163, #115413, .T. ) ;
#49933 = CARTESIAN_POINT ( 'NONE',  ( 3.749999999999944045, 2.500000000000000000, -2.857883832488653741 ) ) ;
#49934 = DIRECTION ( 'NONE',  ( -0.000000000000000000, 1.000000000000000000, -0.000000000000000000 ) ) ;
#49935 = CIRCLE ( 'NONE', #75047, 0.06509327318403745899 ) ;
#49936 = CARTESIAN_POINT ( 'NONE',  ( -11.44999999999999751, 2.500000000000000000, 6.048780366869521252 ) ) ;
#49937 = CARTESIAN_POINT ( 'NONE',  ( 106.3595851929959082, 7.300492252098111479, 4.734447472102021770 ) ) ;
#49938 = DIRECTION ( 'NONE',  ( 0.000000000000000000, 1.000000000000000000, 0.000000000000000000 ) ) ;
#49939 = DIRECTION ( 'NONE',  ( -0.000000000000000000, -1.000000000000000000, -0.000000000000000000 ) ) ;
#49940 = LINE ( 'NONE', #99671, #90226 ) ;
#49941 = CONICAL_SURFACE ( 'NONE', #102246, 0.1000000000000002554, 0.003490658503988666988 ) ;
#49942 = ORIENTED_EDGE ( 'NONE', *, *, #58487, .T. ) ;
#49943 = ORIENTED_EDGE ( 'NONE', *, *, #42016, .F. ) ;
#49946 = ORIENTED_EDGE ( 'NONE', *, *, #53015, .F. ) ;
#49945 = AXIS2_PLACEMENT_3D ( 'NONE', #84343, #94159, #114438 ) ;
#49944 = AXIS2_PLACEMENT_3D ( 'NONE', #11198, #89768, #40037 ) ;
#49947 = ORIENTED_EDGE ( 'NONE', *, *, #98802, .T. ) ;
#49948 = CARTESIAN_POINT ( 'NONE',  ( 13.34999999999989662, 2.500000000000000000, -1.372243186433550033 ) ) ;
#49949 = CARTESIAN_POINT ( 'NONE',  ( 2.299999999999948752, 2.500000000000000000, -3.883716857408426648 ) ) ;
#49950 = CARTESIAN_POINT ( 'NONE',  ( -10.40000000000000213, 12.50000000000000000, -2.276824562219559311E-15 ) ) ;
#49951 = AXIS2_PLACEMENT_3D ( 'NONE', #41728, #62005, #61355 ) ;
#49952 = EDGE_LOOP ( 'NONE', ( #83437, #27670, #21174, #84290 ) ) ;
#49953 = FACE_BOUND ( 'NONE', #125576, .T. ) ;
#49954 = EDGE_LOOP ( 'NONE', ( #127975, #128236 ) ) ;
#49955 = ADVANCED_FACE ( 'NONE', ( #65698 ), #87262, .T. ) ;
#49956 = DIRECTION ( 'NONE',  ( -0.000000000000000000, 1.000000000000000000, -0.000000000000000000 ) ) ;
#49957 = DIRECTION ( 'NONE',  ( 0.000000000000000000, 0.000000000000000000, 1.000000000000000000 ) ) ;
#49958 = CARTESIAN_POINT ( 'NONE',  ( -1.250000000000036193, 12.50000000000000000, 5.737276932171707422 ) ) ;
#49960 = CIRCLE ( 'NONE', #123096, 0.06509327318403745899 ) ;
#49959 = VECTOR ( 'NONE', #125481, 1000.000000000000000 ) ;
#49961 = CARTESIAN_POINT ( 'NONE',  ( 9.599999999999917932, 2.500000000000000000, -0.6928203230275541413 ) ) ;
#49962 = DIRECTION ( 'NONE',  ( 0.000000000000000000, 0.000000000000000000, -1.000000000000000000 ) ) ;
#49963 = DIRECTION ( 'NONE',  ( 0.000000000000000000, 1.000000000000000000, 0.000000000000000000 ) ) ;
#49964 = CARTESIAN_POINT ( 'NONE',  ( 1.649999999999951950, 12.50000000000000000, -5.802370205355749988 ) ) ;
#49965 = CARTESIAN_POINT ( 'NONE',  ( -4.150000000000024336, 12.50000000000000000, -2.230156782645139391 ) ) ;
#49966 = CARTESIAN_POINT ( 'NONE',  ( 6.899999999999926636, 12.50000000000000000, -0.4115034346978156399 ) ) ;
#49967 = ORIENTED_EDGE ( 'NONE', *, *, #63331, .T. ) ;
#49968 = ORIENTED_EDGE ( 'NONE', *, *, #103325, .F. ) ;
#49969 = EDGE_CURVE ( 'NONE', #12970, #128176, #16578, .T. ) ;
#49970 = ORIENTED_EDGE ( 'NONE', *, *, #86935, .T. ) ;
#49971 = EDGE_LOOP ( 'NONE', ( #64267, #13266, #30311, #78729 ) ) ;
#49972 = DIRECTION ( 'NONE',  ( 0.000000000000000000, 1.000000000000000000, 0.000000000000000000 ) ) ;
#49973 = AXIS2_PLACEMENT_3D ( 'NONE', #67940, #88201, #18193 ) ;
#49974 = DIRECTION ( 'NONE',  ( -0.000000000000000000, 1.000000000000000000, -0.000000000000000000 ) ) ;
#49976 = ORIENTED_EDGE ( 'NONE', *, *, #107799, .F. ) ;
#49975 = VERTEX_POINT ( 'NONE', #55875 ) ;
#49977 = ORIENTED_EDGE ( 'NONE', *, *, #54792, .F. ) ;
#49978 = DIRECTION ( 'NONE',  ( 0.000000000000000000, 1.000000000000000000, 0.000000000000000000 ) ) ;
#49979 = AXIS2_PLACEMENT_3D ( 'NONE', #8462, #47771, #87673 ) ;
#49980 = AXIS2_PLACEMENT_3D ( 'NONE', #29083, #21168, #123085 ) ;
#49981 = DIRECTION ( 'NONE',  ( 0.000000000000000000, -0.000000000000000000, 1.000000000000000000 ) ) ;
#49982 = CARTESIAN_POINT ( 'NONE',  ( -5.600000000000020073, 2.500000000000000000, 3.983716857408420964 ) ) ;
#49983 = CARTESIAN_POINT ( 'NONE',  ( 3.149999999999942624, 2.500000000000000000, 6.841600689897072485 ) ) ;
#49984 = DIRECTION ( 'NONE',  ( -0.000000000000000000, -1.000000000000000000, -0.000000000000000000 ) ) ;
#49985 = DIRECTION ( 'NONE',  ( 0.000000000000000000, -0.9999939076577903929, 0.003490651415223739937 ) ) ;
#49986 = CARTESIAN_POINT ( 'NONE',  ( -4.550000000000022915, 12.50000000000000000, 2.230156782645134950 ) ) ;
#49987 = ADVANCED_FACE ( 'NONE', ( #27698 ), #127844, .T. ) ;
#49988 = ORIENTED_EDGE ( 'NONE', *, *, #117380, .F. ) ;
#49990 = FACE_OUTER_BOUND ( 'NONE', #114980, .T. ) ;
#49989 = VECTOR ( 'NONE', #80416, 1000.000000000000000 ) ;
#49991 = EDGE_LOOP ( 'NONE', ( #45687, #89952, #102819, #128535 ) ) ;
#49992 = CONICAL_SURFACE ( 'NONE', #66671, 0.1000000000000002554, 0.003490658503988666988 ) ;
#49993 = ORIENTED_EDGE ( 'NONE', *, *, #93965, .F. ) ;
#49994 = VERTEX_POINT ( 'NONE', #10007 ) ;
#49995 = CARTESIAN_POINT ( 'NONE',  ( -0.4000000000000331624, 2.500000000000000000, -0.5928203230275518321 ) ) ;
#49996 = ORIENTED_EDGE ( 'NONE', *, *, #5934, .T. ) ;
#49997 = EDGE_LOOP ( 'NONE', ( #45557, #98634, #75104, #66501 ) ) ;
#49998 = AXIS2_PLACEMENT_3D ( 'NONE', #66941, #68889, #76140 ) ;
#49999 = DIRECTION ( 'NONE',  ( -0.000000000000000000, -1.000000000000000000, -0.000000000000000000 ) ) ;
#50000 = CIRCLE ( 'NONE', #31208, 0.09999999999999982514 ) ;
#50001 = CARTESIAN_POINT ( 'NONE',  ( 0.5999999999999621192, 12.50000000000000000, 0.4115034346978132529 ) ) ;
#50002 = PLANE ( 'NONE',  #77104 ) ;
#50003 = CARTESIAN_POINT ( 'NONE',  ( -14.34999999999998543, 2.500000000000000000, 2.511473670974877503 ) ) ;
#50004 = CARTESIAN_POINT ( 'NONE',  ( 2.049999999999950084, 2.500000000000000000, -2.165063509461101710 ) ) ;
#50005 = EDGE_LOOP ( 'NONE', ( #22442, #79368, #2130, #16439 ) ) ;
#50006 = CARTESIAN_POINT ( 'NONE',  ( 14.19999999999989626, 12.50000000000000000, -2.276824562219559311E-15 ) ) ;
#50007 = AXIS2_PLACEMENT_3D ( 'NONE', #48667, #79425, #69582 ) ;
#50008 = ORIENTED_EDGE ( 'NONE', *, *, #11037, .F. ) ;
#50009 = CARTESIAN_POINT ( 'NONE',  ( 7.949999999999925571, 2.500000000000000000, -6.495190528383302464 ) ) ;
#50010 = EDGE_CURVE ( 'NONE', #31018, #64039, #119068, .T. ) ;
#50011 = ORIENTED_EDGE ( 'NONE', *, *, #118658, .T. ) ;
#50012 = CARTESIAN_POINT ( 'NONE',  ( 109.6376890251878251, 7.303981195022478445, 4.727079717527256086 ) ) ;
#50013 = CARTESIAN_POINT ( 'NONE',  ( 3.749999999999940492, 12.50000000000000000, 2.857883832488649301 ) ) ;
#50014 = CONICAL_SURFACE ( 'NONE', #68852, 0.1000000000000000472, 0.003490658503988666988 ) ;
#50015 = ORIENTED_EDGE ( 'NONE', *, *, #34649, .F. ) ;
#50016 = DIRECTION ( 'NONE',  ( 0.000000000000000000, 0.000000000000000000, 1.000000000000000000 ) ) ;
#50017 = CARTESIAN_POINT ( 'NONE',  ( -11.84999999999999787, 2.500000000000000000, -6.941600689897074794 ) ) ;
#50018 = EDGE_LOOP ( 'NONE', ( #71050, #47748, #7435, #120621 ) ) ;
#50019 = EDGE_CURVE ( 'NONE', #82469, #54523, #64681, .T. ) ;
#50020 = CONICAL_SURFACE ( 'NONE', #70822, 0.09999999999999982514, 0.003490658503988666988 ) ;
#50021 = CARTESIAN_POINT ( 'NONE',  ( 3.149999999999944400, 12.50000000000000000, 1.818653347947321475 ) ) ;
#50022 = EDGE_LOOP ( 'NONE', ( #25137, #88712 ) ) ;
#50023 = EDGE_CURVE ( 'NONE', #116662, #104656, #31585, .T. ) ;
#50025 = EDGE_LOOP ( 'NONE', ( #68759, #30098, #126817, #3944 ) ) ;
#50024 = EDGE_CURVE ( 'NONE', #41483, #39986, #50131, .T. ) ;
#50026 = FACE_OUTER_BOUND ( 'NONE', #112747, .T. ) ;
#50027 = DIRECTION ( 'NONE',  ( 0.000000000000000000, 0.000000000000000000, -1.000000000000000000 ) ) ;
#50028 = EDGE_CURVE ( 'NONE', #85332, #24109, #125329, .T. ) ;
#50029 = CARTESIAN_POINT ( 'NONE',  ( 184.2968750003414300, 8.734944146203032389, 5.348610694689227483E-16 ) ) ;
#50030 = EDGE_CURVE ( 'NONE', #60931, #50358, #41421, .T. ) ;
#50032 = CIRCLE ( 'NONE', #39658, 0.1000000000000000472 ) ;
#50031 = CARTESIAN_POINT ( 'NONE',  ( -13.09999999999999254, 2.500000000000000000, 0.2464101615137777868 ) ) ;
#50033 = VECTOR ( 'NONE', #54066, 1000.000000000000000 ) ;
#50034 = DIRECTION ( 'NONE',  ( -0.000000000000000000, 1.000000000000000000, -0.000000000000000000 ) ) ;
#50035 = ORIENTED_EDGE ( 'NONE', *, *, #43687, .F. ) ;
#50036 = DIRECTION ( 'NONE',  ( 0.000000000000000000, -0.9999939076577903929, 0.003490651415223739937 ) ) ;
#50037 = VECTOR ( 'NONE', #101150, 1000.000000000000000 ) ;
#50038 = EDGE_CURVE ( 'NONE', #49975, #28873, #41721, .T. ) ;
#50039 = VERTEX_POINT ( 'NONE', #69560 ) ;
#50040 = EDGE_CURVE ( 'NONE', #7340, #63939, #83575, .T. ) ;
#50041 = CARTESIAN_POINT ( 'NONE',  ( -13.09999999999999254, 2.500000000000000000, -0.4464101615137741064 ) ) ;
#50042 = DIRECTION ( 'NONE',  ( 0.000000000000000000, 1.000000000000000000, 0.000000000000000000 ) ) ;
#50043 = ADVANCED_FACE ( 'NONE', ( #8690 ), #4118, .T. ) ;
#50044 = AXIS2_PLACEMENT_3D ( 'NONE', #117641, #115726, #48289 ) ;
#50045 = VECTOR ( 'NONE', #82122, 1000.000000000000000 ) ;
#50046 = PRODUCT_RELATED_PRODUCT_CATEGORY ( 'part', '', ( #95331 ) ) ;
#50047 = CARTESIAN_POINT ( 'NONE',  ( 186.6302083336747160, -4.367472073101514418, -7.564683531250002702 ) ) ;
#50048 = PLANE ( 'NONE',  #67732 ) ;
#50049 = PLANE ( 'NONE',  #86163 ) ;
#50050 = CARTESIAN_POINT ( 'NONE',  ( -1.650000000000034328, 12.50000000000000000, -2.230156782645139391 ) ) ;
#50051 = CARTESIAN_POINT ( 'NONE',  ( -1.650000000000034772, 2.500000000000000000, 5.802370205355744659 ) ) ;
#50052 = ORIENTED_EDGE ( 'NONE', *, *, #51958, .F. ) ;
#50054 = VECTOR ( 'NONE', #22685, 1000.000000000000000 ) ;
#50053 = AXIS2_PLACEMENT_3D ( 'NONE', #129545, #60155, #10384 ) ;
#50055 = FACE_OUTER_BOUND ( 'NONE', #107838, .T. ) ;
#50056 = FACE_OUTER_BOUND ( 'NONE', #44309, .T. ) ;
#50057 = DIRECTION ( 'NONE',  ( 0.000000000000000000, 1.000000000000000000, 0.000000000000000000 ) ) ;
#50058 = ORIENTED_EDGE ( 'NONE', *, *, #12560, .F. ) ;
#50059 = DIRECTION ( 'NONE',  ( 0.000000000000000000, 0.000000000000000000, -1.000000000000000000 ) ) ;
#50060 = VERTEX_POINT ( 'NONE', #119304 ) ;
#50061 = ORIENTED_EDGE ( 'NONE', *, *, #101964, .T. ) ;
#50062 = CARTESIAN_POINT ( 'NONE',  ( -3.950000000000029932, 2.500000000000000000, -6.148780366869526226 ) ) ;
#50063 = VECTOR ( 'NONE', #18531, 1000.000000000000000 ) ;
#50064 = ORIENTED_EDGE ( 'NONE', *, *, #100968, .T. ) ;
#50065 = DIRECTION ( 'NONE',  ( -0.000000000000000000, -1.000000000000000000, -0.000000000000000000 ) ) ;
#50066 = DIRECTION ( 'NONE',  ( 0.000000000000000000, 0.000000000000000000, 1.000000000000000000 ) ) ;
#50067 = VERTEX_POINT ( 'NONE', #90481 ) ;
#50068 = AXIS2_PLACEMENT_3D ( 'NONE', #84945, #124882, #25367 ) ;
#50069 = CARTESIAN_POINT ( 'NONE',  ( 10.64999999999991331, 12.50000000000000000, 6.776507416713035248 ) ) ;
#50070 = DIRECTION ( 'NONE',  ( -0.000000000000000000, -1.000000000000000000, -0.000000000000000000 ) ) ;
#50071 = FACE_OUTER_BOUND ( 'NONE', #45069, .T. ) ;
#50072 = EDGE_CURVE ( 'NONE', #35674, #9000, #60599, .T. ) ;
#50073 = CIRCLE ( 'NONE', #119001, 0.06509327318403745899 ) ;
#50074 = ORIENTED_EDGE ( 'NONE', *, *, #101011, .T. ) ;
#50075 = CIRCLE ( 'NONE', #4073, 0.06509327318403745899 ) ;
#50076 = EDGE_CURVE ( 'NONE', #57186, #83312, #21108, .T. ) ;
#50077 = CIRCLE ( 'NONE', #83518, 0.06509327318403745899 ) ;
#50078 = VERTEX_POINT ( 'NONE', #119963 ) ;
#50079 = EDGE_CURVE ( 'NONE', #103728, #91651, #78768, .T. ) ;
#50080 = ORIENTED_EDGE ( 'NONE', *, *, #36483, .T. ) ;
#50081 = DIRECTION ( 'NONE',  ( 0.000000000000000000, 0.000000000000000000, 1.000000000000000000 ) ) ;
#50082 = DIRECTION ( 'NONE',  ( -0.000000000000000000, -1.000000000000000000, -0.000000000000000000 ) ) ;
#50083 = CARTESIAN_POINT ( 'NONE',  ( 2.499999999999947153, 2.500000000000000000, 0.6928203230275494784 ) ) ;
#50084 = FACE_BOUND ( 'NONE', #23913, .T. ) ;
#50085 = ORIENTED_EDGE ( 'NONE', *, *, #95342, .F. ) ;
#50086 = AXIS2_PLACEMENT_3D ( 'NONE', #92390, #24951, #24308 ) ;
#50087 = CARTESIAN_POINT ( 'NONE',  ( -14.34999999999998543, 12.50000000000000000, -1.818653347947323695 ) ) ;
#50088 = CARTESIAN_POINT ( 'NONE',  ( 11.64999999999990266, 12.50000000000000000, 2.165063509461097713 ) ) ;
#50089 = ORIENTED_EDGE ( 'NONE', *, *, #19875, .T. ) ;
#50090 = EDGE_CURVE ( 'NONE', #98576, #94293, #83293, .T. ) ;
#50092 = DIRECTION ( 'NONE',  ( 0.000000000000000000, 1.000000000000000000, 0.000000000000000000 ) ) ;
#50091 = CONICAL_SURFACE ( 'NONE', #10351, 0.1000000000000002554, 0.003490658503988666988 ) ;
#50093 = CARTESIAN_POINT ( 'NONE',  ( -13.34999999999999076, 2.500000000000000000, -1.372243186433547812 ) ) ;
#50094 = CARTESIAN_POINT ( 'NONE',  ( -10.00000000000000533, 2.500000000000000000, 0.7928203230275495672 ) ) ;
#50095 = CARTESIAN_POINT ( 'NONE',  ( -6.650000000000014566, 2.500000000000000000, 1.572243186433545548 ) ) ;
#50096 = FACE_OUTER_BOUND ( 'NONE', #111601, .T. ) ;
#50097 = CARTESIAN_POINT ( 'NONE',  ( 1.849999999999951017, 2.500000000000000000, -6.248780366869526759 ) ) ;
#50098 = DIRECTION ( 'NONE',  ( 0.000000000000000000, 0.000000000000000000, 1.000000000000000000 ) ) ;
#50099 = ORIENTED_EDGE ( 'NONE', *, *, #97849, .F. ) ;
#50100 = VERTEX_POINT ( 'NONE', #68918 ) ;
#50101 = EDGE_LOOP ( 'NONE', ( #32855, #23230, #11646, #69496 ) ) ;
#50102 = VERTEX_POINT ( 'NONE', #108835 ) ;
#50103 = LINE ( 'NONE', #52023, #37009 ) ;
#50104 = CARTESIAN_POINT ( 'NONE',  ( -5.400000000000024336, 2.500000000000000000, -3.637306695894650055 ) ) ;
#50105 = ORIENTED_EDGE ( 'NONE', *, *, #126160, .F. ) ;
#50106 = FACE_BOUND ( 'NONE', #122501, .T. ) ;
#50107 = EDGE_CURVE ( 'NONE', #74504, #88669, #129166, .T. ) ;
#50108 = DIRECTION ( 'NONE',  ( 0.000000000000000000, 1.000000000000000000, 0.000000000000000000 ) ) ;
#50109 = FACE_OUTER_BOUND ( 'NONE', #8761, .T. ) ;
#50110 = CARTESIAN_POINT ( 'NONE',  ( 1.449999999999951328, 2.500000000000000000, 2.511473670974873507 ) ) ;
#50111 = DIRECTION ( 'NONE',  ( 0.000000000000000000, 0.000000000000000000, 1.000000000000000000 ) ) ;
#50112 = CARTESIAN_POINT ( 'NONE',  ( 3.149999999999942624, 2.500000000000000000, 6.248780366869521430 ) ) ;
#50113 = LINE ( 'NONE', #128687, #124950 ) ;
#50114 = EDGE_LOOP ( 'NONE', ( #95492, #91559 ) ) ;
#50115 = EDGE_LOOP ( 'NONE', ( #7804, #39267 ) ) ;
#50116 = ORIENTED_EDGE ( 'NONE', *, *, #61739, .F. ) ;
#50117 = VERTEX_POINT ( 'NONE', #120605 ) ;
#50118 = ADVANCED_FACE ( 'NONE', ( #51243 ), #19155, .T. ) ;
#50119 = ORIENTED_EDGE ( 'NONE', *, *, #49916, .T. ) ;
#50120 = EDGE_LOOP ( 'NONE', ( #50772, #30017, #26765, #12196 ) ) ;
#50121 = DIRECTION ( 'NONE',  ( -0.000000000000000000, 1.000000000000000000, -0.000000000000000000 ) ) ;
#50122 = FACE_OUTER_BOUND ( 'NONE', #65732, .T. ) ;
#50123 = VECTOR ( 'NONE', #104050, 1000.000000000000000 ) ;
#50124 = ORIENTED_EDGE ( 'NONE', *, *, #24864, .F. ) ;
#50125 = PLANE ( 'NONE',  #99932 ) ;
#50127 = CARTESIAN_POINT ( 'NONE',  ( 13.34999999999989662, 12.50000000000000000, -2.857883832488653741 ) ) ;
#50126 = AXIS2_PLACEMENT_3D ( 'NONE', #8149, #36982, #27790 ) ;
#50128 = CARTESIAN_POINT ( 'NONE',  ( 185.4843750003414300, -8.734944146203032389, -1.604583208406768146E-15 ) ) ;
#50129 = DIRECTION ( 'NONE',  ( 0.000000000000000000, 1.000000000000000000, 0.000000000000000000 ) ) ;
#50130 = CARTESIAN_POINT ( 'NONE',  ( -0.4000000000000401013, 2.500000000000000000, -3.537306695894649966 ) ) ;
#50131 = CIRCLE ( 'NONE', #127479, 0.06509327318403741736 ) ;
#50132 = EDGE_CURVE ( 'NONE', #38338, #105257, #56162, .T. ) ;
#50133 = ORIENTED_EDGE ( 'NONE', *, *, #38479, .T. ) ;
#50134 = DIRECTION ( 'NONE',  ( 0.000000000000000000, 0.000000000000000000, 1.000000000000000000 ) ) ;
#50135 = VECTOR ( 'NONE', #59855, 1000.000000000000000 ) ;
#50136 = ORIENTED_EDGE ( 'NONE', *, *, #126969, .T. ) ;
#50137 = VERTEX_POINT ( 'NONE', #60420 ) ;
#50138 = CARTESIAN_POINT ( 'NONE',  ( -14.34999999999998543, 2.500000000000000000, 1.818653347947325472 ) ) ;
#50139 = CARTESIAN_POINT ( 'NONE',  ( -6.850000000000013856, 12.50000000000000000, 2.511473670974873507 ) ) ;
#50141 = EDGE_CURVE ( 'NONE', #94650, #109859, #74961, .T. ) ;
#50140 = CARTESIAN_POINT ( 'NONE',  ( -10.60000000000000320, 12.50000000000000000, -4.676537180435973440 ) ) ;
#50142 = VERTEX_POINT ( 'NONE', #13210 ) ;
#50143 = VERTEX_POINT ( 'NONE', #23693 ) ;
#50144 = CARTESIAN_POINT ( 'NONE',  ( -9.150000000000009237, 12.50000000000000000, 2.165063509461097713 ) ) ;
#50145 = FACE_OUTER_BOUND ( 'NONE', #90644, .T. ) ;
#50146 = CARTESIAN_POINT ( 'NONE',  ( 127.5000000000000000, -1.500000000000000000, -6.000000000000000000 ) ) ;
#50147 = DIRECTION ( 'NONE',  ( 0.000000000000000000, 0.000000000000000000, 1.000000000000000000 ) ) ;
#50148 = ORIENTED_EDGE ( 'NONE', *, *, #18343, .T. ) ;
#50149 = DIRECTION ( 'NONE',  ( 0.000000000000000000, -0.9999939076577903929, 0.003490651415223739937 ) ) ;
#50150 = ORIENTED_EDGE ( 'NONE', *, *, #14023, .T. ) ;
#50151 = CARTESIAN_POINT ( 'NONE',  ( 16.55874544816221317, -0.4845305829210151960, -6.091953208799018249 ) ) ;
#50152 = CIRCLE ( 'NONE', #37629, 0.06509327318403745899 ) ;
#50153 = VECTOR ( 'NONE', #558, 1000.000000000000000 ) ;
#50154 = VERTEX_POINT ( 'NONE', #63626 ) ;
#50155 = CARTESIAN_POINT ( 'NONE',  ( 186.3333333333333144, 6.668395609140177704, -3.849999999999998312 ) ) ;
#50156 = ADVANCED_FACE ( 'NONE', ( #21770 ), #16445, .T. ) ;
#50157 = CARTESIAN_POINT ( 'NONE',  ( 59.86275542849503495, -3.775834014907373248, 4.995382520279711080 ) ) ;
#50158 = DIRECTION ( 'NONE',  ( 0.000000000000000000, -0.9999939076577903929, 0.003490651415223739937 ) ) ;
#50159 = CARTESIAN_POINT ( 'NONE',  ( 12.09999999999990550, 2.500000000000000000, 3.737306695894644371 ) ) ;
#50160 = VERTEX_POINT ( 'NONE', #11929 ) ;
#50161 = AXIS2_PLACEMENT_3D ( 'NONE', #17951, #45497, #26494 ) ;
#50162 = EDGE_CURVE ( 'NONE', #10500, #47021, #64489, .T. ) ;
#50163 = CARTESIAN_POINT ( 'NONE',  ( 4.399999999999937295, 12.50000000000000000, 4.676537180435972552 ) ) ;
#50164 = DIRECTION ( 'NONE',  ( 0.000000000000000000, 0.000000000000000000, 1.000000000000000000 ) ) ;
#50165 = EDGE_LOOP ( 'NONE', ( #99608, #70746 ) ) ;
#50166 = EDGE_LOOP ( 'NONE', ( #70410, #75465, #9719, #27549 ) ) ;
#50167 = EDGE_CURVE ( 'NONE', #111265, #91437, #31346, .T. ) ;
#50169 = ORIENTED_EDGE ( 'NONE', *, *, #119651, .F. ) ;
#50168 = EDGE_CURVE ( 'NONE', #90001, #111704, #18519, .T. ) ;
#50170 = DIRECTION ( 'NONE',  ( 0.000000000000000000, 0.000000000000000000, 1.000000000000000000 ) ) ;
#50171 = CARTESIAN_POINT ( 'NONE',  ( -0.8500000000000386136, 2.500000000000000000, 5.802370205355744659 ) ) ;
#50172 = CARTESIAN_POINT ( 'NONE',  ( -10.84999999999999964, 2.500000000000000000, 2.757883832488649656 ) ) ;
#50173 = EDGE_CURVE ( 'NONE', #63537, #12708, #102154, .T. ) ;
#50174 =( NAMED_UNIT ( * ) SI_UNIT ( $, .STERADIAN. ) SOLID_ANGLE_UNIT ( ) );
#50176 = EDGE_CURVE ( 'NONE', #70566, #83042, #89629, .T. ) ;
#50175 = AXIS2_PLACEMENT_3D ( 'NONE', #29611, #51204, #70824 ) ;
#50177 = CARTESIAN_POINT ( 'NONE',  ( -0.2000000000000408673, 2.500000000000000000, -3.983716857408426293 ) ) ;
#50178 = DIRECTION ( 'NONE',  ( 0.000000000000000000, 1.000000000000000000, 0.000000000000000000 ) ) ;
#50179 = VECTOR ( 'NONE', #30266, 1000.000000000000000 ) ;
#50180 = DIRECTION ( 'NONE',  ( 0.000000000000000000, -0.000000000000000000, 1.000000000000000000 ) ) ;
#50181 = FACE_OUTER_BOUND ( 'NONE', #122342, .T. ) ;
#50182 = DIRECTION ( 'NONE',  ( -0.000000000000000000, -1.000000000000000000, -0.000000000000000000 ) ) ;
#50183 = EDGE_CURVE ( 'NONE', #102067, #27968, #33527, .T. ) ;
#50184 = EDGE_CURVE ( 'NONE', #51769, #79731, #83269, .T. ) ;
#50185 = CIRCLE ( 'NONE', #110797, 0.06509327318403745899 ) ;
#50186 = VECTOR ( 'NONE', #4602, 1000.000000000000000 ) ;
#50187 = ADVANCED_FACE ( 'NONE', ( #22426 ), #43989, .T. ) ;
#50188 = ADVANCED_FACE ( 'NONE', ( #93092 ), #51986, .T. ) ;
#50189 = EDGE_LOOP ( 'NONE', ( #41371, #52220, #86403, #23848 ) ) ;
#50190 = VECTOR ( 'NONE', #48448, 1000.000000000000000 ) ;
#50191 = DIRECTION ( 'NONE',  ( 0.000000000000000000, -0.9999939076577903929, 0.003490651415223739937 ) ) ;
#50192 = FACE_OUTER_BOUND ( 'NONE', #34840, .T. ) ;
#50193 = CARTESIAN_POINT ( 'NONE',  ( -12.49999999999999289, 12.50000000000000000, 3.572213422710607489 ) ) ;
#50194 = LINE ( 'NONE', #41666, #52640 ) ;
#50195 = CARTESIAN_POINT ( 'NONE',  ( -6.450000000000014388, 2.500000000000000000, 6.248780366869521430 ) ) ;
#50196 = EDGE_CURVE ( 'NONE', #46534, #83081, #49844, .T. ) ;
#50197 = ORIENTED_EDGE ( 'NONE', *, *, #104485, .F. ) ;
#50198 = DIRECTION ( 'NONE',  ( 0.000000000000000000, 0.000000000000000000, 1.000000000000000000 ) ) ;
#50199 = PLANE ( 'NONE',  #40766 ) ;
#50201 = ORIENTED_EDGE ( 'NONE', *, *, #120026, .T. ) ;
#50200 = DIRECTION ( 'NONE',  ( -0.000000000000000000, 1.000000000000000000, -0.000000000000000000 ) ) ;
#50202 =( BOUNDED_CURVE ( )  B_SPLINE_CURVE ( 2, ( #60512, #49402, #51339, #101712, #19256, #921, #11381 ),
 .UNSPECIFIED., .F., .F. ) 
 B_SPLINE_CURVE_WITH_KNOTS ( ( 3, 2, 2, 3 ),
 ( 0.8571428571428578724, 0.8809523809523817084, 0.9047619047619054333, 0.9285714285714292693 ),
 .UNSPECIFIED. ) 
 CURVE ( )  GEOMETRIC_REPRESENTATION_ITEM ( )  RATIONAL_B_SPLINE_CURVE ( ( 0.9999999999999956701, 0.8660254037844430375, 1.000000000000000000, 0.8660254037844387076, 1.000000000000000000, 0.8660254037844349329, 1.000000000000003775 ) ) 
 REPRESENTATION_ITEM ( '' )  );
#50203 = EDGE_LOOP ( 'NONE', ( #19186, #92945, #127463, #8083 ) ) ;
#50204 = PLANE ( 'NONE',  #703 ) ;
#50205 = VERTEX_POINT ( 'NONE', #82628 ) ;
#50206 = ORIENTED_EDGE ( 'NONE', *, *, #60251, .F. ) ;
#50207 = CARTESIAN_POINT ( 'NONE',  ( 3.099999999999945022, 2.500000000000000000, -0.4464101615137783252 ) ) ;
#50208 = CARTESIAN_POINT ( 'NONE',  ( 20.06694580393876137, 2.635910463901537160, -2.269534205243695091 ) ) ;
#50209 = DIRECTION ( 'NONE',  ( 0.000000000000000000, 0.000000000000000000, -1.000000000000000000 ) ) ;
#50210 = CARTESIAN_POINT ( 'NONE',  ( 14.59999999999989484, 12.50000000000000000, 0.7579135962115869374 ) ) ;
#50211 = VERTEX_POINT ( 'NONE', #112078 ) ;
#50213 = CONICAL_SURFACE ( 'NONE', #98303, 0.1000000000000002554, 0.003490658503988666988 ) ;
#50212 = AXIS2_PLACEMENT_3D ( 'NONE', #51968, #101707, #10096 ) ;
#50214 = CARTESIAN_POINT ( 'NONE',  ( 11.89999999999990443, 2.500000000000000000, 0.4464101615137736623 ) ) ;
#50215 = ORIENTED_EDGE ( 'NONE', *, *, #84906, .T. ) ;
#50216 = FACE_OUTER_BOUND ( 'NONE', #48994, .T. ) ;
#50217 = DIRECTION ( 'NONE',  ( -4.274815082592931898E-19, -0.9999939076577903929, -0.003490651415223739937 ) ) ;
#50218 = LINE ( 'NONE', #88165, #127006 ) ;
#50219 = ORIENTED_EDGE ( 'NONE', *, *, #55304, .F. ) ;
#50220 = AXIS2_PLACEMENT_3D ( 'NONE', #25689, #35532, #87178 ) ;
#50221 = EDGE_CURVE ( 'NONE', #125995, #117711, #58021, .T. ) ;
#50222 = EDGE_LOOP ( 'NONE', ( #13389, #111835, #92422, #62580 ) ) ;
#50223 = ORIENTED_EDGE ( 'NONE', *, *, #2219, .T. ) ;
#50225 = ADVANCED_FACE ( 'NONE', ( #104183 ), #32889, .T. ) ;
#50224 = EDGE_LOOP ( 'NONE', ( #414, #44326 ) ) ;
#50226 = ORIENTED_EDGE ( 'NONE', *, *, #39538, .F. ) ;
#50227 = CARTESIAN_POINT ( 'NONE',  ( 6.449999999999930012, 12.50000000000000000, 1.883746621131358934 ) ) ;
#50228 = CARTESIAN_POINT ( 'NONE',  ( 10.89704209839426419, 1.499999999999809708, 8.980393934824158819 ) ) ;
#50229 = CARTESIAN_POINT ( 'NONE',  ( -9.350000000000006750, 2.500000000000000000, 2.511473670974873507 ) ) ;
#50230 = FACE_BOUND ( 'NONE', #2177, .T. ) ;
#50231 = DIRECTION ( 'NONE',  ( -0.000000000000000000, 1.000000000000000000, -0.000000000000000000 ) ) ;
#50232 = CARTESIAN_POINT ( 'NONE',  ( 187.0729166673494319, 4.445597072760120838, -7.699999999999998401 ) ) ;
#50233 = DIRECTION ( 'NONE',  ( 0.000000000000000000, 0.000000000000000000, 1.000000000000000000 ) ) ;
#50234 = DIRECTION ( 'NONE',  ( -0.000000000000000000, 1.000000000000000000, -0.000000000000000000 ) ) ;
#50235 = CARTESIAN_POINT ( 'NONE',  ( -14.79999999999998472, 12.50000000000000000, 0.3464101615137758494 ) ) ;
#50236 = CARTESIAN_POINT ( 'NONE',  ( 165.4999999999999716, 0.000000000000000000, -2.500000000000000000 ) ) ;
#50237 = DIRECTION ( 'NONE',  ( 0.000000000000000000, 0.000000000000000000, 1.000000000000000000 ) ) ;
#50238 = CIRCLE ( 'NONE', #81533, 0.06509327318403745899 ) ;
#50239 = CONICAL_SURFACE ( 'NONE', #64799, 0.1000000000000000472, 0.003490658503988666988 ) ;
#50240 = DIRECTION ( 'NONE',  ( 0.000000000000000000, 1.000000000000000000, 0.000000000000000000 ) ) ;
#50241 = ORIENTED_EDGE ( 'NONE', *, *, #85583, .T. ) ;
#50242 = VERTEX_POINT ( 'NONE', #94353 ) ;
#50243 = ORIENTED_EDGE ( 'NONE', *, *, #4766, .F. ) ;
#50244 = ORIENTED_EDGE ( 'NONE', *, *, #107469, .F. ) ;
#50245 = DIRECTION ( 'NONE',  ( -0.000000000000000000, 1.000000000000000000, -0.000000000000000000 ) ) ;
#50246 = CARTESIAN_POINT ( 'NONE',  ( 12.09999999999990550, 2.500000000000000000, -3.637306695894650055 ) ) ;
#50247 = FACE_BOUND ( 'NONE', #49954, .T. ) ;
#50248 = LINE ( 'NONE', #39796, #54038 ) ;
#50249 = VERTEX_POINT ( 'NONE', #62971 ) ;
#50250 = FACE_OUTER_BOUND ( 'NONE', #77382, .T. ) ;
#50251 = CARTESIAN_POINT ( 'NONE',  ( -13.29999999999999005, 2.500000000000000000, -4.230127018922199333 ) ) ;
#50252 = CARTESIAN_POINT ( 'NONE',  ( -6.050000000000022027, 2.500000000000000000, -6.148780366869526226 ) ) ;
#50253 = CARTESIAN_POINT ( 'NONE',  ( 7.499999999999961808, 2.500000000000000000, 4.430127018922196847 ) ) ;
#50254 = CIRCLE ( 'NONE', #119205, 0.06509327318403745899 ) ;
#50255 = ORIENTED_EDGE ( 'NONE', *, *, #99513, .T. ) ;
#50256 = DIRECTION ( 'NONE',  ( 0.000000000000000000, 0.000000000000000000, 1.000000000000000000 ) ) ;
#50258 = ADVANCED_FACE ( 'NONE', ( #4663 ), #33214, .T. ) ;
#50257 = CONICAL_SURFACE ( 'NONE', #56493, 0.1000000000000002554, 0.003490658503988666988 ) ;
#50259 = VERTEX_POINT ( 'NONE', #124475 ) ;
#50260 = ORIENTED_EDGE ( 'NONE', *, *, #2365, .F. ) ;
#50261 = DIRECTION ( 'NONE',  ( 0.000000000000000000, 0.000000000000000000, -1.000000000000000000 ) ) ;
#50262 = CARTESIAN_POINT ( 'NONE',  ( 5.399999999999931966, 2.500000000000000000, 4.330127018922196314 ) ) ;
#50263 = ORIENTED_EDGE ( 'NONE', *, *, #88559, .T. ) ;
#50264 = CARTESIAN_POINT ( 'NONE',  ( 108.0000000000000142, 8.500000000000000000, -2.249999999999996891 ) ) ;
#50265 = DIRECTION ( 'NONE',  ( -0.000000000000000000, -1.000000000000000000, -0.000000000000000000 ) ) ;
#50266 = DIRECTION ( 'NONE',  ( 0.000000000000000000, -0.000000000000000000, 1.000000000000000000 ) ) ;
#50267 = VECTOR ( 'NONE', #96573, 1000.000000000000000 ) ;
#50268 = ORIENTED_EDGE ( 'NONE', *, *, #20860, .F. ) ;
#50269 = EDGE_CURVE ( 'NONE', #15198, #7354, #8046, .T. ) ;
#50270 = EDGE_CURVE ( 'NONE', #100839, #59702, #26914, .T. ) ;
#50271 = DIRECTION ( 'NONE',  ( 0.000000000000000000, 1.000000000000000000, 0.000000000000000000 ) ) ;
#50272 = EDGE_LOOP ( 'NONE', ( #122410, #20423, #6362, #102612 ) ) ;
#50273 = DIRECTION ( 'NONE',  ( 0.000000000000000000, 0.000000000000000000, -1.000000000000000000 ) ) ;
#50274 = ORIENTED_EDGE ( 'NONE', *, *, #3963, .T. ) ;
#50275 = CARTESIAN_POINT ( 'NONE',  ( 109.3324905233811393, 5.996841997646892075, 4.830676265755256438 ) ) ;
#50276 = EDGE_LOOP ( 'NONE', ( #47758, #111883, #29131, #41738 ) ) ;
#50277 = FACE_OUTER_BOUND ( 'NONE', #77551, .T. ) ;
#50278 = DIRECTION ( 'NONE',  ( 0.000000000000000000, 0.000000000000000000, 1.000000000000000000 ) ) ;
#50279 = DIRECTION ( 'NONE',  ( 0.000000000000000000, 0.000000000000000000, 1.000000000000000000 ) ) ;
#50281 = EDGE_CURVE ( 'NONE', #91248, #60649, #10118, .T. ) ;
#50280 = DIRECTION ( 'NONE',  ( -0.000000000000000000, -1.000000000000000000, -0.000000000000000000 ) ) ;
#50282 = DIRECTION ( 'NONE',  ( 0.000000000000000000, -0.000000000000000000, 1.000000000000000000 ) ) ;
#50283 = VERTEX_POINT ( 'NONE', #66182 ) ;
#50284 = ORIENTED_EDGE ( 'NONE', *, *, #84438, .T. ) ;
#50285 = ORIENTED_EDGE ( 'NONE', *, *, #53423, .T. ) ;
#50286 = DIRECTION ( 'NONE',  ( -0.000000000000000000, 1.000000000000000000, -0.000000000000000000 ) ) ;
#50287 = CARTESIAN_POINT ( 'NONE',  ( 179.5000000000000000, 1.375000000000000000, 7.634788798650556707 ) ) ;
#50289 = DIRECTION ( 'NONE',  ( -0.000000000000000000, 1.000000000000000000, -0.000000000000000000 ) ) ;
#50288 = AXIS2_PLACEMENT_3D ( 'NONE', #57378, #9567, #108402 ) ;
#50291 = VERTEX_POINT ( 'NONE', #36750 ) ;
#50290 = ORIENTED_EDGE ( 'NONE', *, *, #106888, .F. ) ;
#50292 = ORIENTED_EDGE ( 'NONE', *, *, #116237, .F. ) ;
#50293 = AXIS2_PLACEMENT_3D ( 'NONE', #90851, #102594, #2449 ) ;
#50294 = DIRECTION ( 'NONE',  ( 0.000000000000000000, 0.000000000000000000, -1.000000000000000000 ) ) ;
#50295 = EDGE_LOOP ( 'NONE', ( #90470, #44736, #60897, #31294 ) ) ;
#50296 = CARTESIAN_POINT ( 'NONE',  ( 12.89999999999989910, 12.50000000000000000, -0.6928203230275542523 ) ) ;
#50297 = CIRCLE ( 'NONE', #41981, 0.06509327318403745899 ) ;
#50298 = CARTESIAN_POINT ( 'NONE',  ( -4.400000000000028777, 12.50000000000000000, -3.983716857408426293 ) ) ;
#50299 = CARTESIAN_POINT ( 'NONE',  ( -6.650000000000014566, 12.50000000000000000, 1.472243186433545459 ) ) ;
#50300 = LINE ( 'NONE', #9729, #69578 ) ;
#50301 = DIRECTION ( 'NONE',  ( 0.000000000000000000, 0.000000000000000000, 1.000000000000000000 ) ) ;
#50302 = CARTESIAN_POINT ( 'NONE',  ( -4.800000000000022915, 2.500000000000000000, 3.983716857408420076 ) ) ;
#50303 = CARTESIAN_POINT ( 'NONE',  ( -12.94999999999999218, 2.500000000000000000, 2.165063509461101265 ) ) ;
#50304 = EDGE_LOOP ( 'NONE', ( #10288, #108403 ) ) ;
#50305 = ORIENTED_EDGE ( 'NONE', *, *, #14693, .T. ) ;
#50306 = EDGE_CURVE ( 'NONE', #46758, #97470, #106350, .T. ) ;
#50307 = PLANE ( 'NONE',  #59116 ) ;
#50308 = ORIENTED_EDGE ( 'NONE', *, *, #34059, .F. ) ;
#50309 = ORIENTED_EDGE ( 'NONE', *, *, #65818, .F. ) ;
#50310 = ADVANCED_FACE ( 'NONE', ( #105477 ), #45724, .T. ) ;
#50311 = DIRECTION ( 'NONE',  ( 0.000000000000000000, 1.000000000000000000, 0.000000000000000000 ) ) ;
#50312 = CARTESIAN_POINT ( 'NONE',  ( -2.900000000000029665, 12.50000000000000000, 4.330127018922196314 ) ) ;
#50313 = DIRECTION ( 'NONE',  ( -0.000000000000000000, 1.000000000000000000, -0.000000000000000000 ) ) ;
#50314 = EDGE_CURVE ( 'NONE', #71164, #129204, #16414, .T. ) ;
#50315 = DIRECTION ( 'NONE',  ( 0.000000000000000000, 1.000000000000000000, 0.000000000000000000 ) ) ;
#50316 = DIRECTION ( 'NONE',  ( 0.000000000000000000, 0.000000000000000000, 1.000000000000000000 ) ) ;
#50317 = DIRECTION ( 'NONE',  ( 0.000000000000000000, 0.000000000000000000, 1.000000000000000000 ) ) ;
#50318 = DIRECTION ( 'NONE',  ( 0.000000000000000000, 0.000000000000000000, 1.000000000000000000 ) ) ;
#50319 = EDGE_CURVE ( 'NONE', #58972, #49723, #43588, .T. ) ;
#50320 = EDGE_CURVE ( 'NONE', #17512, #74641, #68693, .T. ) ;
#50321 = ADVANCED_FACE ( 'NONE', ( #86466 ), #116712, .T. ) ;
#50322 = DIRECTION ( 'NONE',  ( 0.000000000000000000, -0.9999939076577903929, 0.003490651415223739937 ) ) ;
#50323 = AXIS2_PLACEMENT_3D ( 'NONE', #10539, #119864, #80595 ) ;
#50325 = ORIENTED_EDGE ( 'NONE', *, *, #91780, .T. ) ;
#50324 = AXIS2_PLACEMENT_3D ( 'NONE', #50955, #10994, #90861 ) ;
#50326 = EDGE_CURVE ( 'NONE', #62091, #23183, #3850, .T. ) ;
#50327 = ORIENTED_EDGE ( 'NONE', *, *, #87512, .F. ) ;
#50328 = ORIENTED_EDGE ( 'NONE', *, *, #64738, .T. ) ;
#50329 = ORIENTED_EDGE ( 'NONE', *, *, #34066, .T. ) ;
#50330 = PLANE ( 'NONE',  #33692 ) ;
#50331 = FACE_OUTER_BOUND ( 'NONE', #91289, .T. ) ;
#50333 = EDGE_CURVE ( 'NONE', #84351, #2148, #95891, .T. ) ;
#50332 = CIRCLE ( 'NONE', #54518, 0.06509327318403745899 ) ;
#50334 = ORIENTED_EDGE ( 'NONE', *, *, #107198, .F. ) ;
#50335 = PLANE ( 'NONE',  #48607 ) ;
#50336 = CARTESIAN_POINT ( 'NONE',  ( 186.1145833340161175, 6.668395609140177704, -3.849999999999998312 ) ) ;
#50337 = CARTESIAN_POINT ( 'NONE',  ( -1.700000000000034817, 12.50000000000000000, -2.385244779468109755E-15 ) ) ;
#50339 = ORIENTED_EDGE ( 'NONE', *, *, #14077, .F. ) ;
#50338 = CARTESIAN_POINT ( 'NONE',  ( 7.899999999999924860, 2.500000000000000000, 5.022947341949748790 ) ) ;
#50340 = CARTESIAN_POINT ( 'NONE',  ( -10.45000000000000107, 2.500000000000000000, 6.595190528383296780 ) ) ;
#50341 = CARTESIAN_POINT ( 'NONE',  ( -3.950000000000024603, 12.50000000000000000, -2.446380397790840266 ) ) ;
#50342 = AXIS2_PLACEMENT_3D ( 'NONE', #119092, #118437, #28787 ) ;
#50343 = ORIENTED_EDGE ( 'NONE', *, *, #122609, .T. ) ;
#50344 = VERTEX_POINT ( 'NONE', #95653 ) ;
#50345 = ORIENTED_EDGE ( 'NONE', *, *, #96751, .T. ) ;
#50346 = ORIENTED_EDGE ( 'NONE', *, *, #122540, .T. ) ;
#50347 = DIRECTION ( 'NONE',  ( 0.000000000000000000, 1.000000000000000000, 0.000000000000000000 ) ) ;
#50348 = VECTOR ( 'NONE', #25395, 1000.000000000000000 ) ;
#50349 = CARTESIAN_POINT ( 'NONE',  ( 2.499999999999948930, 2.500000000000000000, -4.922947341949753586 ) ) ;
#50350 = DIRECTION ( 'NONE',  ( 0.000000000000000000, 1.000000000000000000, 0.000000000000000000 ) ) ;
#50351 = AXIS2_PLACEMENT_3D ( 'NONE', #25114, #74872, #4817 ) ;
#50352 = DIRECTION ( 'NONE',  ( -0.000000000000000000, 1.000000000000000000, -0.000000000000000000 ) ) ;
#50353 = ORIENTED_EDGE ( 'NONE', *, *, #6157, .T. ) ;
#50354 = CARTESIAN_POINT ( 'NONE',  ( -11.25000000000000178, 2.500000000000000000, -1.572243186433546214 ) ) ;
#50355 = CARTESIAN_POINT ( 'NONE',  ( -5.650000000000019895, 2.500000000000000000, 6.148780366869520009 ) ) ;
#50356 = DIRECTION ( 'NONE',  ( 0.000000000000000000, -0.9999939076577903929, 0.003490651415223739937 ) ) ;
#50357 = CARTESIAN_POINT ( 'NONE',  ( 0.1999999999999636513, 2.500000000000000000, -0.3464101615137760715 ) ) ;
#50358 = VERTEX_POINT ( 'NONE', #55086 ) ;
#50359 = DIRECTION ( 'NONE',  ( 0.000000000000000000, -0.000000000000000000, 1.000000000000000000 ) ) ;
#50360 = EDGE_CURVE ( 'NONE', #7073, #17919, #110457, .T. ) ;
#50361 = ORIENTED_EDGE ( 'NONE', *, *, #51225, .F. ) ;
#50362 = ORIENTED_EDGE ( 'NONE', *, *, #44709, .T. ) ;
#50363 = DIRECTION ( 'NONE',  ( 0.000000000000000000, 0.000000000000000000, 1.000000000000000000 ) ) ;
#50364 = DIRECTION ( 'NONE',  ( 0.000000000000000000, 0.000000000000000000, 1.000000000000000000 ) ) ;
#50365 = FACE_BOUND ( 'NONE', #102275, .T. ) ;
#50366 = LINE ( 'NONE', #121041, #114045 ) ;
#50367 = DIRECTION ( 'NONE',  ( 0.000000000000000000, 0.000000000000000000, 1.000000000000000000 ) ) ;
#50368 = CARTESIAN_POINT ( 'NONE',  ( -14.54999999999998472, 12.50000000000000000, 2.230156782645138946 ) ) ;
#50369 = ADVANCED_FACE ( 'NONE', ( #85185 ), #14302, .T. ) ;
#50370 = AXIS2_PLACEMENT_3D ( 'NONE', #55291, #95220, #85390 ) ;
#50371 = AXIS2_PLACEMENT_3D ( 'NONE', #36159, #125795, #64949 ) ;
#50373 = AXIS2_PLACEMENT_3D ( 'NONE', #67831, #20035, #99887 ) ;
#50372 = PLANE ( 'NONE',  #37947 ) ;
#50374 = LINE ( 'NONE', #58911, #101220 ) ;
#50375 = CARTESIAN_POINT ( 'NONE',  ( -1.900000000000035438, 2.500000000000000000, 3.983716857408420076 ) ) ;
#50376 = LINE ( 'NONE', #90277, #38565 ) ;
#50377 = ORIENTED_EDGE ( 'NONE', *, *, #13107, .F. ) ;
#50378 = DIRECTION ( 'NONE',  ( 0.000000000000000000, 0.000000000000000000, 1.000000000000000000 ) ) ;
#50379 = CIRCLE ( 'NONE', #14748, 0.1000000000000002554 ) ;
#50380 = DIRECTION ( 'NONE',  ( -0.000000000000000000, -1.000000000000000000, -0.000000000000000000 ) ) ;
#50381 = EDGE_LOOP ( 'NONE', ( #27324, #70745 ) ) ;
#50382 = EDGE_LOOP ( 'NONE', ( #67833, #115546, #115079, #72814 ) ) ;
#50383 = AXIS2_PLACEMENT_3D ( 'NONE', #128039, #107752, #90026 ) ;
#50384 = FACE_OUTER_BOUND ( 'NONE', #111481, .T. ) ;
#50385 = FACE_OUTER_BOUND ( 'NONE', #43809, .T. ) ;
#50386 = FACE_BOUND ( 'NONE', #21624, .T. ) ;
#50387 = DIRECTION ( 'NONE',  ( 0.000000000000000000, 0.000000000000000000, 1.000000000000000000 ) ) ;
#50388 = PLANE ( 'NONE',  #82099 ) ;
#50389 = VERTEX_POINT ( 'NONE', #56999 ) ;
#50390 = DIRECTION ( 'NONE',  ( 0.000000000000000000, -0.000000000000000000, 1.000000000000000000 ) ) ;
#50391 = CARTESIAN_POINT ( 'NONE',  ( -3.950000000000026379, 2.500000000000000000, 2.411473670974873862 ) ) ;
#50392 = EDGE_LOOP ( 'NONE', ( #72720, #49249, #52484, #112925 ) ) ;
#50393 = CARTESIAN_POINT ( 'NONE',  ( -4.550000000000022915, 2.500000000000000000, -2.265063509461101798 ) ) ;
#50394 = CARTESIAN_POINT ( 'NONE',  ( 186.7395833340161175, 4.445597072760133273, 7.699999999999975309 ) ) ;
#50395 = EDGE_CURVE ( 'NONE', #3248, #44501, #70756, .T. ) ;
#50396 = VECTOR ( 'NONE', #107253, 1000.000000000000000 ) ;
#50397 = DIRECTION ( 'NONE',  ( 0.000000000000000000, 1.000000000000000000, 0.000000000000000000 ) ) ;
#50398 = DIRECTION ( 'NONE',  ( -0.000000000000000000, -1.000000000000000000, -0.000000000000000000 ) ) ;
#50399 = AXIS2_PLACEMENT_3D ( 'NONE', #38597, #17631, #119071 ) ;
#50400 = EDGE_CURVE ( 'NONE', #108643, #70884, #104204, .T. ) ;
#50401 = AXIS2_PLACEMENT_3D ( 'NONE', #47573, #57385, #87469 ) ;
#50402 = VERTEX_POINT ( 'NONE', #76007 ) ;
#50403 = CARTESIAN_POINT ( 'NONE',  ( 2.499999999999948930, 12.50000000000000000, -5.088040615133791356 ) ) ;
#50404 = DIRECTION ( 'NONE',  ( 0.000000000000000000, 0.000000000000000000, 1.000000000000000000 ) ) ;
#50405 = DIRECTION ( 'NONE',  ( 0.000000000000000000, -0.9999939076577903929, 0.003490651415223739937 ) ) ;
#50406 = CARTESIAN_POINT ( 'NONE',  ( 9.149999999999920419, 12.50000000000000000, 1.472243186433545459 ) ) ;
#50407 = ORIENTED_EDGE ( 'NONE', *, *, #11743, .F. ) ;
#50408 = ADVANCED_FACE ( 'NONE', ( #26277 ), #82810, .T. ) ;
#50409 = ORIENTED_EDGE ( 'NONE', *, *, #123284, .F. ) ;
#50410 = EDGE_CURVE ( 'NONE', #92182, #53057, #20659, .T. ) ;
#50411 = LINE ( 'NONE', #110621, #15810 ) ;
#50412 = AXIS2_PLACEMENT_3D ( 'NONE', #115870, #107337, #125044 ) ;
#50413 = ORIENTED_EDGE ( 'NONE', *, *, #127912, .F. ) ;
#50414 = DIRECTION ( 'NONE',  ( 0.000000000000000000, 0.000000000000000000, 1.000000000000000000 ) ) ;
#50415 = AXIS2_PLACEMENT_3D ( 'NONE', #1997, #62233, #13743 ) ;
#50416 = PLANE ( 'NONE',  #116267 ) ;
#50417 = CARTESIAN_POINT ( 'NONE',  ( -1.900000000000034994, 2.500000000000000000, -4.776537180435978414 ) ) ;
#50418 = EDGE_LOOP ( 'NONE', ( #86406, #23524, #61476, #124981 ) ) ;
#50419 = ADVANCED_FACE ( 'NONE', ( #10796 ), #64578, .T. ) ;
#50420 = LINE ( 'NONE', #70069, #53739 ) ;
#50421 = CARTESIAN_POINT ( 'NONE',  ( -3.950000000000026379, 2.500000000000000000, -1.818653347947326138 ) ) ;
#50422 = CARTESIAN_POINT ( 'NONE',  ( -5.400000000000023448, 2.500000000000000000, -4.430127018922202176 ) ) ;
#50423 = DIRECTION ( 'NONE',  ( 0.000000000000000000, -0.000000000000000000, 1.000000000000000000 ) ) ;
#50424 = DIRECTION ( 'NONE',  ( -0.000000000000000000, 1.000000000000000000, -0.000000000000000000 ) ) ;
#50425 = EDGE_CURVE ( 'NONE', #98142, #4651, #22607, .T. ) ;
#50426 = DIRECTION ( 'NONE',  ( 0.000000000000000000, 0.000000000000000000, 1.000000000000000000 ) ) ;
#50427 = AXIS2_PLACEMENT_3D ( 'NONE', #104595, #24114, #103967 ) ;
#50428 = ORIENTED_EDGE ( 'NONE', *, *, #9847, .T. ) ;
#50429 = AXIS2_PLACEMENT_3D ( 'NONE', #102385, #69691, #50081 ) ;
#50430 = ORIENTED_EDGE ( 'NONE', *, *, #7725, .T. ) ;
#50431 = CARTESIAN_POINT ( 'NONE',  ( -0.4000000000000392131, 2.500000000000000000, -4.230127018922201998 ) ) ;
#50432 = EDGE_LOOP ( 'NONE', ( #85853, #2608 ) ) ;
#50433 = CARTESIAN_POINT ( 'NONE',  ( 107.3283321151400003, 5.885277908845356620, 4.965988341037961717 ) ) ;
#50435 = ORIENTED_EDGE ( 'NONE', *, *, #56897, .T. ) ;
#50434 = EDGE_LOOP ( 'NONE', ( #42663, #76054, #76754, #46943 ) ) ;
#50436 = ORIENTED_EDGE ( 'NONE', *, *, #19385, .T. ) ;
#50437 = DIRECTION ( 'NONE',  ( -0.000000000000000000, -1.000000000000000000, -0.000000000000000000 ) ) ;
#50438 = DIRECTION ( 'NONE',  ( 0.000000000000000000, 0.000000000000000000, 1.000000000000000000 ) ) ;
#50439 = DIRECTION ( 'NONE',  ( 0.000000000000000000, 1.000000000000000000, 0.000000000000000000 ) ) ;
#50440 = SURFACE_SIDE_STYLE ('',( #70094 ) ) ;
#50441 = CARTESIAN_POINT ( 'NONE',  ( 2.899999999999945732, 12.50000000000000000, -2.385244779468109755E-15 ) ) ;
#50442 = VECTOR ( 'NONE', #12073, 1000.000000000000000 ) ;
#50443 = AXIS2_PLACEMENT_3D ( 'NONE', #113073, #33869, #94087 ) ;
#50444 = CARTESIAN_POINT ( 'NONE',  ( 11.89999999999990798, 12.50000000000000000, -4.741630453620015118 ) ) ;
#50445 = DIRECTION ( 'NONE',  ( 0.000000000000000000, 1.000000000000000000, 0.000000000000000000 ) ) ;
#50446 = CARTESIAN_POINT ( 'NONE',  ( 2.499999999999981792, 2.500000000000000000, 4.330127018922196314 ) ) ;
#50447 = CARTESIAN_POINT ( 'NONE',  ( 8.749999999999953815, 2.500000000000000000, -2.065063509461102065 ) ) ;
#50448 = FACE_OUTER_BOUND ( 'NONE', #102589, .T. ) ;
#50449 = EDGE_LOOP ( 'NONE', ( #59432, #98999 ) ) ;
#50450 = EDGE_CURVE ( 'NONE', #42165, #86633, #68789, .T. ) ;
#50451 = DIRECTION ( 'NONE',  ( 0.000000000000000000, -0.000000000000000000, 1.000000000000000000 ) ) ;
#50452 = ORIENTED_EDGE ( 'NONE', *, *, #82224, .F. ) ;
#50453 = ORIENTED_EDGE ( 'NONE', *, *, #12458, .F. ) ;
#50454 = LINE ( 'NONE', #29537, #31504 ) ;
#50455 = FACE_OUTER_BOUND ( 'NONE', #24795, .T. ) ;
#50456 = EDGE_CURVE ( 'NONE', #47635, #31556, #31159, .T. ) ;
#50457 = CARTESIAN_POINT ( 'NONE',  ( 186.9479166673494603, -6.668395609140176816, -3.850000000000003642 ) ) ;
#50458 = FACE_OUTER_BOUND ( 'NONE', #123283, .T. ) ;
#50459 = DIRECTION ( 'NONE',  ( -4.274815082592931898E-19, -0.9999939076577903929, -0.003490651415223739937 ) ) ;
#50460 = AXIS2_PLACEMENT_3D ( 'NONE', #122433, #111290, #72047 ) ;
#50461 = CARTESIAN_POINT ( 'NONE',  ( -4.550000000000026468, 2.500000000000000000, -6.495190528383302464 ) ) ;
#50462 = ORIENTED_EDGE ( 'NONE', *, *, #16740, .T. ) ;
#50463 = CONICAL_SURFACE ( 'NONE', #60930, 0.1000000000000000472, 0.003490658503988666988 ) ;
#50464 = EDGE_CURVE ( 'NONE', #4878, #85926, #33304, .T. ) ;
#50465 = CONICAL_SURFACE ( 'NONE', #87999, 0.1000000000000002554, 0.003490658503988666988 ) ;
#50466 = EDGE_CURVE ( 'NONE', #74459, #13178, #2951, .T. ) ;
#50467 = ADVANCED_FACE ( 'NONE', ( #70397 ), #52688, .T. ) ;
#50468 = VERTEX_POINT ( 'NONE', #51423 ) ;
#50469 = CARTESIAN_POINT ( 'NONE',  ( -5.650000000000019895, 2.500000000000000000, 6.741600689897071952 ) ) ;
#50470 = CONICAL_SURFACE ( 'NONE', #81762, 0.1000000000000002554, 0.003490658503988666988 ) ;
#50471 = ORIENTED_EDGE ( 'NONE', *, *, #29993, .F. ) ;
#50473 = DIRECTION ( 'NONE',  ( 0.000000000000000000, 0.000000000000000000, 1.000000000000000000 ) ) ;
#50472 = CIRCLE ( 'NONE', #85955, 0.1000000000000000056 ) ;
#50474 = EDGE_CURVE ( 'NONE', #73263, #34057, #26938, .T. ) ;
#50475 = ORIENTED_EDGE ( 'NONE', *, *, #4781, .T. ) ;
#50476 = AXIS2_PLACEMENT_3D ( 'NONE', #19196, #38227, #78805 ) ;
#50477 = ORIENTED_EDGE ( 'NONE', *, *, #114551, .F. ) ;
#50478 = CARTESIAN_POINT ( 'NONE',  ( 2.499999999999947153, 12.50000000000000000, 3.572213422710607489 ) ) ;
#50479 = DIRECTION ( 'NONE',  ( -0.000000000000000000, 1.000000000000000000, -0.000000000000000000 ) ) ;
#50480 = ADVANCED_FACE ( 'NONE', ( #92614 ), #1008, .F. ) ;
#50481 = ADVANCED_FACE ( 'NONE', ( #41602 ), #75054, .T. ) ;
#50482 = DIRECTION ( 'NONE',  ( 0.000000000000000000, -0.9999939076577903929, 0.003490651415223739937 ) ) ;
#50483 = PLANE ( 'NONE',  #77910 ) ;
#50484 = CARTESIAN_POINT ( 'NONE',  ( 17.50000000000000000, 1.666666666666665186, 4.000000000000000000 ) ) ;
#50485 = VERTEX_POINT ( 'NONE', #42236 ) ;
#50486 = DIRECTION ( 'NONE',  ( 0.000000000000000000, 1.000000000000000000, 0.000000000000000000 ) ) ;
#50487 = CARTESIAN_POINT ( 'NONE',  ( 0.7999999999999548583, 2.500000000000000000, 4.230127018922196669 ) ) ;
#50488 = CARTESIAN_POINT ( 'NONE',  ( 8.349999999999919709, 2.500000000000000000, -2.857883832488653741 ) ) ;
#50489 = DIRECTION ( 'NONE',  ( 0.000000000000000000, 1.000000000000000000, 0.000000000000000000 ) ) ;
#50490 = DIRECTION ( 'NONE',  ( 0.000000000000000000, 0.000000000000000000, 1.000000000000000000 ) ) ;
#50491 = ORIENTED_EDGE ( 'NONE', *, *, #22569, .F. ) ;
#50492 = ORIENTED_EDGE ( 'NONE', *, *, #1803, .T. ) ;
#50493 = CARTESIAN_POINT ( 'NONE',  ( -3.750000000000025757, 12.50000000000000000, -2.857883832488653741 ) ) ;
#50494 = EDGE_LOOP ( 'NONE', ( #89489, #111546 ) ) ;
#50495 = CARTESIAN_POINT ( 'NONE',  ( 14.39999999999989555, 2.500000000000000000, 0.4464101615137736623 ) ) ;
#50496 = DIRECTION ( 'NONE',  ( 0.000000000000000000, 1.000000000000000000, 0.000000000000000000 ) ) ;
#50497 = AXIS2_PLACEMENT_3D ( 'NONE', #93781, #63684, #91200 ) ;
#50498 = VERTEX_POINT ( 'NONE', #81512 ) ;
#50499 = CARTESIAN_POINT ( 'NONE',  ( 3.749999999999944045, 12.50000000000000000, -2.857883832488653741 ) ) ;
#50500 = CARTESIAN_POINT ( 'NONE',  ( -8.350000000000008527, 2.500000000000000000, 7.188010851410848723 ) ) ;
#50501 = CARTESIAN_POINT ( 'NONE',  ( 11.04999999999990656, 12.50000000000000000, 2.511473670974873507 ) ) ;
#50502 = CARTESIAN_POINT ( 'NONE',  ( -5.850000000000018296, 12.50000000000000000, 1.472243186433545459 ) ) ;
#50503 = CONICAL_SURFACE ( 'NONE', #60970, 0.1000000000000000056, 0.003490658503988666988 ) ;
#50504 = AXIS2_PLACEMENT_3D ( 'NONE', #18268, #79771, #29398 ) ;
#50505 = CARTESIAN_POINT ( 'NONE',  ( 9.799999999999917222, 2.500000000000000000, 0.2464101615137735679 ) ) ;
#50506 = AXIS2_PLACEMENT_3D ( 'NONE', #118907, #16809, #67191 ) ;
#50507 = ORIENTED_EDGE ( 'NONE', *, *, #66981, .T. ) ;
#50508 = CARTESIAN_POINT ( 'NONE',  ( 59.88498294812150391, 2.860410289928506433, -5.641291750192007903 ) ) ;
#50509 = CARTESIAN_POINT ( 'NONE',  ( 4.349999999999938360, 2.500000000000000000, 1.918653347947321564 ) ) ;
#50510 = CARTESIAN_POINT ( 'NONE',  ( -9.999999999999969802, 12.50000000000000000, 4.395220292106234439 ) ) ;
#50512 = DIRECTION ( 'NONE',  ( 0.000000000000000000, 0.000000000000000000, 1.000000000000000000 ) ) ;
#50511 = AXIS2_PLACEMENT_3D ( 'NONE', #118632, #27043, #87869 ) ;
#50513 = EDGE_CURVE ( 'NONE', #113633, #44909, #114747, .T. ) ;
#50514 = ORIENTED_EDGE ( 'NONE', *, *, #32506, .T. ) ;
#50515 = CIRCLE ( 'NONE', #67209, 0.06509327318403745899 ) ;
#50516 = EDGE_LOOP ( 'NONE', ( #53355, #41446, #101556, #92113 ) ) ;
#50517 = LINE ( 'NONE', #82581, #16599 ) ;
#50518 = DIRECTION ( 'NONE',  ( 0.000000000000000000, 0.000000000000000000, -1.000000000000000000 ) ) ;
#50519 = CIRCLE ( 'NONE', #52584, 0.09999999999999982514 ) ;
#50520 = FACE_OUTER_BOUND ( 'NONE', #60706, .T. ) ;
#50521 = ORIENTED_EDGE ( 'NONE', *, *, #71456, .T. ) ;
#50522 = CARTESIAN_POINT ( 'NONE',  ( -8.550000000000013145, 12.50000000000000000, -1.753560074763288679 ) ) ;
#50523 = CARTESIAN_POINT ( 'NONE',  ( -3.749999999999991118, 2.500000000000000000, -2.265063509461101798 ) ) ;
#50524 = AXIS2_PLACEMENT_3D ( 'NONE', #59099, #30300, #78755 ) ;
#50525 = CIRCLE ( 'NONE', #35871, 0.1000000000000002554 ) ;
#50526 = ORIENTED_EDGE ( 'NONE', *, *, #107770, .F. ) ;
#50527 = CARTESIAN_POINT ( 'NONE',  ( 6.649999999999931077, 12.50000000000000000, -6.495190528383302464 ) ) ;
#50528 = ORIENTED_EDGE ( 'NONE', *, *, #108262, .F. ) ;
#50529 = CARTESIAN_POINT ( 'NONE',  ( -8.550000000000013145, 2.500000000000000000, 2.411473670974873862 ) ) ;
#50530 = VERTEX_POINT ( 'NONE', #72347 ) ;
#50531 = CARTESIAN_POINT ( 'NONE',  ( 8.349999999999919709, 12.50000000000000000, 6.495190528383297135 ) ) ;
#50532 = CARTESIAN_POINT ( 'NONE',  ( 4.848431875627500887, 2.499999999999999112, -8.943854603337394238 ) ) ;
#50533 = ORIENTED_EDGE ( 'NONE', *, *, #41160, .F. ) ;
#50534 = ORIENTED_EDGE ( 'NONE', *, *, #106834, .F. ) ;
#50535 = DIRECTION ( 'NONE',  ( 0.000000000000000000, 1.000000000000000000, 0.000000000000000000 ) ) ;
#50536 = CARTESIAN_POINT ( 'NONE',  ( -0.6000000000000383915, 12.50000000000000000, -4.048810130592463530 ) ) ;
#50537 = EDGE_LOOP ( 'NONE', ( #66290, #96303 ) ) ;
#50538 = DIRECTION ( 'NONE',  ( 0.000000000000000000, 0.000000000000000000, 1.000000000000000000 ) ) ;
#50539 = DIRECTION ( 'NONE',  ( -4.274815082592931898E-19, -0.9999939076577903929, -0.003490651415223739937 ) ) ;
#50540 = FACE_OUTER_BOUND ( 'NONE', #91578, .T. ) ;
#50541 = AXIS2_PLACEMENT_3D ( 'NONE', #42510, #129607, #62146 ) ;
#50542 = CARTESIAN_POINT ( 'NONE',  ( 106.6791543986367259, 7.234036580820199624, 4.833745377036900770 ) ) ;
#50543 = DIRECTION ( 'NONE',  ( -0.000000000000000000, -1.000000000000000000, -0.000000000000000000 ) ) ;
#50544 = AXIS2_PLACEMENT_3D ( 'NONE', #83318, #3456, #45327 ) ;
#50545 = DIRECTION ( 'NONE',  ( 0.000000000000000000, -0.000000000000000000, 1.000000000000000000 ) ) ;
#50546 = CARTESIAN_POINT ( 'NONE',  ( -9.600000000000008527, 2.500000000000000000, 4.330127018922196314 ) ) ;
#50547 = EDGE_CURVE ( 'NONE', #117651, #51156, #99865, .T. ) ;
#50548 = CONICAL_SURFACE ( 'NONE', #69327, 0.1000000000000002554, 0.003490658503988666988 ) ;
#50549 = EDGE_LOOP ( 'NONE', ( #93270, #90848 ) ) ;
#50551 = ORIENTED_EDGE ( 'NONE', *, *, #88125, .T. ) ;
#50550 = AXIS2_PLACEMENT_3D ( 'NONE', #20021, #12743, #120147 ) ;
#50552 = EDGE_LOOP ( 'NONE', ( #99460, #8536, #9, #97259 ) ) ;
#50553 = LINE ( 'NONE', #71486, #106047 ) ;
#50554 = DIRECTION ( 'NONE',  ( 0.000000000000000000, 0.000000000000000000, -1.000000000000000000 ) ) ;
#50555 = VECTOR ( 'NONE', #72338, 1000.000000000000000 ) ;
#50556 = CARTESIAN_POINT ( 'NONE',  ( -11.69999999999999929, 2.500000000000000000, -4.330127018922198978 ) ) ;
#50559 = ORIENTED_EDGE ( 'NONE', *, *, #14551, .T. ) ;
#50558 = ORIENTED_EDGE ( 'NONE', *, *, #13938, .F. ) ;
#50557 = AXIS2_PLACEMENT_3D ( 'NONE', #17823, #26375, #65638 ) ;
#50560 = EDGE_CURVE ( 'NONE', #12189, #68896, #29102, .T. ) ;
#50561 = FACE_BOUND ( 'NONE', #95853, .T. ) ;
#50562 = ORIENTED_EDGE ( 'NONE', *, *, #98320, .F. ) ;
#50563 = EDGE_CURVE ( 'NONE', #10632, #26142, #120780, .T. ) ;
#50564 = CARTESIAN_POINT ( 'NONE',  ( 6.849999999999929479, 2.500000000000000000, 6.841600689897072485 ) ) ;
#50565 = DIRECTION ( 'NONE',  ( 0.000000000000000000, 0.000000000000000000, -1.000000000000000000 ) ) ;
#50566 = AXIS2_PLACEMENT_3D ( 'NONE', #127362, #28515, #39007 ) ;
#50567 = DIRECTION ( 'NONE',  ( 0.000000000000000000, 0.000000000000000000, 1.000000000000000000 ) ) ;
#50568 = DIRECTION ( 'NONE',  ( -0.000000000000000000, 1.000000000000000000, -0.000000000000000000 ) ) ;
#50569 = CARTESIAN_POINT ( 'NONE',  ( -3.350000000000028955, 12.50000000000000000, 7.188010851410848723 ) ) ;
#50570 = CARTESIAN_POINT ( 'NONE',  ( 13.94999999999989804, 12.50000000000000000, 1.818653347947321475 ) ) ;
#50571 = ADVANCED_FACE ( 'NONE', ( #21287 ), #6074, .T. ) ;
#50572 = DIRECTION ( 'NONE',  ( 0.000000000000000000, 1.000000000000000000, 0.000000000000000000 ) ) ;
#50573 = EDGE_CURVE ( 'NONE', #39206, #28200, #125226, .T. ) ;
#50574 = CARTESIAN_POINT ( 'NONE',  ( -3.350000000000028511, 2.500000000000000000, 1.572243186433545548 ) ) ;
#50575 = ADVANCED_FACE ( 'NONE', ( #94537 ), #110551, .T. ) ;
#50576 = CARTESIAN_POINT ( 'NONE',  ( -6.250000000000019540, 12.50000000000000000, -2.857883832488653741 ) ) ;
#50577 = EDGE_CURVE ( 'NONE', #120557, #112512, #72996, .T. ) ;
#50578 = CARTESIAN_POINT ( 'NONE',  ( 10.19999999999991225, 12.50000000000000000, 3.983716857408420076 ) ) ;
#50579 = EDGE_LOOP ( 'NONE', ( #115909, #103982, #21186, #112766 ) ) ;
#50580 = VERTEX_POINT ( 'NONE', #54601 ) ;
#50581 = VERTEX_POINT ( 'NONE', #85989 ) ;
#50582 = ORIENTED_EDGE ( 'NONE', *, *, #12190, .T. ) ;
#50583 = DIRECTION ( 'NONE',  ( 0.000000000000000000, -0.9999939076577903929, 0.003490651415223739937 ) ) ;
#50584 = FACE_OUTER_BOUND ( 'NONE', #78125, .T. ) ;
#50586 = VERTEX_POINT ( 'NONE', #33071 ) ;
#50585 = ORIENTED_EDGE ( 'NONE', *, *, #11565, .F. ) ;
#50587 = VERTEX_POINT ( 'NONE', #95839 ) ;
#50588 = CARTESIAN_POINT ( 'NONE',  ( -6.050000000000020250, 2.500000000000000000, -2.411473670974877859 ) ) ;
#50589 = VECTOR ( 'NONE', #51931, 1000.000000000000000 ) ;
#50590 = CARTESIAN_POINT ( 'NONE',  ( 3.099999999999944134, 2.500000000000000000, 4.676537180435972552 ) ) ;
#50591 = DIRECTION ( 'NONE',  ( 0.000000000000000000, 0.000000000000000000, -1.000000000000000000 ) ) ;
#50592 = CARTESIAN_POINT ( 'NONE',  ( 13.74999999999989697, 12.50000000000000000, 2.857883832488649301 ) ) ;
#50593 = DIRECTION ( 'NONE',  ( 0.000000000000000000, 0.000000000000000000, 1.000000000000000000 ) ) ;
#50594 = CARTESIAN_POINT ( 'NONE',  ( 5.649999999999934630, 2.500000000000000000, -1.818653347947325916 ) ) ;
#50595 = DIRECTION ( 'NONE',  ( -4.274815082592931898E-19, -0.9999939076577903929, -0.003490651415223739937 ) ) ;
#50596 = VERTEX_POINT ( 'NONE', #74912 ) ;
#50597 = CIRCLE ( 'NONE', #125798, 0.09999999999999982514 ) ;
#50598 = CIRCLE ( 'NONE', #58925, 0.1000000000000002554 ) ;
#50599 = CARTESIAN_POINT ( 'NONE',  ( 13.34999999999989662, 2.500000000000000000, -2.757883832488654097 ) ) ;
#50600 = ORIENTED_EDGE ( 'NONE', *, *, #41208, .T. ) ;
#50601 = VECTOR ( 'NONE', #20383, 1000.000000000000000 ) ;
#50602 = ORIENTED_EDGE ( 'NONE', *, *, #81991, .F. ) ;
#50603 = CIRCLE ( 'NONE', #71533, 0.09999999999999982514 ) ;
#50604 = ORIENTED_EDGE ( 'NONE', *, *, #65044, .T. ) ;
#50605 = DIRECTION ( 'NONE',  ( 0.000000000000000000, -0.9999939076577903929, 0.003490651415223739937 ) ) ;
#50606 = EDGE_CURVE ( 'NONE', #38108, #68087, #4859, .T. ) ;
#50607 = ORIENTED_EDGE ( 'NONE', *, *, #96693, .T. ) ;
#50608 = ORIENTED_EDGE ( 'NONE', *, *, #10873, .F. ) ;
#50609 = FACE_OUTER_BOUND ( 'NONE', #83901, .T. ) ;
#50610 = AXIS2_PLACEMENT_3D ( 'NONE', #32218, #2073, #69530 ) ;
#50611 = LINE ( 'NONE', #80739, #127033 ) ;
#50612 = CARTESIAN_POINT ( 'NONE',  ( 3.749999999999942268, 2.500000000000000000, -1.572243186433550211 ) ) ;
#50613 = DIRECTION ( 'NONE',  ( 0.000000000000000000, 1.000000000000000000, 0.000000000000000000 ) ) ;
#50614 = CIRCLE ( 'NONE', #92370, 0.09999999999999999167 ) ;
#50615 = DIRECTION ( 'NONE',  ( -0.000000000000000000, 1.000000000000000000, -0.000000000000000000 ) ) ;
#50616 = CIRCLE ( 'NONE', #52675, 0.06509327318403745899 ) ;
#50617 = AXIS2_PLACEMENT_3D ( 'NONE', #26289, #5339, #85195 ) ;
#50618 = EDGE_CURVE ( 'NONE', #52298, #89250, #4212, .T. ) ;
#50619 = CARTESIAN_POINT ( 'NONE',  ( 10.39999999999991154, 2.500000000000000000, -5.122947341949753763 ) ) ;
#50620 = EDGE_CURVE ( 'NONE', #98964, #129208, #77110, .T. ) ;
#50621 = CONICAL_SURFACE ( 'NONE', #75747, 0.1000000000000002554, 0.003490658503988666988 ) ;
#50622 = EDGE_CURVE ( 'NONE', #69752, #18522, #23215, .T. ) ;
#50623 = CARTESIAN_POINT ( 'NONE',  ( -11.64999999999999680, 2.500000000000000000, -6.595190528383298556 ) ) ;
#50624 = EDGE_LOOP ( 'NONE', ( #4245, #83910, #91210, #28473 ) ) ;
#50626 = EDGE_CURVE ( 'NONE', #122009, #78632, #1882, .T. ) ;
#50625 = CARTESIAN_POINT ( 'NONE',  ( 21.24748442509683244, -0.7426088330904641044, 4.181982359507943947 ) ) ;
#50627 = ORIENTED_EDGE ( 'NONE', *, *, #44074, .F. ) ;
#50628 = CARTESIAN_POINT ( 'NONE',  ( 112.8677677318791979, 8.624640698664421734, 1.154296164367282218 ) ) ;
#50629 = VECTOR ( 'NONE', #5, 1000.000000000000000 ) ;
#50630 = CARTESIAN_POINT ( 'NONE',  ( -9.800000000000004263, 2.500000000000000000, 4.083716857408420609 ) ) ;
#50632 = ORIENTED_EDGE ( 'NONE', *, *, #95252, .F. ) ;
#50631 = ADVANCED_FACE ( 'NONE', ( #55903 ), #49941, .T. ) ;
#50633 = DIRECTION ( 'NONE',  ( 0.000000000000000000, 0.000000000000000000, 1.000000000000000000 ) ) ;
#50634 = EDGE_CURVE ( 'NONE', #8778, #58319, #123174, .T. ) ;
#50635 = DIRECTION ( 'NONE',  ( 0.000000000000000000, 0.000000000000000000, -1.000000000000000000 ) ) ;
#50636 = ORIENTED_EDGE ( 'NONE', *, *, #58041, .F. ) ;
#50637 = EDGE_CURVE ( 'NONE', #33308, #118779, #47878, .T. ) ;
#50638 = EDGE_CURVE ( 'NONE', #99278, #84066, #3941, .T. ) ;
#50639 = EDGE_CURVE ( 'NONE', #89885, #90718, #118960, .T. ) ;
#50640 = CARTESIAN_POINT ( 'NONE',  ( -0.8500000000000382805, 2.500000000000000000, -1.472243186433550122 ) ) ;
#50641 = ORIENTED_EDGE ( 'NONE', *, *, #9115, .T. ) ;
#50642 = ORIENTED_EDGE ( 'NONE', *, *, #91346, .F. ) ;
#50643 = DIRECTION ( 'NONE',  ( -0.000000000000000000, -1.000000000000000000, -0.000000000000000000 ) ) ;
#50644 = CARTESIAN_POINT ( 'NONE',  ( 11.44999999999990514, 12.50000000000000000, -6.148780366869526226 ) ) ;
#50645 = CARTESIAN_POINT ( 'NONE',  ( 9.349999999999919709, 2.500000000000000000, -6.048780366869526581 ) ) ;
#50646 = LINE ( 'NONE', #61110, #93154 ) ;
#50647 = EDGE_CURVE ( 'NONE', #52447, #6702, #37413, .T. ) ;
#50648 = LINE ( 'NONE', #101040, #56204 ) ;
#50649 = EDGE_LOOP ( 'NONE', ( #76413, #75055, #45119, #55080 ) ) ;
#50650 = DIRECTION ( 'NONE',  ( 0.000000000000000000, -0.9999939076577903929, 0.003490651415223739937 ) ) ;
#50651 = CIRCLE ( 'NONE', #98658, 0.09999999999999999167 ) ;
#50652 = AXIS2_PLACEMENT_3D ( 'NONE', #107507, #95756, #17828 ) ;
#50653 = AXIS2_PLACEMENT_3D ( 'NONE', #16473, #28906, #77352 ) ;
#50654 = EDGE_LOOP ( 'NONE', ( #87787, #77938, #84222, #121808 ) ) ;
#50655 = LINE ( 'NONE', #109588, #25653 ) ;
#50656 = CARTESIAN_POINT ( 'NONE',  ( -8.100000000000013856, 2.500000000000000000, -0.2464101615137782308 ) ) ;
#50657 = AXIS2_PLACEMENT_3D ( 'NONE', #24772, #64682, #126184 ) ;
#50658 = CIRCLE ( 'NONE', #71480, 0.06509327318403745899 ) ;
#50659 = AXIS2_PLACEMENT_3D ( 'NONE', #77964, #68138, #98892 ) ;
#50660 = AXIS2_PLACEMENT_3D ( 'NONE', #24513, #75525, #84716 ) ;
#50661 = CONICAL_SURFACE ( 'NONE', #96611, 0.1000000000000002554, 0.003490658503988666988 ) ;
#50662 = CARTESIAN_POINT ( 'NONE',  ( 186.0468750003414300, -8.734944146203032389, -1.604583208406768146E-15 ) ) ;
#50663 = DIRECTION ( 'NONE',  ( 0.000000000000000000, 0.000000000000000000, -1.000000000000000000 ) ) ;
#50664 = FACE_OUTER_BOUND ( 'NONE', #82553, .T. ) ;
#50665 = DIRECTION ( 'NONE',  ( -0.000000000000000000, -1.000000000000000000, -0.000000000000000000 ) ) ;
#50666 = CARTESIAN_POINT ( 'NONE',  ( 6.849999999999930367, 2.500000000000000000, -6.841600689897078702 ) ) ;
#50667 = VERTEX_POINT ( 'NONE', #23888 ) ;
#50668 = DIRECTION ( 'NONE',  ( -0.000000000000000000, 1.000000000000000000, -0.000000000000000000 ) ) ;
#50669 = CARTESIAN_POINT ( 'NONE',  ( 6.699999999999930012, 12.50000000000000000, -4.265033745738164406 ) ) ;
#50670 = DIRECTION ( 'NONE',  ( 0.000000000000000000, 0.000000000000000000, -1.000000000000000000 ) ) ;
#50671 = ORIENTED_EDGE ( 'NONE', *, *, #76302, .T. ) ;
#50672 = DIRECTION ( 'NONE',  ( 0.000000000000000000, 0.000000000000000000, -1.000000000000000000 ) ) ;
#50673 = AXIS2_PLACEMENT_3D ( 'NONE', #105073, #72419, #5578 ) ;
#50674 = EDGE_CURVE ( 'NONE', #79091, #57186, #127292, .T. ) ;
#50675 = ORIENTED_EDGE ( 'NONE', *, *, #91149, .F. ) ;
#50676 = EDGE_LOOP ( 'NONE', ( #37301, #65209, #9219, #85370 ) ) ;
#50677 = CARTESIAN_POINT ( 'NONE',  ( 3.349999999999942801, 2.500000000000000000, 2.757883832488649656 ) ) ;
#50678 = ORIENTED_EDGE ( 'NONE', *, *, #36751, .T. ) ;
#50679 = DIRECTION ( 'NONE',  ( 0.000000000000000000, 1.000000000000000000, 0.000000000000000000 ) ) ;
#50680 = DIRECTION ( 'NONE',  ( 0.000000000000000000, 0.000000000000000000, -1.000000000000000000 ) ) ;
#50681 = VECTOR ( 'NONE', #78203, 1000.000000000000000 ) ;
#50682 = ORIENTED_EDGE ( 'NONE', *, *, #1976, .F. ) ;
#50683 = CONICAL_SURFACE ( 'NONE', #25846, 0.1000000000000002554, 0.003490658503988666988 ) ;
#50684 = CARTESIAN_POINT ( 'NONE',  ( -6.250000000000021316, 2.500000000000000000, -1.472243186433550122 ) ) ;
#50685 = DIRECTION ( 'NONE',  ( -0.000000000000000000, 1.000000000000000000, -0.000000000000000000 ) ) ;
#50686 = LINE ( 'NONE', #36706, #107215 ) ;
#50687 = EDGE_CURVE ( 'NONE', #82670, #85004, #83375, .T. ) ;
#50688 = VECTOR ( 'NONE', #33777, 1000.000000000000000 ) ;
#50689 = VERTEX_POINT ( 'NONE', #5501 ) ;
#50690 = AXIS2_PLACEMENT_3D ( 'NONE', #40163, #11340, #80736 ) ;
#50691 = AXIS2_PLACEMENT_3D ( 'NONE', #33533, #83894, #114644 ) ;
#50692 = VECTOR ( 'NONE', #125979, 1000.000000000000000 ) ;
#50693 = ORIENTED_EDGE ( 'NONE', *, *, #75452, .T. ) ;
#50694 = ORIENTED_EDGE ( 'NONE', *, *, #95561, .T. ) ;
#50695 = DIRECTION ( 'NONE',  ( 0.000000000000000000, 0.000000000000000000, 1.000000000000000000 ) ) ;
#50696 = DIRECTION ( 'NONE',  ( 0.000000000000000000, 0.000000000000000000, -1.000000000000000000 ) ) ;
#50697 = CARTESIAN_POINT ( 'NONE',  ( -10.20000000000000284, 2.500000000000000000, 3.883716857408421319 ) ) ;
#50698 = FACE_BOUND ( 'NONE', #111592, .T. ) ;
#50699 = ORIENTED_EDGE ( 'NONE', *, *, #17137, .F. ) ;
#50700 = FACE_OUTER_BOUND ( 'NONE', #4865, .T. ) ;
#50701 = CARTESIAN_POINT ( 'NONE',  ( 15.59999999999988951, 2.500000000000000000, 0.2464101615137735679 ) ) ;
#50702 = AXIS2_PLACEMENT_3D ( 'NONE', #121042, #22223, #103350 ) ;
#50703 = EDGE_LOOP ( 'NONE', ( #27466, #84094 ) ) ;
#50704 = CONICAL_SURFACE ( 'NONE', #517, 0.1000000000000002554, 0.003490658503988666988 ) ;
#50705 = CARTESIAN_POINT ( 'NONE',  ( -12.89999999999999325, 2.500000000000000000, -3.637306695894647390 ) ) ;
#50706 = CARTESIAN_POINT ( 'NONE',  ( -10.20000000000000462, 12.50000000000000000, 4.741630453620009789 ) ) ;
#50707 = AXIS2_PLACEMENT_3D ( 'NONE', #7129, #74600, #66701 ) ;
#50708 = AXIS2_PLACEMENT_3D ( 'NONE', #33415, #124996, #83155 ) ;
#50709 = VECTOR ( 'NONE', #61551, 1000.000000000000000 ) ;
#50710 = CARTESIAN_POINT ( 'NONE',  ( -0.4000000000000404898, 2.500000000000000000, 5.022947341949748790 ) ) ;
#50711 = FACE_OUTER_BOUND ( 'NONE', #13881, .T. ) ;
#50712 = DIRECTION ( 'NONE',  ( 0.000000000000000000, 0.000000000000000000, 1.000000000000000000 ) ) ;
#50713 = CARTESIAN_POINT ( 'NONE',  ( -6.650000000000019007, 2.500000000000000000, -1.472243186433550122 ) ) ;
#50714 = CIRCLE ( 'NONE', #96665, 0.1000000000000002554 ) ;
#50715 = LINE ( 'NONE', #88707, #12680 ) ;
#50716 = ADVANCED_FACE ( 'NONE', ( #74266 ), #105662, .T. ) ;
#50717 = ORIENTED_EDGE ( 'NONE', *, *, #72716, .T. ) ;
#50718 = AXIS2_PLACEMENT_3D ( 'NONE', #111234, #22254, #1298 ) ;
#50719 = ORIENTED_EDGE ( 'NONE', *, *, #3601, .T. ) ;
#50720 = ORIENTED_EDGE ( 'NONE', *, *, #8733, .T. ) ;
#50721 = EDGE_LOOP ( 'NONE', ( #123987, #39472, #94502, #94841 ) ) ;
#50722 = CARTESIAN_POINT ( 'NONE',  ( 88.00000000000001421, 0.000000000000000000, 8.699999999999999289 ) ) ;
#50723 = DIRECTION ( 'NONE',  ( 0.000000000000000000, 0.000000000000000000, 1.000000000000000000 ) ) ;
#50724 = ORIENTED_EDGE ( 'NONE', *, *, #49406, .T. ) ;
#50725 = FACE_BOUND ( 'NONE', #48301, .T. ) ;
#50726 = EDGE_CURVE ( 'NONE', #72665, #12542, #75533, .T. ) ;
#50727 = CARTESIAN_POINT ( 'NONE',  ( 0.3999999999999559464, 2.500000000000000000, -4.430127018922202176 ) ) ;
#50728 = CARTESIAN_POINT ( 'NONE',  ( -4.400000000000028777, 2.500000000000000000, -3.883716857408426648 ) ) ;
#50729 = CARTESIAN_POINT ( 'NONE',  ( -6.700000000000019718, 2.500000000000000000, -4.430127018922202176 ) ) ;
#50730 = DIRECTION ( 'NONE',  ( -0.000000000000000000, -1.000000000000000000, -0.000000000000000000 ) ) ;
#50731 = EDGE_CURVE ( 'NONE', #1776, #8661, #70844, .T. ) ;
#50732 = DIRECTION ( 'NONE',  ( 0.000000000000000000, 0.000000000000000000, 1.000000000000000000 ) ) ;
#50733 = EDGE_CURVE ( 'NONE', #118880, #104652, #75142, .T. ) ;
#50734 = LINE ( 'NONE', #21266, #97737 ) ;
#50735 = CARTESIAN_POINT ( 'NONE',  ( -5.600000000000020073, 12.50000000000000000, 0.4115034346978110880 ) ) ;
#50736 = CONICAL_SURFACE ( 'NONE', #119982, 0.1000000000000002554, 0.003490658503988666988 ) ;
#50737 = ADVANCED_FACE ( 'NONE', ( #57199 ), #100192, .T. ) ;
#50738 = DIRECTION ( 'NONE',  ( -0.000000000000000000, -1.000000000000000000, -0.000000000000000000 ) ) ;
#50739 = ADVANCED_FACE ( 'NONE', ( #68297 ), #99066, .T. ) ;
#50740 = EDGE_LOOP ( 'NONE', ( #112354, #78034, #29935, #95284, #41915, #24794, #14228, #9087 ) ) ;
#50741 = EDGE_CURVE ( 'NONE', #99983, #120284, #10301, .T. ) ;
#50742 = EDGE_LOOP ( 'NONE', ( #17426, #60129 ) ) ;
#50743 = VERTEX_POINT ( 'NONE', #117373 ) ;
#50744 = VERTEX_POINT ( 'NONE', #68949 ) ;
#50745 = EDGE_LOOP ( 'NONE', ( #1606, #33817 ) ) ;
#50746 = CONICAL_SURFACE ( 'NONE', #121742, 0.1000000000000000472, 0.003490658503988666988 ) ;
#50747 = VERTEX_POINT ( 'NONE', #97122 ) ;
#50748 = VECTOR ( 'NONE', #11128, 1000.000000000000000 ) ;
#50749 = CIRCLE ( 'NONE', #123891, 0.09999999999999982514 ) ;
#50750 = DIRECTION ( 'NONE',  ( 0.000000000000000000, 1.000000000000000000, 0.000000000000000000 ) ) ;
#50751 = VERTEX_POINT ( 'NONE', #49339 ) ;
#50752 = ADVANCED_FACE ( 'NONE', ( #87923 ), #58431, .T. ) ;
#50753 = EDGE_CURVE ( 'NONE', #63286, #35370, #37502, .T. ) ;
#50755 = EDGE_CURVE ( 'NONE', #110598, #18873, #27099, .T. ) ;
#50754 = AXIS2_PLACEMENT_3D ( 'NONE', #51126, #122436, #112614 ) ;
#50756 = CIRCLE ( 'NONE', #40299, 0.09999999999999982514 ) ;
#50757 = CARTESIAN_POINT ( 'NONE',  ( -2.900000000000030553, 2.500000000000000000, 5.022947341949748790 ) ) ;
#50758 = CARTESIAN_POINT ( 'NONE',  ( 185.4427083336747160, -6.551208109652278289, 3.782341765624995134 ) ) ;
#50759 = DIRECTION ( 'NONE',  ( -0.000000000000000000, 1.000000000000000000, -0.000000000000000000 ) ) ;
#50760 = CARTESIAN_POINT ( 'NONE',  ( 5.399999999999934630, 2.500000000000000000, 0.6928203230275494784 ) ) ;
#50761 = CIRCLE ( 'NONE', #21513, 0.1000000000000002554 ) ;
#50762 = CIRCLE ( 'NONE', #71685, 1.000000000000000444 ) ;
#50763 = AXIS2_PLACEMENT_3D ( 'NONE', #78798, #47392, #15484 ) ;
#50764 = EDGE_LOOP ( 'NONE', ( #126586, #78355, #57902, #94204 ) ) ;
#50765 = CARTESIAN_POINT ( 'NONE',  ( -11.25000000000000000, 2.500000000000000000, -7.188010851410850499 ) ) ;
#50766 = AXIS2_PLACEMENT_3D ( 'NONE', #82860, #10849, #91370 ) ;
#50767 = EDGE_LOOP ( 'NONE', ( #111502, #52046 ) ) ;
#50768 = VERTEX_POINT ( 'NONE', #67001 ) ;
#50769 = CARTESIAN_POINT ( 'NONE',  ( 5.849999999999933920, 2.500000000000000000, -2.957883832488653830 ) ) ;
#50770 = CARTESIAN_POINT ( 'NONE',  ( -0.6000000000000388356, 12.50000000000000000, 3.983716857408420964 ) ) ;
#50771 = DIRECTION ( 'NONE',  ( 0.000000000000000000, 0.000000000000000000, 1.000000000000000000 ) ) ;
#50772 = ORIENTED_EDGE ( 'NONE', *, *, #59941, .F. ) ;
#50773 = ORIENTED_EDGE ( 'NONE', *, *, #32349, .T. ) ;
#50774 = AXIS2_PLACEMENT_3D ( 'NONE', #31069, #70968, #21217 ) ;
#50775 = DIRECTION ( 'NONE',  ( -4.274815082592931898E-19, -0.9999939076577903929, -0.003490651415223739937 ) ) ;
#50776 = DIRECTION ( 'NONE',  ( -0.000000000000000000, -1.000000000000000000, -0.000000000000000000 ) ) ;
#50777 = DIRECTION ( 'NONE',  ( 0.000000000000000000, 0.000000000000000000, 1.000000000000000000 ) ) ;
#50778 = CARTESIAN_POINT ( 'NONE',  ( 10.84999999999990905, 2.500000000000000000, 2.065063509461097624 ) ) ;
#50779 = VERTEX_POINT ( 'NONE', #128549 ) ;
#50780 = LINE ( 'NONE', #71704, #77384 ) ;
#50782 = ORIENTED_EDGE ( 'NONE', *, *, #79007, .F. ) ;
#50781 = AXIS2_PLACEMENT_3D ( 'NONE', #124569, #85273, #76751 ) ;
#50783 = DIRECTION ( 'NONE',  ( 0.000000000000000000, 0.000000000000000000, 1.000000000000000000 ) ) ;
#50784 = CIRCLE ( 'NONE', #42379, 0.06509327318403745899 ) ;
#50785 = AXIS2_PLACEMENT_3D ( 'NONE', #54641, #23919, #65755 ) ;
#50786 = ORIENTED_EDGE ( 'NONE', *, *, #13769, .T. ) ;
#50787 = DIRECTION ( 'NONE',  ( 0.000000000000000000, 0.000000000000000000, -1.000000000000000000 ) ) ;
#50788 = DIRECTION ( 'NONE',  ( 0.000000000000000000, 0.000000000000000000, -1.000000000000000000 ) ) ;
#50789 = CARTESIAN_POINT ( 'NONE',  ( -4.150000000000025224, 12.50000000000000000, 2.922977105672686982 ) ) ;
#50790 = EDGE_CURVE ( 'NONE', #71326, #122362, #38885, .T. ) ;
#50792 = VECTOR ( 'NONE', #55680, 1000.000000000000000 ) ;
#50791 = DIRECTION ( 'NONE',  ( -0.000000000000000000, -1.000000000000000000, -0.000000000000000000 ) ) ;
#50793 = VERTEX_POINT ( 'NONE', #76202 ) ;
#50794 = CIRCLE ( 'NONE', #6843, 0.06509327318403745899 ) ;
#50795 = EDGE_CURVE ( 'NONE', #110101, #32791, #116113, .T. ) ;
#50796 = VECTOR ( 'NONE', #11124, 1000.000000000000000 ) ;
#50797 = DIRECTION ( 'NONE',  ( -4.274815082592931898E-19, -0.9999939076577903929, -0.003490651415223739937 ) ) ;
#50798 = CONICAL_SURFACE ( 'NONE', #36225, 0.1000000000000002554, 0.003490658503988666988 ) ;
#50799 = ADVANCED_FACE ( 'NONE', ( #37572 ), #18562, .T. ) ;
#50800 = CARTESIAN_POINT ( 'NONE',  ( 8.149999999999920419, 2.500000000000000000, 6.148780366869520897 ) ) ;
#50801 = ORIENTED_EDGE ( 'NONE', *, *, #49597, .T. ) ;
#50802 = ORIENTED_EDGE ( 'NONE', *, *, #103649, .T. ) ;
#50803 = ORIENTED_EDGE ( 'NONE', *, *, #100077, .T. ) ;
#50804 = CARTESIAN_POINT ( 'NONE',  ( -2.700000000000029932, 12.50000000000000000, -0.4115034346978156399 ) ) ;
#50805 = CARTESIAN_POINT ( 'NONE',  ( 6.049999999999934097, 2.500000000000000000, 6.248780366869521430 ) ) ;
#50806 = DIRECTION ( 'NONE',  ( -0.000000000000000000, 1.000000000000000000, -0.000000000000000000 ) ) ;
#50807 = CONICAL_SURFACE ( 'NONE', #48753, 0.09999999999999982514, 0.003490658503988666988 ) ;
#50808 = LINE ( 'NONE', #20703, #55310 ) ;
#50809 = EDGE_CURVE ( 'NONE', #114240, #78540, #98119, .T. ) ;
#50810 = DIRECTION ( 'NONE',  ( 0.000000000000000000, 0.000000000000000000, -1.000000000000000000 ) ) ;
#50811 = AXIS2_PLACEMENT_3D ( 'NONE', #26669, #106509, #78356 ) ;
#50812 = CARTESIAN_POINT ( 'NONE',  ( -12.49999999999995914, 2.500000000000000000, -4.230127018922199333 ) ) ;
#50813 = CIRCLE ( 'NONE', #111425, 0.1000000000000002554 ) ;
#50814 = DIRECTION ( 'NONE',  ( 0.000000000000000000, -0.000000000000000000, 1.000000000000000000 ) ) ;
#50815 = AXIS2_PLACEMENT_3D ( 'NONE', #126292, #26796, #66707 ) ;
#50816 = AXIS2_PLACEMENT_3D ( 'NONE', #78469, #98079, #126908 ) ;
#50817 = DIRECTION ( 'NONE',  ( 0.000000000000000000, 0.000000000000000000, 1.000000000000000000 ) ) ;
#50818 = AXIS2_PLACEMENT_3D ( 'NONE', #71175, #111077, #41744 ) ;
#50819 = EDGE_LOOP ( 'NONE', ( #89270, #67018 ) ) ;
#50820 = CARTESIAN_POINT ( 'NONE',  ( -2.900000000000029221, 2.500000000000000000, 0.09999999999999772959 ) ) ;
#50821 = DIRECTION ( 'NONE',  ( 0.000000000000000000, 0.000000000000000000, -1.000000000000000000 ) ) ;
#50822 = ADVANCED_FACE ( 'NONE', ( #108229 ), #39665, .T. ) ;
#50823 = CARTESIAN_POINT ( 'NONE',  ( 12.09999999999990550, 2.500000000000000000, 3.737306695894644371 ) ) ;
#50824 = CARTESIAN_POINT ( 'NONE',  ( 2.049999999999950084, 12.50000000000000000, 2.165063509461097713 ) ) ;
#50825 = EDGE_LOOP ( 'NONE', ( #66153, #64028 ) ) ;
#50826 = CARTESIAN_POINT ( 'NONE',  ( 10.39999999999991509, 2.500000000000000000, -0.6928203230275542523 ) ) ;
#50827 = LINE ( 'NONE', #51480, #36557 ) ;
#50829 = EDGE_LOOP ( 'NONE', ( #33905, #104539, #97309, #24364 ) ) ;
#50828 = DIRECTION ( 'NONE',  ( 0.000000000000000000, 0.000000000000000000, 1.000000000000000000 ) ) ;
#50830 = CONICAL_SURFACE ( 'NONE', #17447, 0.09999999999999982514, 0.003490658503988666988 ) ;
#50831 = ORIENTED_EDGE ( 'NONE', *, *, #57877, .T. ) ;
#50832 = DIRECTION ( 'NONE',  ( 0.000000000000000000, 0.000000000000000000, 1.000000000000000000 ) ) ;
#50833 = VECTOR ( 'NONE', #34434, 1000.000000000000000 ) ;
#50834 = EDGE_CURVE ( 'NONE', #65564, #102028, #46740, .T. ) ;
#50835 = ORIENTED_EDGE ( 'NONE', *, *, #94932, .T. ) ;
#50836 = AXIS2_PLACEMENT_3D ( 'NONE', #1927, #30777, #110599 ) ;
#50837 = VERTEX_POINT ( 'NONE', #88595 ) ;
#50838 = DIRECTION ( 'NONE',  ( 0.000000000000000000, 0.000000000000000000, 1.000000000000000000 ) ) ;
#50839 = AXIS2_PLACEMENT_3D ( 'NONE', #52210, #122888, #123510 ) ;
#50840 = CIRCLE ( 'NONE', #34118, 0.1000000000000002554 ) ;
#50841 = DIRECTION ( 'NONE',  ( 0.000000000000000000, 0.000000000000000000, 1.000000000000000000 ) ) ;
#50842 = LINE ( 'NONE', #31851, #63048 ) ;
#50843 = CYLINDRICAL_SURFACE ( 'NONE', #123196, 5.200000000000000178 ) ;
#50845 = ORIENTED_EDGE ( 'NONE', *, *, #65381, .F. ) ;
#50844 = AXIS2_PLACEMENT_3D ( 'NONE', #68848, #118584, #27616 ) ;
#50846 = CIRCLE ( 'NONE', #11109, 0.06509327318403745899 ) ;
#50847 = AXIS2_PLACEMENT_3D ( 'NONE', #49386, #89289, #80117 ) ;
#50848 = PLANE ( 'NONE',  #25186 ) ;
#50850 = ORIENTED_EDGE ( 'NONE', *, *, #39109, .T. ) ;
#50849 = CIRCLE ( 'NONE', #88487, 0.06509327318403745899 ) ;
#50851 = AXIS2_PLACEMENT_3D ( 'NONE', #108736, #59004, #98925 ) ;
#50852 = DIRECTION ( 'NONE',  ( 0.000000000000000000, 0.000000000000000000, 1.000000000000000000 ) ) ;
#50853 = EDGE_CURVE ( 'NONE', #54395, #87768, #22923, .T. ) ;
#50854 = CARTESIAN_POINT ( 'NONE',  ( 17.01005371150556655, -1.931450858213975774, 5.528361852685534039 ) ) ;
#50855 = CIRCLE ( 'NONE', #36199, 0.06509327318403745899 ) ;
#50856 = ORIENTED_EDGE ( 'NONE', *, *, #16417, .F. ) ;
#50857 = ORIENTED_EDGE ( 'NONE', *, *, #84894, .F. ) ;
#50858 = ORIENTED_EDGE ( 'NONE', *, *, #99656, .T. ) ;
#50859 = EDGE_LOOP ( 'NONE', ( #32205, #76214 ) ) ;
#50860 = DIRECTION ( 'NONE',  ( -0.000000000000000000, -1.000000000000000000, -0.000000000000000000 ) ) ;
#50861 = CARTESIAN_POINT ( 'NONE',  ( 14.66596005923860702, 1.500000000000160538, 7.515560522276493849 ) ) ;
#50862 = LINE ( 'NONE', #12206, #27438 ) ;
#50863 = FACE_BOUND ( 'NONE', #122431, .T. ) ;
#50864 = LINE ( 'NONE', #95136, #20229 ) ;
#50865 = CARTESIAN_POINT ( 'NONE',  ( 185.9062500006828316, -8.891194145520236347, -1.633285867636356693E-15 ) ) ;
#50866 = LINE ( 'NONE', #61333, #113789 ) ;
#50867 = DIRECTION ( 'NONE',  ( 0.000000000000000000, -0.9999939076577903929, 0.003490651415223739937 ) ) ;
#50868 = AXIS2_PLACEMENT_3D ( 'NONE', #47963, #96389, #127798 ) ;
#50869 = CARTESIAN_POINT ( 'NONE',  ( 3.099999999999945466, 2.500000000000000000, 0.3464101615137735735 ) ) ;
#50870 = CARTESIAN_POINT ( 'NONE',  ( 4.149999999999941735, 2.500000000000000000, -2.857883832488653741 ) ) ;
#50871 = DIRECTION ( 'NONE',  ( 0.000000000000000000, 0.000000000000000000, 1.000000000000000000 ) ) ;
#50872 = VECTOR ( 'NONE', #24476, 1000.000000000000000 ) ;
#50873 = COLOUR_RGB ( '', 0.08235294, 0.09019608, 0.10196078) ;
#50874 = CARTESIAN_POINT ( 'NONE',  ( -2.300000000000032685, 2.500000000000000000, -0.3464101615137783474 ) ) ;
#50875 = EDGE_CURVE ( 'NONE', #11372, #118034, #27028, .T. ) ;
#50876 = ORIENTED_EDGE ( 'NONE', *, *, #90766, .T. ) ;
#50877 = ORIENTED_EDGE ( 'NONE', *, *, #35227, .F. ) ;
#50878 = VERTEX_POINT ( 'NONE', #47387 ) ;
#50879 = ADVANCED_BREP_SHAPE_REPRESENTATION ( '', ( #102059, #108296 ), #66615 ) ;
#50880 = ORIENTED_EDGE ( 'NONE', *, *, #29745, .T. ) ;
#50881 = PLANE ( 'NONE',  #2116 ) ;
#50882 = DIRECTION ( 'NONE',  ( 0.000000000000000000, 1.000000000000000000, 0.000000000000000000 ) ) ;
#50883 = VERTEX_POINT ( 'NONE', #64118 ) ;
#50884 = FACE_BOUND ( 'NONE', #39336, .T. ) ;
#50885 = VECTOR ( 'NONE', #16146, 1000.000000000000000 ) ;
#50886 = FACE_OUTER_BOUND ( 'NONE', #75572, .T. ) ;
#50888 = EDGE_CURVE ( 'NONE', #110619, #101819, #96063, .T. ) ;
#50887 = AXIS2_PLACEMENT_3D ( 'NONE', #38378, #118847, #89395 ) ;
#50889 = AXIS2_PLACEMENT_3D ( 'NONE', #1080, #31838, #51490 ) ;
#50890 = ORIENTED_EDGE ( 'NONE', *, *, #977, .F. ) ;
#50891 = EDGE_CURVE ( 'NONE', #109714, #114322, #110802, .T. ) ;
#50892 = CARTESIAN_POINT ( 'NONE',  ( 5.399999999999934630, 2.500000000000000000, 0.5928203230275495006 ) ) ;
#50893 = DIRECTION ( 'NONE',  ( -4.274815082592931898E-19, -0.9999939076577903929, -0.003490651415223739937 ) ) ;
#50894 = EDGE_CURVE ( 'NONE', #86833, #65792, #41709, .T. ) ;
#50895 = CARTESIAN_POINT ( 'NONE',  ( 11.89999999999990443, 12.50000000000000000, -0.3464101615137782364 ) ) ;
#50896 = ADVANCED_FACE ( 'NONE', ( #72191 ), #102341, .T. ) ;
#50897 = DIRECTION ( 'NONE',  ( 0.000000000000000000, 0.000000000000000000, 1.000000000000000000 ) ) ;
#50899 = EDGE_CURVE ( 'NONE', #120246, #71888, #16629, .T. ) ;
#50898 = CIRCLE ( 'NONE', #124047, 0.06509327318403745899 ) ;
#50900 = VERTEX_POINT ( 'NONE', #22455 ) ;
#50901 = DIRECTION ( 'NONE',  ( -0.000000000000000000, -1.000000000000000000, -0.000000000000000000 ) ) ;
#50902 = CIRCLE ( 'NONE', #67601, 0.1000000000000000472 ) ;
#50903 = AXIS2_PLACEMENT_3D ( 'NONE', #25183, #35664, #36326 ) ;
#50904 = AXIS2_PLACEMENT_3D ( 'NONE', #6299, #44978, #86152 ) ;
#50905 = ORIENTED_EDGE ( 'NONE', *, *, #40290, .T. ) ;
#50906 = EDGE_CURVE ( 'NONE', #87824, #9138, #857, .T. ) ;
#50907 = VERTEX_POINT ( 'NONE', #40143 ) ;
#50908 = CARTESIAN_POINT ( 'NONE',  ( -8.350000000000012079, 2.500000000000000000, 1.472243186433545459 ) ) ;
#50909 = ADVANCED_FACE ( 'NONE', ( #61060 ), #129196, .T. ) ;
#50910 = DIRECTION ( 'NONE',  ( 0.000000000000000000, 0.000000000000000000, 1.000000000000000000 ) ) ;
#50911 = CIRCLE ( 'NONE', #19602, 0.06509327318403745899 ) ;
#50912 = ORIENTED_EDGE ( 'NONE', *, *, #119469, .F. ) ;
#50913 = EDGE_CURVE ( 'NONE', #113123, #116569, #125317, .T. ) ;
#50914 = FACE_OUTER_BOUND ( 'NONE', #3512, .T. ) ;
#50915 = EDGE_CURVE ( 'NONE', #86766, #23803, #106526, .T. ) ;
#50916 = DIRECTION ( 'NONE',  ( 0.000000000000000000, 0.000000000000000000, 1.000000000000000000 ) ) ;
#50917 = ADVANCED_FACE ( 'NONE', ( #11321 ), #70939, .T. ) ;
#50918 = DIRECTION ( 'NONE',  ( 0.000000000000000000, -0.9999939076577903929, 0.003490651415223739937 ) ) ;
#50919 = DIRECTION ( 'NONE',  ( 0.000000000000000000, 0.000000000000000000, 1.000000000000000000 ) ) ;
#50920 = ORIENTED_EDGE ( 'NONE', *, *, #57723, .T. ) ;
#50921 = DIRECTION ( 'NONE',  ( 0.000000000000000000, 0.000000000000000000, 1.000000000000000000 ) ) ;
#50922 = EDGE_CURVE ( 'NONE', #99646, #55120, #52160, .T. ) ;
#50923 = ORIENTED_EDGE ( 'NONE', *, *, #54052, .F. ) ;
#50924 = CARTESIAN_POINT ( 'NONE',  ( 186.5000000000000000, 4.898587196589412829E-16, 4.000000000000000000 ) ) ;
#50925 = ORIENTED_EDGE ( 'NONE', *, *, #5386, .T. ) ;
#50926 = CARTESIAN_POINT ( 'NONE',  ( 14.59999999999989484, 2.500000000000000000, -0.1000000000000022815 ) ) ;
#50927 = ORIENTED_EDGE ( 'NONE', *, *, #12632, .F. ) ;
#50928 = FACE_OUTER_BOUND ( 'NONE', #98621, .T. ) ;
#50929 = CARTESIAN_POINT ( 'NONE',  ( -12.29999999999999716, 2.500000000000000000, -3.983716857408423628 ) ) ;
#50930 = CIRCLE ( 'NONE', #109404, 0.1000000000000000472 ) ;
#50931 = DIRECTION ( 'NONE',  ( 0.000000000000000000, 0.000000000000000000, 1.000000000000000000 ) ) ;
#50932 = CIRCLE ( 'NONE', #119873, 0.09999999999999999167 ) ;
#50933 = PLANE ( 'NONE',  #57098 ) ;
#50934 = DIRECTION ( 'NONE',  ( 0.000000000000000000, 1.000000000000000000, 0.000000000000000000 ) ) ;
#50935 = EDGE_LOOP ( 'NONE', ( #87052, #89794 ) ) ;
#50936 = ORIENTED_EDGE ( 'NONE', *, *, #97136, .F. ) ;
#50937 = ORIENTED_EDGE ( 'NONE', *, *, #3808, .F. ) ;
#50938 = DIRECTION ( 'NONE',  ( 0.000000000000000000, 0.000000000000000000, 1.000000000000000000 ) ) ;
#50939 = CIRCLE ( 'NONE', #17550, 0.09999999999999999167 ) ;
#50940 = AXIS2_PLACEMENT_3D ( 'NONE', #64003, #103930, #94740 ) ;
#50941 = VECTOR ( 'NONE', #9672, 1000.000000000000000 ) ;
#50942 = FACE_OUTER_BOUND ( 'NONE', #48957, .T. ) ;
#50943 = AXIS2_PLACEMENT_3D ( 'NONE', #98548, #107750, #77630 ) ;
#50945 = DIRECTION ( 'NONE',  ( 0.000000000000000000, 1.000000000000000000, 0.000000000000000000 ) ) ;
#50944 = AXIS2_PLACEMENT_3D ( 'NONE', #85256, #73488, #24403 ) ;
#50947 = ORIENTED_EDGE ( 'NONE', *, *, #38212, .T. ) ;
#50946 = ORIENTED_EDGE ( 'NONE', *, *, #69141, .F. ) ;
#50948 = VERTEX_POINT ( 'NONE', #60448 ) ;
#50949 = DIRECTION ( 'NONE',  ( 0.000000000000000000, -0.000000000000000000, 1.000000000000000000 ) ) ;
#50950 = VERTEX_POINT ( 'NONE', #121923 ) ;
#50951 = DIRECTION ( 'NONE',  ( -0.000000000000000000, -1.000000000000000000, -0.000000000000000000 ) ) ;
#50952 = VECTOR ( 'NONE', #79802, 1000.000000000000000 ) ;
#50954 = B_SPLINE_CURVE_WITH_KNOTS ( 'NONE', 3,
 ( #76618, #115888, #116529, #7209 ),
 .UNSPECIFIED., .F., .F.,
 ( 4, 4 ),
 ( 4.336808689942017736E-19, 0.002128161363186974360 ),
 .UNSPECIFIED. ) ;
#50953 = DIRECTION ( 'NONE',  ( 0.000000000000000000, -0.000000000000000000, 1.000000000000000000 ) ) ;
#50955 = CARTESIAN_POINT ( 'NONE',  ( 12.69999999999990159, 2.500000000000000000, 4.676537180435972552 ) ) ;
#50956 = CARTESIAN_POINT ( 'NONE',  ( -10.85000000000000142, 2.500000000000000000, -1.372243186433546036 ) ) ;
#50957 = CARTESIAN_POINT ( 'NONE',  ( -3.350000000000028955, 2.500000000000000000, -2.165063509461101710 ) ) ;
#50958 = CARTESIAN_POINT ( 'NONE',  ( -7.900000000000011013, 2.500000000000000000, 5.022947341949748790 ) ) ;
#50959 = VECTOR ( 'NONE', #7803, 1000.000000000000000 ) ;
#50960 = CARTESIAN_POINT ( 'NONE',  ( -7.500000000000001776, -1.500000000000000000, -9.999999999999998224 ) ) ;
#50961 = ORIENTED_EDGE ( 'NONE', *, *, #52420, .F. ) ;
#50962 = ORIENTED_EDGE ( 'NONE', *, *, #43683, .F. ) ;
#50963 = EDGE_CURVE ( 'NONE', #31381, #74338, #89803, .T. ) ;
#50964 = CARTESIAN_POINT ( 'NONE',  ( 6.849999999999929479, 12.50000000000000000, 6.906693963081109722 ) ) ;
#50966 = EDGE_CURVE ( 'NONE', #30332, #15328, #114835, .T. ) ;
#50965 = CARTESIAN_POINT ( 'NONE',  ( 3.149999999999946176, 2.500000000000000000, -6.941600689897077459 ) ) ;
#50967 = ORIENTED_EDGE ( 'NONE', *, *, #115485, .T. ) ;
#50968 =( BOUNDED_CURVE ( )  B_SPLINE_CURVE ( 2, ( #6801, #86682, #125955, #117402, #15994, #105021, #47418 ),
 .UNSPECIFIED., .F., .F. ) 
 B_SPLINE_CURVE_WITH_KNOTS ( ( 3, 2, 2, 3 ),
 ( 0.3571428571428574283, 0.3809523809523812643, 0.4047619047619051003, 0.4285714285714289362 ),
 .UNSPECIFIED. ) 
 CURVE ( )  GEOMETRIC_REPRESENTATION_ITEM ( )  RATIONAL_B_SPLINE_CURVE ( ( 0.9999999999999984457, 0.8660254037844402619, 1.000000000000000000, 0.8660254037844387076, 1.000000000000000000, 0.8660254037844364872, 1.000000000000002220 ) ) 
 REPRESENTATION_ITEM ( '' )  );
#50969 = ORIENTED_EDGE ( 'NONE', *, *, #90766, .F. ) ;
#50970 = CARTESIAN_POINT ( 'NONE',  ( 187.1927083336747160, 6.551208109652275624, -3.782341765624998686 ) ) ;
#50971 = CARTESIAN_POINT ( 'NONE',  ( 194.5000000000000000, 6.123233995736766282E-16, 5.000000000000000000 ) ) ;
#50972 = LINE ( 'NONE', #71897, #70866 ) ;
#50973 = AXIS2_PLACEMENT_3D ( 'NONE', #49904, #91097, #38810 ) ;
#50974 = DIRECTION ( 'NONE',  ( 0.000000000000000000, 0.000000000000000000, 1.000000000000000000 ) ) ;
#50975 = EDGE_CURVE ( 'NONE', #116333, #22598, #10389, .T. ) ;
#50976 = DIRECTION ( 'NONE',  ( 0.000000000000000000, 0.000000000000000000, 1.000000000000000000 ) ) ;
#50977 = FACE_OUTER_BOUND ( 'NONE', #63293, .T. ) ;
#50978 = CARTESIAN_POINT ( 'NONE',  ( 11.24999999999994316, 2.500000000000000000, -6.395190528383301931 ) ) ;
#50979 = DIRECTION ( 'NONE',  ( -4.274815082592931898E-19, -0.9999939076577903929, -0.003490651415223739937 ) ) ;
#50980 = AXIS2_PLACEMENT_3D ( 'NONE', #29275, #36526, #118931 ) ;
#50982 = CIRCLE ( 'NONE', #124112, 0.06509327318403745899 ) ;
#50981 = LINE ( 'NONE', #100068, #77140 ) ;
#50983 = EDGE_LOOP ( 'NONE', ( #25276, #54769, #52726, #129225 ) ) ;
#50984 = CIRCLE ( 'NONE', #71806, 0.06509327318403745899 ) ;
#50985 = ORIENTED_EDGE ( 'NONE', *, *, #78090, .F. ) ;
#50986 = EDGE_LOOP ( 'NONE', ( #114428, #56857, #685, #23720 ) ) ;
#50987 = ORIENTED_EDGE ( 'NONE', *, *, #8890, .T. ) ;
#50988 = ORIENTED_EDGE ( 'NONE', *, *, #2043, .F. ) ;
#50989 = CIRCLE ( 'NONE', #119925, 0.06509327318403745899 ) ;
#50990 = PLANE ( 'NONE',  #115313 ) ;
#50991 = CARTESIAN_POINT ( 'NONE',  ( 187.5000000000000000, 0.000000000000000000, 0.000000000000000000 ) ) ;
#50992 = CIRCLE ( 'NONE', #76008, 0.09999999999999982514 ) ;
#50993 = CIRCLE ( 'NONE', #22074, 0.09999999999999999167 ) ;
#50994 = ORIENTED_EDGE ( 'NONE', *, *, #107947, .F. ) ;
#50995 = CARTESIAN_POINT ( 'NONE',  ( -1.650000000000034328, 12.50000000000000000, -7.122917578226816815 ) ) ;
#50996 = DIRECTION ( 'NONE',  ( -0.000000000000000000, 1.000000000000000000, -0.000000000000000000 ) ) ;
#50997 = DIRECTION ( 'NONE',  ( 0.000000000000000000, -0.000000000000000000, 1.000000000000000000 ) ) ;
#50999 = ORIENTED_EDGE ( 'NONE', *, *, #11975, .T. ) ;
#50998 = LINE ( 'NONE', #121008, #7730 ) ;
#51000 = LINE ( 'NONE', #1236, #101829 ) ;
#51001 = AXIS2_PLACEMENT_3D ( 'NONE', #120138, #19335, #80217 ) ;
#51002 = DIRECTION ( 'NONE',  ( 0.000000000000000000, 0.000000000000000000, -1.000000000000000000 ) ) ;
#51003 = EDGE_CURVE ( 'NONE', #46382, #88884, #29192, .T. ) ;
#51004 = ORIENTED_EDGE ( 'NONE', *, *, #126689, .T. ) ;
#51005 = AXIS2_PLACEMENT_3D ( 'NONE', #97058, #114117, #15246 ) ;
#51006 = CIRCLE ( 'NONE', #88643, 0.1000000000000002554 ) ;
#51007 = CIRCLE ( 'NONE', #126303, 0.09999999999999999167 ) ;
#51008 = ORIENTED_EDGE ( 'NONE', *, *, #7883, .F. ) ;
#51009 = ORIENTED_EDGE ( 'NONE', *, *, #57740, .T. ) ;
#51010 = EDGE_LOOP ( 'NONE', ( #103521, #50124 ) ) ;
#51011 = DIRECTION ( 'NONE',  ( -0.000000000000000000, -1.000000000000000000, -0.000000000000000000 ) ) ;
#51012 = AXIS2_PLACEMENT_3D ( 'NONE', #49950, #29009, #128519 ) ;
#51013 = FACE_OUTER_BOUND ( 'NONE', #72940, .T. ) ;
#51014 = FACE_OUTER_BOUND ( 'NONE', #105259, .T. ) ;
#51015 = CIRCLE ( 'NONE', #99020, 0.1000000000000002554 ) ;
#51016 = CARTESIAN_POINT ( 'NONE',  ( -3.150000000000032330, 12.50000000000000000, -6.083687093685488989 ) ) ;
#51018 = ORIENTED_EDGE ( 'NONE', *, *, #94895, .T. ) ;
#51017 = ADVANCED_FACE ( 'NONE', ( #111440 ), #6169, .T. ) ;
#51019 = FACE_OUTER_BOUND ( 'NONE', #50295, .T. ) ;
#51020 = PLANE ( 'NONE',  #22570 ) ;
#51021 = DIRECTION ( 'NONE',  ( 0.000000000000000000, 0.000000000000000000, 1.000000000000000000 ) ) ;
#51022 = CARTESIAN_POINT ( 'NONE',  ( 21.24754738303277435, -0.7337760880902347571, 4.182111650399361835 ) ) ;
#51023 = EDGE_CURVE ( 'NONE', #67661, #108498, #64670, .T. ) ;
#51024 = ORIENTED_EDGE ( 'NONE', *, *, #34477, .F. ) ;
#51025 = ORIENTED_EDGE ( 'NONE', *, *, #64064, .F. ) ;
#51026 = VERTEX_POINT ( 'NONE', #61732 ) ;
#51028 = CIRCLE ( 'NONE', #67721, 0.06509327318403745899 ) ;
#51027 = CARTESIAN_POINT ( 'NONE',  ( 0.8499999999999553468, 12.50000000000000000, -2.230156782645139391 ) ) ;
#51029 = CONICAL_SURFACE ( 'NONE', #80264, 0.09999999999999982514, 0.003490658503988666988 ) ;
#51030 = ADVANCED_FACE ( 'NONE', ( #91817 ), #114926, .T. ) ;
#51031 = CARTESIAN_POINT ( 'NONE',  ( 2.000000000000000000, 0.000000000000000000, -5.000000000000004441 ) ) ;
#51032 = FACE_BOUND ( 'NONE', #52208, .T. ) ;
#51033 = CARTESIAN_POINT ( 'NONE',  ( -15.39999999999998082, 2.500000000000000000, 0.6928203230275518099 ) ) ;
#51034 = CYLINDRICAL_SURFACE ( 'NONE', #38195, 0.5000000000000000000 ) ;
#51035 = DIRECTION ( 'NONE',  ( 0.000000000000000000, 0.000000000000000000, 1.000000000000000000 ) ) ;
#51036 = AXIS2_PLACEMENT_3D ( 'NONE', #54527, #103656, #22534 ) ;
#51037 = AXIS2_PLACEMENT_3D ( 'NONE', #22012, #70449, #39079 ) ;
#51038 = AXIS2_PLACEMENT_3D ( 'NONE', #34365, #8569, #77331 ) ;
#51039 = DIRECTION ( 'NONE',  ( 0.000000000000000000, 0.000000000000000000, 1.000000000000000000 ) ) ;
#51040 = FACE_OUTER_BOUND ( 'NONE', #129232, .T. ) ;
#51041 = CARTESIAN_POINT ( 'NONE',  ( -13.34999999999999076, 2.500000000000000000, -1.572243186433547990 ) ) ;
#51042 = VERTEX_POINT ( 'NONE', #64757 ) ;
#51044 = DIRECTION ( 'NONE',  ( -0.000000000000000000, 1.000000000000000000, -0.000000000000000000 ) ) ;
#51043 = VECTOR ( 'NONE', #13630, 1000.000000000000000 ) ;
#51045 = CONICAL_SURFACE ( 'NONE', #46833, 0.1000000000000002554, 0.003490658503988666988 ) ;
#51046 = CONICAL_SURFACE ( 'NONE', #28043, 0.1000000000000002554, 0.003490658503988666988 ) ;
#51047 = DIRECTION ( 'NONE',  ( 0.000000000000000000, 1.000000000000000000, 0.000000000000000000 ) ) ;
#51048 = ORIENTED_EDGE ( 'NONE', *, *, #118642, .T. ) ;
#51049 = VERTEX_POINT ( 'NONE', #44479 ) ;
#51050 = AXIS2_PLACEMENT_3D ( 'NONE', #20216, #60159, #100066 ) ;
#51051 = DIRECTION ( 'NONE',  ( -0.000000000000000000, -1.000000000000000000, -0.000000000000000000 ) ) ;
#51052 = DIRECTION ( 'NONE',  ( 0.000000000000000000, 0.000000000000000000, 1.000000000000000000 ) ) ;
#51053 = FACE_BOUND ( 'NONE', #128670, .T. ) ;
#51054 = DIRECTION ( 'NONE',  ( 0.000000000000000000, 0.000000000000000000, -1.000000000000000000 ) ) ;
#51055 = EDGE_CURVE ( 'NONE', #50102, #41939, #126919, .T. ) ;
#51056 = CARTESIAN_POINT ( 'NONE',  ( -2.950000000000029932, 2.500000000000000000, 2.065063509461097624 ) ) ;
#51057 = ORIENTED_EDGE ( 'NONE', *, *, #74151, .T. ) ;
#51058 = DIRECTION ( 'NONE',  ( 0.000000000000000000, -0.9999939076577903929, 0.003490651415223739937 ) ) ;
#51059 = EDGE_CURVE ( 'NONE', #118212, #123047, #18785, .T. ) ;
#51060 = CARTESIAN_POINT ( 'NONE',  ( 184.1666666666666856, -6.668395609140176816, -3.850000000000003642 ) ) ;
#51061 = ADVANCED_FACE ( 'NONE', ( #56223 ), #104471, .T. ) ;
#51063 = ORIENTED_EDGE ( 'NONE', *, *, #66247, .F. ) ;
#51062 = VECTOR ( 'NONE', #620, 1000.000000000000000 ) ;
#51064 = DIRECTION ( 'NONE',  ( -4.274815082592931898E-19, -0.9999939076577903929, -0.003490651415223739937 ) ) ;
#51065 = PLANE ( 'NONE',  #70041 ) ;
#51066 = ADVANCED_FACE ( 'NONE', ( #106614 ), #123355, .T. ) ;
#51067 = EDGE_CURVE ( 'NONE', #22544, #93141, #14577, .T. ) ;
#51068 = FACE_OUTER_BOUND ( 'NONE', #92278, .T. ) ;
#51069 = ADVANCED_FACE ( 'NONE', ( #77167 ), #66690, .T. ) ;
#51070 = CARTESIAN_POINT ( 'NONE',  ( -9.600000000000008527, 12.50000000000000000, -4.395220292106235327 ) ) ;
#51071 = CIRCLE ( 'NONE', #44810, 0.06509327318403745899 ) ;
#51072 = VERTEX_POINT ( 'NONE', #104673 ) ;
#51073 = DIRECTION ( 'NONE',  ( 0.000000000000000000, 0.000000000000000000, -1.000000000000000000 ) ) ;
#51074 = EDGE_CURVE ( 'NONE', #84952, #101891, #116431, .T. ) ;
#51075 = FACE_OUTER_BOUND ( 'NONE', #34488, .T. ) ;
#51076 = CARTESIAN_POINT ( 'NONE',  ( 184.7395833340161175, 4.445597072760175905, 7.699999999999896261 ) ) ;
#51077 = ORIENTED_EDGE ( 'NONE', *, *, #103963, .T. ) ;
#51078 = ORIENTED_EDGE ( 'NONE', *, *, #89977, .F. ) ;
#51079 = EDGE_CURVE ( 'NONE', #15576, #102929, #117068, .T. ) ;
#51080 = DIRECTION ( 'NONE',  ( 0.000000000000000000, 0.000000000000000000, 1.000000000000000000 ) ) ;
#51081 = EDGE_CURVE ( 'NONE', #87216, #120954, #79453, .T. ) ;
#51082 = ORIENTED_EDGE ( 'NONE', *, *, #5051, .T. ) ;
#51083 = CARTESIAN_POINT ( 'NONE',  ( -12.49999999999999467, 2.500000000000000000, -3.737306695894647035 ) ) ;
#51084 = DIRECTION ( 'NONE',  ( 0.000000000000000000, 1.000000000000000000, 0.000000000000000000 ) ) ;
#51085 = CIRCLE ( 'NONE', #82475, 0.1000000000000002554 ) ;
#51086 = CARTESIAN_POINT ( 'NONE',  ( -5.200000000000022382, 12.50000000000000000, 4.676537180435972552 ) ) ;
#51087 = ORIENTED_EDGE ( 'NONE', *, *, #91845, .T. ) ;
#51088 = DIRECTION ( 'NONE',  ( -0.000000000000000000, -1.000000000000000000, -0.000000000000000000 ) ) ;
#51089 = DIRECTION ( 'NONE',  ( 0.000000000000000000, 1.000000000000000000, 0.000000000000000000 ) ) ;
#51090 = LINE ( 'NONE', #90996, #82035 ) ;
#51091 = DIRECTION ( 'NONE',  ( -4.274815082592931898E-19, -0.9999939076577903929, -0.003490651415223739937 ) ) ;
#51092 = CARTESIAN_POINT ( 'NONE',  ( -7.900000000000014566, 2.500000000000000000, -0.1000000000000022815 ) ) ;
#51093 = DIRECTION ( 'NONE',  ( -0.000000000000000000, -1.000000000000000000, -0.000000000000000000 ) ) ;
#51094 = EDGE_LOOP ( 'NONE', ( #52132, #76579, #36459, #53788 ) ) ;
#51095 = VERTEX_POINT ( 'NONE', #47075 ) ;
#51096 = DIRECTION ( 'NONE',  ( 0.000000000000000000, -0.9999939076577903929, 0.003490651415223739937 ) ) ;
#51098 = ORIENTED_EDGE ( 'NONE', *, *, #69954, .T. ) ;
#51097 = VECTOR ( 'NONE', #100905, 1000.000000000000000 ) ;
#51099 = VECTOR ( 'NONE', #93049, 1000.000000000000000 ) ;
#51100 = PLANE ( 'NONE',  #122462 ) ;
#51102 = ORIENTED_EDGE ( 'NONE', *, *, #50790, .F. ) ;
#51101 = ORIENTED_EDGE ( 'NONE', *, *, #739, .T. ) ;
#51103 = VERTEX_POINT ( 'NONE', #45139 ) ;
#51104 = AXIS2_PLACEMENT_3D ( 'NONE', #53155, #92420, #10615 ) ;
#51105 = DIRECTION ( 'NONE',  ( 0.000000000000000000, 0.000000000000000000, -1.000000000000000000 ) ) ;
#51106 = VECTOR ( 'NONE', #97380, 1000.000000000000000 ) ;
#51107 = DIRECTION ( 'NONE',  ( 0.000000000000000000, 1.000000000000000000, 0.000000000000000000 ) ) ;
#51108 = DIRECTION ( 'NONE',  ( 0.000000000000000000, 0.000000000000000000, -1.000000000000000000 ) ) ;
#51109 = DIRECTION ( 'NONE',  ( 0.000000000000000000, 0.000000000000000000, 1.000000000000000000 ) ) ;
#51110 = CARTESIAN_POINT ( 'NONE',  ( -5.650000000000023448, 2.500000000000000000, -6.248780366869526759 ) ) ;
#51111 = DIRECTION ( 'NONE',  ( 0.000000000000000000, 1.000000000000000000, 0.000000000000000000 ) ) ;
#51112 = DIRECTION ( 'NONE',  ( -0.000000000000000000, 1.000000000000000000, -0.000000000000000000 ) ) ;
#51113 = CARTESIAN_POINT ( 'NONE',  ( 16.55874544816229488, 0.4845305829427787869, -6.091953208798931207 ) ) ;
#51114 = CARTESIAN_POINT ( 'NONE',  ( -7.100000000000018296, 12.50000000000000000, -2.385244779468109755E-15 ) ) ;
#51115 = EDGE_LOOP ( 'NONE', ( #70806, #9892 ) ) ;
#51116 = ADVANCED_FACE ( 'NONE', ( #124337 ), #96156, .T. ) ;
#51117 = AXIS2_PLACEMENT_3D ( 'NONE', #82524, #122440, #15018 ) ;
#51118 = VECTOR ( 'NONE', #64637, 1000.000000000000000 ) ;
#51119 = EDGE_CURVE ( 'NONE', #66361, #73062, #83561, .T. ) ;
#51120 = LINE ( 'NONE', #99576, #67398 ) ;
#51121 = VECTOR ( 'NONE', #69127, 1000.000000000000000 ) ;
#51122 = CONICAL_SURFACE ( 'NONE', #115847, 0.1000000000000002554, 0.003490658503988666988 ) ;
#51123 = ORIENTED_EDGE ( 'NONE', *, *, #77357, .T. ) ;
#51124 = EDGE_LOOP ( 'NONE', ( #96449, #102003, #66129, #57020 ) ) ;
#51125 = CARTESIAN_POINT ( 'NONE',  ( 105.0000000000000142, 8.500000000000000000, 0.2500000000000003886 ) ) ;
#51126 = CARTESIAN_POINT ( 'NONE',  ( 3.749999999999940492, 12.50000000000000000, 5.802370205355744659 ) ) ;
#51127 = AXIS2_PLACEMENT_3D ( 'NONE', #90195, #100043, #18888 ) ;
#51128 = DIRECTION ( 'NONE',  ( 0.000000000000000000, 0.000000000000000000, -1.000000000000000000 ) ) ;
#51129 = VECTOR ( 'NONE', #70702, 1000.000000000000000 ) ;
#51131 = CARTESIAN_POINT ( 'NONE',  ( 6.649999999999931077, 12.50000000000000000, -6.430097255199264339 ) ) ;
#51130 = AXIS2_PLACEMENT_3D ( 'NONE', #60619, #103098, #93284 ) ;
#51132 = DIRECTION ( 'NONE',  ( 0.000000000000000000, 0.000000000000000000, -1.000000000000000000 ) ) ;
#51133 = DIRECTION ( 'NONE',  ( 0.000000000000000000, -0.000000000000000000, 1.000000000000000000 ) ) ;
#51134 = VERTEX_POINT ( 'NONE', #14991 ) ;
#51136 = EDGE_LOOP ( 'NONE', ( #48215, #46041, #99396, #2342 ) ) ;
#51135 = CIRCLE ( 'NONE', #86610, 8.040022453829767102 ) ;
#51137 = VECTOR ( 'NONE', #51064, 1000.000000000000000 ) ;
#51138 = VERTEX_POINT ( 'NONE', #66049 ) ;
#51139 = CARTESIAN_POINT ( 'NONE',  ( -14.14999999999998614, 2.500000000000000000, 1.472243186433549456 ) ) ;
#51140 = ORIENTED_EDGE ( 'NONE', *, *, #62204, .F. ) ;
#51141 = CIRCLE ( 'NONE', #124290, 0.06509327318403745899 ) ;
#51142 = VERTEX_POINT ( 'NONE', #95521 ) ;
#51143 = DIRECTION ( 'NONE',  ( 0.000000000000000000, 0.000000000000000000, 1.000000000000000000 ) ) ;
#51144 = DIRECTION ( 'NONE',  ( -0.000000000000000000, -1.000000000000000000, -0.000000000000000000 ) ) ;
#51145 = DIRECTION ( 'NONE',  ( 0.000000000000000000, -0.9999939076577903929, 0.003490651415223739937 ) ) ;
#51146 = CARTESIAN_POINT ( 'NONE',  ( 10.19999999999991580, 12.50000000000000000, -0.3464101615137783474 ) ) ;
#51147 = DIRECTION ( 'NONE',  ( -0.000000000000000000, -1.000000000000000000, -0.000000000000000000 ) ) ;
#51148 = VERTEX_POINT ( 'NONE', #94871 ) ;
#51149 = CARTESIAN_POINT ( 'NONE',  ( -5.850000000000022737, 12.50000000000000000, -2.099970236277064473 ) ) ;
#51150 = FACE_OUTER_BOUND ( 'NONE', #109236, .T. ) ;
#51151 = LINE ( 'NONE', #91060, #66632 ) ;
#51152 = PLANE ( 'NONE',  #28486 ) ;
#51153 = AXIS2_PLACEMENT_3D ( 'NONE', #93791, #113425, #33588 ) ;
#51154 = DIRECTION ( 'NONE',  ( 0.000000000000000000, 1.000000000000000000, 0.000000000000000000 ) ) ;
#51155 = EDGE_CURVE ( 'NONE', #2020, #2451, #46404, .T. ) ;
#51156 = VERTEX_POINT ( 'NONE', #5184 ) ;
#51157 = ORIENTED_EDGE ( 'NONE', *, *, #103558, .T. ) ;
#51158 = ORIENTED_EDGE ( 'NONE', *, *, #79012, .F. ) ;
#51159 = DIRECTION ( 'NONE',  ( 0.000000000000000000, 1.000000000000000000, 0.000000000000000000 ) ) ;
#51160 = VERTEX_POINT ( 'NONE', #105981 ) ;
#51161 = CONICAL_SURFACE ( 'NONE', #95070, 0.09999999999999982514, 0.003490658503988666988 ) ;
#51162 = LINE ( 'NONE', #91070, #123933 ) ;
#51164 = EDGE_CURVE ( 'NONE', #58918, #112146, #81504, .T. ) ;
#51163 = DIRECTION ( 'NONE',  ( 0.000000000000000000, 1.000000000000000000, 0.000000000000000000 ) ) ;
#51165 = AXIS2_PLACEMENT_3D ( 'NONE', #20920, #19636, #623 ) ;
#51167 = ORIENTED_EDGE ( 'NONE', *, *, #10641, .T. ) ;
#51166 = EDGE_CURVE ( 'NONE', #76721, #115200, #100276, .T. ) ;
#51168 = CARTESIAN_POINT ( 'NONE',  ( -7.900000000000011013, 2.500000000000000000, 3.637306695894644726 ) ) ;
#51169 = CARTESIAN_POINT ( 'NONE',  ( -9.600000000000006750, 12.50000000000000000, 3.637306695894644726 ) ) ;
#51170 = PLANE ( 'NONE',  #191 ) ;
#51171 = EDGE_CURVE ( 'NONE', #122705, #41669, #48056, .T. ) ;
#51172 = DIRECTION ( 'NONE',  ( 0.000000000000000000, 1.000000000000000000, 0.000000000000000000 ) ) ;
#51173 = AXIS2_PLACEMENT_3D ( 'NONE', #106845, #15894, #36849 ) ;
#51174 = CARTESIAN_POINT ( 'NONE',  ( -10.80000000000000071, 12.50000000000000000, 4.330127018922196314 ) ) ;
#51175 = EDGE_CURVE ( 'NONE', #51588, #125598, #89898, .T. ) ;
#51176 = CONICAL_SURFACE ( 'NONE', #7223, 0.1000000000000002554, 0.003490658503988666988 ) ;
#51177 = ORIENTED_EDGE ( 'NONE', *, *, #28870, .F. ) ;
#51178 = VERTEX_POINT ( 'NONE', #19529 ) ;
#51179 = EDGE_CURVE ( 'NONE', #67593, #41594, #100034, .T. ) ;
#51180 = CARTESIAN_POINT ( 'NONE',  ( 23.99341564996507259, 2.839174804732068846, -2.508498394836132572 ) ) ;
#51181 = CARTESIAN_POINT ( 'NONE',  ( -9.550000000000006040, 2.500000000000000000, -2.265063509461101798 ) ) ;
#51182 = DIRECTION ( 'NONE',  ( 0.000000000000000000, 0.000000000000000000, 1.000000000000000000 ) ) ;
#51183 = CARTESIAN_POINT ( 'NONE',  ( 3.149999999999944400, 2.500000000000000000, 2.511473670974873507 ) ) ;
#51184 = VERTEX_POINT ( 'NONE', #117709 ) ;
#51185 = VECTOR ( 'NONE', #31114, 1000.000000000000000 ) ;
#51187 = ORIENTED_EDGE ( 'NONE', *, *, #111788, .F. ) ;
#51186 = VECTOR ( 'NONE', #98860, 1000.000000000000000 ) ;
#51188 = CARTESIAN_POINT ( 'NONE',  ( -0.4000000000000331624, 12.50000000000000000, 0.000000000000000000 ) ) ;
#51189 = CARTESIAN_POINT ( 'NONE',  ( 7.499999999999925393, 12.50000000000000000, -3.637306695894650055 ) ) ;
#51190 = FACE_OUTER_BOUND ( 'NONE', #122563, .T. ) ;
#51191 = VECTOR ( 'NONE', #37026, 1000.000000000000000 ) ;
#51192 = ORIENTED_EDGE ( 'NONE', *, *, #92293, .T. ) ;
#51193 = LINE ( 'NONE', #30911, #28097 ) ;
#51194 = DIRECTION ( 'NONE',  ( -0.000000000000000000, 1.000000000000000000, -0.000000000000000000 ) ) ;
#51195 = VERTEX_POINT ( 'NONE', #39205 ) ;
#51196 = DIRECTION ( 'NONE',  ( 0.000000000000000000, -0.9999939076577903929, 0.003490651415223739937 ) ) ;
#51197 = ORIENTED_EDGE ( 'NONE', *, *, #51344, .T. ) ;
#51198 = CARTESIAN_POINT ( 'NONE',  ( -9.150000000000009237, 12.50000000000000000, 2.857883832488649301 ) ) ;
#51199 = VERTEX_POINT ( 'NONE', #20178 ) ;
#51200 = ADVANCED_FACE ( 'NONE', ( #79115 ), #28071, .T. ) ;
#51201 = CIRCLE ( 'NONE', #63718, 0.1000000000000002554 ) ;
#51202 = EDGE_LOOP ( 'NONE', ( #101073, #66776 ) ) ;
#51203 = CARTESIAN_POINT ( 'NONE',  ( -12.89999999999999147, 12.50000000000000000, 1.843143693225357538E-15 ) ) ;
#51204 = DIRECTION ( 'NONE',  ( -0.000000000000000000, -1.000000000000000000, -0.000000000000000000 ) ) ;
#51205 = CONICAL_SURFACE ( 'NONE', #128483, 0.09999999999999982514, 0.003490658503988666988 ) ;
#51206 = CIRCLE ( 'NONE', #7262, 0.09999999999999982514 ) ;
#51207 = AXIS2_PLACEMENT_3D ( 'NONE', #129338, #102276, #93743 ) ;
#51208 = EDGE_LOOP ( 'NONE', ( #5587, #39719, #91459, #105087 ) ) ;
#51209 = ORIENTED_EDGE ( 'NONE', *, *, #33794, .T. ) ;
#51210 = EDGE_CURVE ( 'NONE', #2267, #121831, #77284, .T. ) ;
#51211 = LINE ( 'NONE', #69534, #3874 ) ;
#51212 = DIRECTION ( 'NONE',  ( -4.274815082592931898E-19, -0.9999939076577903929, -0.003490651415223739937 ) ) ;
#51213 = EDGE_LOOP ( 'NONE', ( #21528, #3785 ) ) ;
#51214 = EDGE_CURVE ( 'NONE', #16035, #52780, #107911, .T. ) ;
#51215 = CARTESIAN_POINT ( 'NONE',  ( 184.8177083336747160, 4.367472073101515306, 7.564683531250000925 ) ) ;
#51216 = CIRCLE ( 'NONE', #9443, 0.06509327318403745899 ) ;
#51217 = VECTOR ( 'NONE', #117400, 1000.000000000000000 ) ;
#51218 = DIRECTION ( 'NONE',  ( 0.000000000000000000, 1.000000000000000000, 0.000000000000000000 ) ) ;
#51219 = CARTESIAN_POINT ( 'NONE',  ( 6.049999999999934097, 2.500000000000000000, -2.411473670974877859 ) ) ;
#51220 = PLANE ( 'NONE',  #126176 ) ;
#51221 = EDGE_CURVE ( 'NONE', #3072, #84759, #90184, .T. ) ;
#51222 = AXIS2_PLACEMENT_3D ( 'NONE', #65943, #56746, #27962 ) ;
#51223 = CARTESIAN_POINT ( 'NONE',  ( -5.400000000000023448, 2.500000000000000000, -5.122947341949753763 ) ) ;
#51224 = PLANE ( 'NONE',  #65178 ) ;
#51225 = EDGE_CURVE ( 'NONE', #101891, #78289, #68971, .T. ) ;
#51226 = EDGE_CURVE ( 'NONE', #118876, #97854, #83654, .T. ) ;
#51227 = CIRCLE ( 'NONE', #124378, 0.1000000000000000472 ) ;
#51228 = AXIS2_PLACEMENT_3D ( 'NONE', #116725, #65700, #46073 ) ;
#51229 = ORIENTED_EDGE ( 'NONE', *, *, #20560, .T. ) ;
#51230 = ORIENTED_EDGE ( 'NONE', *, *, #24188, .F. ) ;
#51231 = DIRECTION ( 'NONE',  ( 0.000000000000000000, 0.000000000000000000, 1.000000000000000000 ) ) ;
#51232 = EDGE_CURVE ( 'NONE', #48128, #78911, #12524, .T. ) ;
#51233 = ORIENTED_EDGE ( 'NONE', *, *, #86638, .F. ) ;
#51234 = DIRECTION ( 'NONE',  ( -4.274815082592931898E-19, -0.9999939076577903929, -0.003490651415223739937 ) ) ;
#51235 = DIRECTION ( 'NONE',  ( 0.000000000000000000, 1.000000000000000000, 0.000000000000000000 ) ) ;
#51236 = CIRCLE ( 'NONE', #90924, 0.1000000000000000472 ) ;
#51237 = DIRECTION ( 'NONE',  ( -0.000000000000000000, -1.000000000000000000, -0.000000000000000000 ) ) ;
#51239 = ORIENTED_EDGE ( 'NONE', *, *, #70676, .T. ) ;
#51238 = ORIENTED_EDGE ( 'NONE', *, *, #72895, .T. ) ;
#51240 = FACE_BOUND ( 'NONE', #8317, .T. ) ;
#51241 = ORIENTED_EDGE ( 'NONE', *, *, #32552, .F. ) ;
#51242 = DIRECTION ( 'NONE',  ( 0.000000000000000000, 0.000000000000000000, -1.000000000000000000 ) ) ;
#51243 = FACE_OUTER_BOUND ( 'NONE', #26665, .T. ) ;
#51244 = EDGE_CURVE ( 'NONE', #36298, #126837, #94009, .T. ) ;
#51245 = CARTESIAN_POINT ( 'NONE',  ( 115.5000000000000000, 2.000000000000000000, 2.000000000000003553 ) ) ;
#51247 = ADVANCED_FACE ( 'NONE', ( #88249 ), #29274, .T. ) ;
#51246 = LINE ( 'NONE', #46880, #24251 ) ;
#51248 = CARTESIAN_POINT ( 'NONE',  ( -5.850000000000021849, 2.500000000000000000, -5.802370205355749988 ) ) ;
#51249 = DIRECTION ( 'NONE',  ( 0.000000000000000000, 0.000000000000000000, -1.000000000000000000 ) ) ;
#51250 = DIRECTION ( 'NONE',  ( 0.000000000000000000, -1.000000000000000000, 0.000000000000000000 ) ) ;
#51251 = DIRECTION ( 'NONE',  ( -0.000000000000000000, 1.000000000000000000, -0.000000000000000000 ) ) ;
#51252 = DIRECTION ( 'NONE',  ( 0.000000000000000000, 0.000000000000000000, -1.000000000000000000 ) ) ;
#51253 = CARTESIAN_POINT ( 'NONE',  ( -0.2000000000000408673, 2.500000000000000000, -4.083716857408426826 ) ) ;
#51254 = AXIS2_PLACEMENT_3D ( 'NONE', #125263, #15931, #25769 ) ;
#51255 = DIRECTION ( 'NONE',  ( -0.000000000000000000, 1.000000000000000000, -0.000000000000000000 ) ) ;
#51256 = VERTEX_POINT ( 'NONE', #128211 ) ;
#51257 = ORIENTED_EDGE ( 'NONE', *, *, #17539, .F. ) ;
#51258 = ORIENTED_EDGE ( 'NONE', *, *, #40833, .F. ) ;
#51259 = EDGE_LOOP ( 'NONE', ( #96577, #83489, #120165, #77060 ) ) ;
#51260 = DIRECTION ( 'NONE',  ( 0.000000000000000000, 0.000000000000000000, 1.000000000000000000 ) ) ;
#51261 = DIRECTION ( 'NONE',  ( 0.000000000000000000, -0.000000000000000000, 1.000000000000000000 ) ) ;
#51263 = ORIENTED_EDGE ( 'NONE', *, *, #11711, .T. ) ;
#51262 = ORIENTED_EDGE ( 'NONE', *, *, #26531, .T. ) ;
#51264 = EDGE_LOOP ( 'NONE', ( #69406, #77941, #87327, #104455 ) ) ;
#51265 = CARTESIAN_POINT ( 'NONE',  ( -12.69999999999999218, 2.500000000000000000, -0.3464101615137741286 ) ) ;
#51266 = CIRCLE ( 'NONE', #111884, 0.1000000000000002554 ) ;
#51267 = AXIS2_PLACEMENT_3D ( 'NONE', #79679, #38498, #30605 ) ;
#51268 = CARTESIAN_POINT ( 'NONE',  ( 0.8499999999999536815, 2.500000000000000000, 5.802370205355744659 ) ) ;
#51269 = CARTESIAN_POINT ( 'NONE',  ( 5.849999999999933920, 2.500000000000000000, 5.802370205355744659 ) ) ;
#51270 = CARTESIAN_POINT ( 'NONE',  ( 12.09999999999990195, 2.500000000000000000, 0.6928203230275494784 ) ) ;
#51271 = DIRECTION ( 'NONE',  ( 0.000000000000000000, 1.000000000000000000, 0.000000000000000000 ) ) ;
#51272 = PLANE ( 'NONE',  #7949 ) ;
#51273 = DIRECTION ( 'NONE',  ( -0.000000000000000000, -1.000000000000000000, -0.000000000000000000 ) ) ;
#51274 = EDGE_CURVE ( 'NONE', #6262, #31484, #37595, .T. ) ;
#51275 = EDGE_LOOP ( 'NONE', ( #128848, #43541, #92548, #92536 ) ) ;
#51276 = CARTESIAN_POINT ( 'NONE',  ( 2.899999999999944844, 2.500000000000000000, 3.637306695894644726 ) ) ;
#51277 = ORIENTED_EDGE ( 'NONE', *, *, #120955, .T. ) ;
#51278 = AXIS2_PLACEMENT_3D ( 'NONE', #124421, #83213, #93669 ) ;
#51279 = VERTEX_POINT ( 'NONE', #30665 ) ;
#51280 = EDGE_CURVE ( 'NONE', #19267, #114403, #64761, .T. ) ;
#51281 = ORIENTED_EDGE ( 'NONE', *, *, #98565, .F. ) ;
#51282 = CIRCLE ( 'NONE', #30352, 0.1000000000000002554 ) ;
#51283 = DIRECTION ( 'NONE',  ( 0.000000000000000000, -0.9999939076577903929, 0.003490651415223739937 ) ) ;
#51284 = ORIENTED_EDGE ( 'NONE', *, *, #48424, .T. ) ;
#51285 = ORIENTED_EDGE ( 'NONE', *, *, #17474, .T. ) ;
#51286 = EDGE_LOOP ( 'NONE', ( #11085, #94339, #104498, #16934 ) ) ;
#51287 = DIRECTION ( 'NONE',  ( 0.000000000000000000, 0.000000000000000000, 1.000000000000000000 ) ) ;
#51288 = EDGE_CURVE ( 'NONE', #83267, #87429, #60128, .T. ) ;
#51290 = CIRCLE ( 'NONE', #55474, 0.09999999999999982514 ) ;
#51289 = DIRECTION ( 'NONE',  ( 0.000000000000000000, 0.000000000000000000, -1.000000000000000000 ) ) ;
#51291 = CARTESIAN_POINT ( 'NONE',  ( 3.099999999999945466, 2.500000000000000000, 0.2464101615137735679 ) ) ;
#51292 = CIRCLE ( 'NONE', #32425, 0.1000000000000002554 ) ;
#51293 = CARTESIAN_POINT ( 'NONE',  ( -9.600000000000008527, 2.500000000000000000, 4.330127018922196314 ) ) ;
#51294 = CARTESIAN_POINT ( 'NONE',  ( -10.65000000000000213, 2.500000000000000000, 1.918653347947321564 ) ) ;
#51295 = DIRECTION ( 'NONE',  ( 0.000000000000000000, 0.000000000000000000, 1.000000000000000000 ) ) ;
#51296 = DIRECTION ( 'NONE',  ( -0.000000000000000000, 1.000000000000000000, -0.000000000000000000 ) ) ;
#51297 = VERTEX_POINT ( 'NONE', #17585 ) ;
#51298 = DIRECTION ( 'NONE',  ( 0.000000000000000000, 0.000000000000000000, -1.000000000000000000 ) ) ;
#51299 = EDGE_LOOP ( 'NONE', ( #29568, #78594 ) ) ;
#51300 = DIRECTION ( 'NONE',  ( -0.000000000000000000, -1.000000000000000000, -0.000000000000000000 ) ) ;
#51301 = LINE ( 'NONE', #92485, #21126 ) ;
#51302 = VERTEX_POINT ( 'NONE', #87618 ) ;
#51303 = DIRECTION ( 'NONE',  ( 0.000000000000000000, 0.000000000000000000, 1.000000000000000000 ) ) ;
#51304 = DIRECTION ( 'NONE',  ( -0.000000000000000000, -1.000000000000000000, -0.000000000000000000 ) ) ;
#51305 = AXIS2_PLACEMENT_3D ( 'NONE', #15657, #65415, #125616 ) ;
#51306 = VERTEX_POINT ( 'NONE', #97445 ) ;
#51307 = CIRCLE ( 'NONE', #97247, 0.06509327318403745899 ) ;
#51309 = CARTESIAN_POINT ( 'NONE',  ( 9.149999999999920419, 12.50000000000000000, 2.857883832488649301 ) ) ;
#51308 = VECTOR ( 'NONE', #126640, 1000.000000000000000 ) ;
#51310 = VERTEX_POINT ( 'NONE', #127556 ) ;
#51311 = CIRCLE ( 'NONE', #120569, 0.1000000000000002554 ) ;
#51312 = VERTEX_POINT ( 'NONE', #37883 ) ;
#51313 = DIRECTION ( 'NONE',  ( 0.000000000000000000, 0.000000000000000000, 1.000000000000000000 ) ) ;
#51314 = DIRECTION ( 'NONE',  ( 0.000000000000000000, 0.000000000000000000, -1.000000000000000000 ) ) ;
#51315 = CARTESIAN_POINT ( 'NONE',  ( 184.6718750003414016, 9.264065473108010111E-16, -7.564683531250000925 ) ) ;
#51316 = CARTESIAN_POINT ( 'NONE',  ( 5.399999999999932854, 12.50000000000000000, 3.572213422710607489 ) ) ;
#51317 = CIRCLE ( 'NONE', #82705, 0.06509327318403745899 ) ;
#51318 = DIRECTION ( 'NONE',  ( -0.000000000000000000, 1.000000000000000000, -0.000000000000000000 ) ) ;
#51319 = AXIS2_PLACEMENT_3D ( 'NONE', #79727, #77149, #128856 ) ;
#51320 = ORIENTED_EDGE ( 'NONE', *, *, #30554, .F. ) ;
#51321 = VECTOR ( 'NONE', #120660, 1000.000000000000000 ) ;
#51322 = DIRECTION ( 'NONE',  ( -0.000000000000000000, -1.000000000000000000, -0.000000000000000000 ) ) ;
#51323 = EDGE_LOOP ( 'NONE', ( #105535, #119911 ) ) ;
#51324 = CONICAL_SURFACE ( 'NONE', #91015, 0.1000000000000000472, 0.003490658503988666988 ) ;
#51325 = DIRECTION ( 'NONE',  ( 0.000000000000000000, 1.000000000000000000, 0.000000000000000000 ) ) ;
#51328 = EDGE_CURVE ( 'NONE', #18575, #104669, #77794, .T. ) ;
#51327 = VECTOR ( 'NONE', #3407, 1000.000000000000000 ) ;
#51326 = CARTESIAN_POINT ( 'NONE',  ( -6.250000000000015987, 12.50000000000000000, 5.867463478539781896 ) ) ;
#51329 = AXIS2_PLACEMENT_3D ( 'NONE', #112754, #23730, #114038 ) ;
#51330 = CONICAL_SURFACE ( 'NONE', #36744, 0.09999999999999999167, 0.003490658503988666988 ) ;
#51331 = EDGE_CURVE ( 'NONE', #89644, #25512, #54306, .T. ) ;
#51332 = CARTESIAN_POINT ( 'NONE',  ( 186.2552083336747444, 6.551208109652275624, -3.782341765624998686 ) ) ;
#51333 = FACE_OUTER_BOUND ( 'NONE', #67176, .T. ) ;
#51334 = DIRECTION ( 'NONE',  ( 0.000000000000000000, 1.000000000000000000, 0.000000000000000000 ) ) ;
#51335 = CARTESIAN_POINT ( 'NONE',  ( 3.349999999999945466, 2.500000000000000000, -7.188010851410854052 ) ) ;
#51336 = EDGE_CURVE ( 'NONE', #48809, #32526, #58819, .T. ) ;
#51337 = DIRECTION ( 'NONE',  ( 0.000000000000000000, 0.000000000000000000, 1.000000000000000000 ) ) ;
#51338 = VERTEX_POINT ( 'NONE', #3759 ) ;
#51339 = CARTESIAN_POINT ( 'NONE',  ( 184.4166666666666856, 6.668395609140176816, 3.850000000000000977 ) ) ;
#51340 = DIRECTION ( 'NONE',  ( 0.000000000000000000, 1.000000000000000000, 0.000000000000000000 ) ) ;
#51341 = DIRECTION ( 'NONE',  ( 0.000000000000000000, 1.000000000000000000, 0.000000000000000000 ) ) ;
#51342 = ADVANCED_FACE ( 'NONE', ( #110488 ), #111107, .T. ) ;
#51343 = EDGE_CURVE ( 'NONE', #107840, #2581, #6, .T. ) ;
#51344 = EDGE_CURVE ( 'NONE', #79361, #46788, #127467, .T. ) ;
#51345 = CONICAL_SURFACE ( 'NONE', #32565, 0.1000000000000000472, 0.003490658503988666988 ) ;
#51346 = ORIENTED_EDGE ( 'NONE', *, *, #15812, .T. ) ;
#51347 = DIRECTION ( 'NONE',  ( -0.000000000000000000, -1.000000000000000000, -0.000000000000000000 ) ) ;
#51348 = ORIENTED_EDGE ( 'NONE', *, *, #118583, .F. ) ;
#51349 = ORIENTED_EDGE ( 'NONE', *, *, #12863, .F. ) ;
#51350 = CARTESIAN_POINT ( 'NONE',  ( -4.150000000000025224, 2.500000000000000000, -1.372243186433550033 ) ) ;
#51351 = AXIS2_PLACEMENT_3D ( 'NONE', #125114, #35456, #3404 ) ;
#51352 = ORIENTED_EDGE ( 'NONE', *, *, #52989, .F. ) ;
#51353 = CARTESIAN_POINT ( 'NONE',  ( 18.27284318114482176, -0.4998542452738461428, -4.791717918554368794 ) ) ;
#51354 = DIRECTION ( 'NONE',  ( 0.000000000000000000, -0.000000000000000000, 1.000000000000000000 ) ) ;
#51355 = AXIS2_PLACEMENT_3D ( 'NONE', #38866, #98376, #78775 ) ;
#51356 = AXIS2_PLACEMENT_3D ( 'NONE', #44924, #75646, #126704 ) ;
#51357 = EDGE_LOOP ( 'NONE', ( #69064, #47897, #52759, #116116 ) ) ;
#51358 = CARTESIAN_POINT ( 'NONE',  ( -3.950000000000026379, 12.50000000000000000, 6.776507416713035248 ) ) ;
#51359 = DIRECTION ( 'NONE',  ( 0.000000000000000000, 1.000000000000000000, 0.000000000000000000 ) ) ;
#51360 = ORIENTED_EDGE ( 'NONE', *, *, #30183, .F. ) ;
#51361 = AXIS2_PLACEMENT_3D ( 'NONE', #43157, #92887, #12997 ) ;
#51362 = ORIENTED_EDGE ( 'NONE', *, *, #33728, .F. ) ;
#51363 = CONICAL_SURFACE ( 'NONE', #72201, 0.1000000000000002554, 0.003490658503988666988 ) ;
#51364 = EDGE_LOOP ( 'NONE', ( #3371, #29749 ) ) ;
#51365 = FACE_OUTER_BOUND ( 'NONE', #76716, .T. ) ;
#51366 = FACE_OUTER_BOUND ( 'NONE', #13518, .T. ) ;
#51367 = FACE_OUTER_BOUND ( 'NONE', #15308, .T. ) ;
#51368 = FACE_BOUND ( 'NONE', #66000, .T. ) ;
#51369 = EDGE_LOOP ( 'NONE', ( #27426, #63485, #71605, #105847 ) ) ;
#51370 = DIRECTION ( 'NONE',  ( -4.274815082592931898E-19, -0.9999939076577903929, -0.003490651415223739937 ) ) ;
#51371 = DIRECTION ( 'NONE',  ( -0.000000000000000000, 1.000000000000000000, -0.000000000000000000 ) ) ;
#51372 = VERTEX_POINT ( 'NONE', #41130 ) ;
#51373 = CARTESIAN_POINT ( 'NONE',  ( -6.650000000000014566, 12.50000000000000000, 5.802370205355744659 ) ) ;
#51375 = DIRECTION ( 'NONE',  ( -0.000000000000000000, -1.000000000000000000, -0.000000000000000000 ) ) ;
#51374 = AXIS2_PLACEMENT_3D ( 'NONE', #22558, #101748, #13989 ) ;
#51376 = AXIS2_PLACEMENT_3D ( 'NONE', #128527, #89212, #28370 ) ;
#51378 = ADVANCED_FACE ( 'NONE', ( #10981 ), #12906, .T. ) ;
#51377 = CARTESIAN_POINT ( 'NONE',  ( -1.700000000000035261, 12.50000000000000000, 4.265033745738159077 ) ) ;
#51379 = CARTESIAN_POINT ( 'NONE',  ( 1.049999999999953637, 12.50000000000000000, 2.511473670974873507 ) ) ;
#51380 = CARTESIAN_POINT ( 'NONE',  ( -2.100000000000033396, 12.50000000000000000, -3.637306695894650055 ) ) ;
#51381 = EDGE_CURVE ( 'NONE', #7787, #98954, #31340, .T. ) ;
#51382 = CARTESIAN_POINT ( 'NONE',  ( -13.34999999999999076, 12.50000000000000000, -2.857883832488651521 ) ) ;
#51383 = DIRECTION ( 'NONE',  ( 0.000000000000000000, 0.000000000000000000, -1.000000000000000000 ) ) ;
#51384 = ADVANCED_FACE ( 'NONE', ( #3124 ), #66992, .T. ) ;
#51385 = ORIENTED_EDGE ( 'NONE', *, *, #103171, .T. ) ;
#51386 = VERTEX_POINT ( 'NONE', #120949 ) ;
#51388 = VERTEX_POINT ( 'NONE', #23385 ) ;
#51387 = EDGE_CURVE ( 'NONE', #128844, #41725, #46090, .T. ) ;
#51389 = ORIENTED_EDGE ( 'NONE', *, *, #85160, .F. ) ;
#51390 = DIRECTION ( 'NONE',  ( -0.000000000000000000, 1.000000000000000000, -0.000000000000000000 ) ) ;
#51391 = ADVANCED_FACE ( 'NONE', ( #62050 ), #29374, .T. ) ;
#51392 = CARTESIAN_POINT ( 'NONE',  ( 0.8499999999999557909, 12.50000000000000000, -7.253104124594891289 ) ) ;
#51393 = ORIENTED_EDGE ( 'NONE', *, *, #92546, .F. ) ;
#51394 = FACE_BOUND ( 'NONE', #31104, .T. ) ;
#51395 = PLANE ( 'NONE',  #14421 ) ;
#51396 = DIRECTION ( 'NONE',  ( 0.000000000000000000, 1.000000000000000000, 0.000000000000000000 ) ) ;
#51397 = ADVANCED_FACE ( 'NONE', ( #100654 ), #35628, .T. ) ;
#51398 = CARTESIAN_POINT ( 'NONE',  ( 4.149999999999941735, 2.500000000000000000, -1.372243186433550033 ) ) ;
#51399 = ADVANCED_FACE ( 'NONE', ( #71206 ), #2161, .T. ) ;
#51400 = VECTOR ( 'NONE', #57829, 1000.000000000000000 ) ;
#51401 = DIRECTION ( 'NONE',  ( 0.000000000000000000, -0.000000000000000000, 1.000000000000000000 ) ) ;
#51402 = AXIS2_PLACEMENT_3D ( 'NONE', #91867, #42121, #92497 ) ;
#51403 = DIRECTION ( 'NONE',  ( 0.000000000000000000, 1.000000000000000000, 0.000000000000000000 ) ) ;
#51404 = DIRECTION ( 'NONE',  ( 0.000000000000000000, -0.9999939076577903929, 0.003490651415223739937 ) ) ;
#51405 = DIRECTION ( 'NONE',  ( -0.000000000000000000, -1.000000000000000000, -0.000000000000000000 ) ) ;
#51406 = DIRECTION ( 'NONE',  ( 0.000000000000000000, -0.000000000000000000, 1.000000000000000000 ) ) ;
#51407 = APPLICATION_CONTEXT ( 'automotive_design' ) ;
#51408 = CARTESIAN_POINT ( 'NONE',  ( 11.89999999999990798, 2.500000000000000000, -4.776537180435977525 ) ) ;
#51409 = EDGE_LOOP ( 'NONE', ( #56226, #91514 ) ) ;
#51410 = ADVANCED_FACE ( 'NONE', ( #22778 ), #98298, .T. ) ;
#51411 = EDGE_LOOP ( 'NONE', ( #118947, #8464, #71974, #43446 ) ) ;
#51412 = EDGE_LOOP ( 'NONE', ( #97554, #81847 ) ) ;
#51413 = ORIENTED_EDGE ( 'NONE', *, *, #49282, .T. ) ;
#51414 = ORIENTED_EDGE ( 'NONE', *, *, #26378, .F. ) ;
#51415 = ORIENTED_EDGE ( 'NONE', *, *, #35160, .F. ) ;
#51416 = AXIS2_PLACEMENT_3D ( 'NONE', #29119, #100419, #49405 ) ;
#51417 = CARTESIAN_POINT ( 'NONE',  ( 175.5000000000000000, 6.123233995736766282E-16, 5.000000000000000000 ) ) ;
#51418 = VERTEX_POINT ( 'NONE', #62694 ) ;
#51419 = VECTOR ( 'NONE', #117191, 1000.000000000000000 ) ;
#51420 = AXIS2_PLACEMENT_3D ( 'NONE', #29523, #28886, #69431 ) ;
#51421 = CARTESIAN_POINT ( 'NONE',  ( -3.950000000000029932, 2.500000000000000000, -6.048780366869526581 ) ) ;
#51422 = CARTESIAN_POINT ( 'NONE',  ( -4.350000000000023626, 2.500000000000000000, -2.611473670974877592 ) ) ;
#51423 = CARTESIAN_POINT ( 'NONE',  ( 10.64999999999990976, 2.500000000000000000, 1.918653347947321564 ) ) ;
#51425 = CONICAL_SURFACE ( 'NONE', #38618, 0.09999999999999999167, 0.003490658503988666988 ) ;
#51424 = CARTESIAN_POINT ( 'NONE',  ( -6.050000000000020250, 12.50000000000000000, -2.576566944158915184 ) ) ;
#51426 = ORIENTED_EDGE ( 'NONE', *, *, #26387, .T. ) ;
#51427 = DIRECTION ( 'NONE',  ( 0.000000000000000000, 0.000000000000000000, 1.000000000000000000 ) ) ;
#51428 = ORIENTED_EDGE ( 'NONE', *, *, #13810, .T. ) ;
#51429 = ORIENTED_EDGE ( 'NONE', *, *, #77646, .T. ) ;
#51430 = CARTESIAN_POINT ( 'NONE',  ( 5.449999999999937117, 2.500000000000000000, -6.595190528383302109 ) ) ;
#51431 = CARTESIAN_POINT ( 'NONE',  ( 5.599999999999934808, 2.500000000000000000, -4.676537180435978769 ) ) ;
#51432 = FACE_OUTER_BOUND ( 'NONE', #58138, .T. ) ;
#51433 = VECTOR ( 'NONE', #3883, 1000.000000000000000 ) ;
#51434 = VERTEX_POINT ( 'NONE', #1814 ) ;
#51435 = EDGE_LOOP ( 'NONE', ( #102547, #58406 ) ) ;
#51436 = LINE ( 'NONE', #100507, #88132 ) ;
#51437 = EDGE_CURVE ( 'NONE', #90278, #33163, #108762, .T. ) ;
#51438 = CARTESIAN_POINT ( 'NONE',  ( -0.4500000000000402012, 2.500000000000000000, 2.065063509461097624 ) ) ;
#51439 = DIRECTION ( 'NONE',  ( 0.000000000000000000, 0.000000000000000000, 1.000000000000000000 ) ) ;
#51440 = CARTESIAN_POINT ( 'NONE',  ( -10.65000000000000391, 2.500000000000000000, -6.048780366869523029 ) ) ;
#51441 = EDGE_LOOP ( 'NONE', ( #73891, #725 ) ) ;
#51442 = DIRECTION ( 'NONE',  ( 0.000000000000000000, 0.000000000000000000, 1.000000000000000000 ) ) ;
#51443 = CONICAL_SURFACE ( 'NONE', #30520, 0.09999999999999982514, 0.003490658503988666988 ) ;
#51444 = ORIENTED_EDGE ( 'NONE', *, *, #126738, .F. ) ;
#51446 = AXIS2_PLACEMENT_3D ( 'NONE', #31098, #33030, #100459 ) ;
#51445 = DIRECTION ( 'NONE',  ( 0.000000000000000000, -0.9999939076577903929, 0.003490651415223739937 ) ) ;
#51447 = ORIENTED_EDGE ( 'NONE', *, *, #22942, .F. ) ;
#51448 = VECTOR ( 'NONE', #70672, 1000.000000000000000 ) ;
#51449 = DIRECTION ( 'NONE',  ( -0.000000000000000000, -1.000000000000000000, -0.000000000000000000 ) ) ;
#51450 = DIRECTION ( 'NONE',  ( -0.000000000000000000, -1.000000000000000000, -0.000000000000000000 ) ) ;
#51451 = DIRECTION ( 'NONE',  ( 0.000000000000000000, 0.000000000000000000, 1.000000000000000000 ) ) ;
#51452 = PLANE ( 'NONE',  #129591 ) ;
#51453 = ORIENTED_EDGE ( 'NONE', *, *, #55468, .T. ) ;
#51454 = CIRCLE ( 'NONE', #89096, 0.06509327318403745899 ) ;
#51455 = CARTESIAN_POINT ( 'NONE',  ( 9.349999999999916156, 2.500000000000000000, 6.841600689897072485 ) ) ;
#51456 = DIRECTION ( 'NONE',  ( 0.000000000000000000, -0.000000000000000000, 1.000000000000000000 ) ) ;
#51457 = ORIENTED_EDGE ( 'NONE', *, *, #49201, .T. ) ;
#51458 = VERTEX_POINT ( 'NONE', #43074 ) ;
#51459 = ORIENTED_EDGE ( 'NONE', *, *, #56230, .F. ) ;
#51460 = DIRECTION ( 'NONE',  ( 0.000000000000000000, -0.000000000000000000, 1.000000000000000000 ) ) ;
#51461 = FACE_OUTER_BOUND ( 'NONE', #51646, .T. ) ;
#51462 =( NAMED_UNIT ( * ) PLANE_ANGLE_UNIT ( ) SI_UNIT ( $, .RADIAN. ) );
#51463 = LINE ( 'NONE', #3632, #86696 ) ;
#51464 = CARTESIAN_POINT ( 'NONE',  ( -5.850000000000019185, 2.500000000000000000, 6.495190528383297135 ) ) ;
#51465 = CARTESIAN_POINT ( 'NONE',  ( -2.050000000000032685, 2.500000000000000000, -2.065063509461102065 ) ) ;
#51466 = DIRECTION ( 'NONE',  ( 0.000000000000000000, -0.000000000000000000, 1.000000000000000000 ) ) ;
#51467 = CARTESIAN_POINT ( 'NONE',  ( 2.049999999999950084, 2.500000000000000000, 2.265063509461097357 ) ) ;
#51468 = EDGE_CURVE ( 'NONE', #88843, #17565, #77386, .T. ) ;
#51469 = ORIENTED_EDGE ( 'NONE', *, *, #9097, .T. ) ;
#51470 = DIRECTION ( 'NONE',  ( 0.000000000000000000, 0.000000000000000000, 1.000000000000000000 ) ) ;
#51471 = ADVANCED_FACE ( 'NONE', ( #63323 ), #83622, .T. ) ;
#51472 = CARTESIAN_POINT ( 'NONE',  ( 0.6499999999999561684, 12.50000000000000000, -2.576566944158915184 ) ) ;
#51473 = DIRECTION ( 'NONE',  ( -4.274815082592931898E-19, -0.9999939076577903929, -0.003490651415223739937 ) ) ;
#51474 = LINE ( 'NONE', #121476, #116981 ) ;
#51475 = ADVANCED_FACE ( 'NONE', ( #122899 ), #125496, .T. ) ;
#51476 = VERTEX_POINT ( 'NONE', #25990 ) ;
#51477 = DIRECTION ( 'NONE',  ( -0.000000000000000000, -1.000000000000000000, -0.000000000000000000 ) ) ;
#51478 = AXIS2_PLACEMENT_3D ( 'NONE', #37403, #129023, #66833 ) ;
#51479 = AXIS2_PLACEMENT_3D ( 'NONE', #87821, #38100, #79329 ) ;
#51480 = CARTESIAN_POINT ( 'NONE',  ( 1.249999999999988898, 2.500000000000000000, -6.595190528383302109 ) ) ;
#51482 = ORIENTED_EDGE ( 'NONE', *, *, #100387, .F. ) ;
#51481 = LINE ( 'NONE', #3019, #100689 ) ;
#51483 = ADVANCED_FACE ( 'NONE', ( #14207 ), #83736, .T. ) ;
#51484 = ADVANCED_FACE ( 'NONE', ( #46252 ), #12621, .T. ) ;
#51485 = EDGE_CURVE ( 'NONE', #18602, #95183, #126106, .T. ) ;
#51486 = ADVANCED_FACE ( 'NONE', ( #86159 ), #14669, .T. ) ;
#51487 = EDGE_CURVE ( 'NONE', #9001, #40822, #20945, .T. ) ;
#51488 = ORIENTED_EDGE ( 'NONE', *, *, #103124, .T. ) ;
#51489 = CONICAL_SURFACE ( 'NONE', #70534, 0.1000000000000002554, 0.003490658503988666988 ) ;
#51490 = DIRECTION ( 'NONE',  ( 0.000000000000000000, 0.000000000000000000, -1.000000000000000000 ) ) ;
#51491 = ORIENTED_EDGE ( 'NONE', *, *, #117516, .F. ) ;
#51492 = ORIENTED_EDGE ( 'NONE', *, *, #37970, .F. ) ;
#51493 = CARTESIAN_POINT ( 'NONE',  ( -4.800000000000028244, 2.500000000000000000, -3.983716857408426293 ) ) ;
#51494 = ADVANCED_FACE ( 'NONE', ( #46922 ), #75080, .T. ) ;
#51495 = CARTESIAN_POINT ( 'NONE',  ( 21.23528140090977345, 2.699413673072324826, -2.293764360948901793 ) ) ;
#51496 = CARTESIAN_POINT ( 'NONE',  ( 6.049999999999932321, 2.500000000000000000, 6.741600689897071952 ) ) ;
#51497 = CIRCLE ( 'NONE', #49363, 8.040022453829767102 ) ;
#51498 = DIRECTION ( 'NONE',  ( 0.000000000000000000, 0.000000000000000000, -1.000000000000000000 ) ) ;
#51499 = EDGE_LOOP ( 'NONE', ( #18229, #95582 ) ) ;
#51500 = CONICAL_SURFACE ( 'NONE', #128883, 0.1000000000000000472, 0.003490658503988666988 ) ;
#51501 = DIRECTION ( 'NONE',  ( 0.000000000000000000, 1.000000000000000000, 0.000000000000000000 ) ) ;
#51502 = ORIENTED_EDGE ( 'NONE', *, *, #73831, .T. ) ;
#51503 = DIRECTION ( 'NONE',  ( 0.000000000000000000, 0.000000000000000000, 1.000000000000000000 ) ) ;
#51504 = DIRECTION ( 'NONE',  ( 0.000000000000000000, 0.000000000000000000, -1.000000000000000000 ) ) ;
#51505 = ORIENTED_EDGE ( 'NONE', *, *, #44526, .T. ) ;
#51506 = VERTEX_POINT ( 'NONE', #126766 ) ;
#51507 = EDGE_LOOP ( 'NONE', ( #40348, #14000, #43841, #53100 ) ) ;
#51508 = ORIENTED_EDGE ( 'NONE', *, *, #20910, .T. ) ;
#51509 = DIRECTION ( 'NONE',  ( 0.000000000000000000, 1.000000000000000000, 0.000000000000000000 ) ) ;
#51510 = CARTESIAN_POINT ( 'NONE',  ( 13.51931942407928311, 1.499999999999935829, 8.074217333073997693 ) ) ;
#51511 = DIRECTION ( 'NONE',  ( 0.000000000000000000, 1.000000000000000000, 0.000000000000000000 ) ) ;
#51512 = FACE_BOUND ( 'NONE', #26485, .T. ) ;
#51513 = DIRECTION ( 'NONE',  ( 0.000000000000000000, 1.000000000000000000, 0.000000000000000000 ) ) ;
#51514 = CIRCLE ( 'NONE', #11786, 0.1000000000000002554 ) ;
#51515 = CARTESIAN_POINT ( 'NONE',  ( 183.8229166673494888, -4.445597072760122614, 7.699999999999998401 ) ) ;
#51516 = DIRECTION ( 'NONE',  ( 0.000000000000000000, 0.000000000000000000, 1.000000000000000000 ) ) ;
#51517 = CARTESIAN_POINT ( 'NONE',  ( -10.85000000000000142, 2.500000000000000000, -6.495190528383298911 ) ) ;
#51518 = VECTOR ( 'NONE', #29758, 1000.000000000000000 ) ;
#51519 = AXIS2_PLACEMENT_3D ( 'NONE', #44178, #84098, #84760 ) ;
#51520 = DIRECTION ( 'NONE',  ( 0.000000000000000000, 1.000000000000000000, 0.000000000000000000 ) ) ;
#51521 = CIRCLE ( 'NONE', #91226, 0.06509327318403745899 ) ;
#51522 = DIRECTION ( 'NONE',  ( -4.274815082592931898E-19, -0.9999939076577903929, -0.003490651415223739937 ) ) ;
#51523 = EDGE_CURVE ( 'NONE', #75902, #121648, #56698, .T. ) ;
#51524 = DIRECTION ( 'NONE',  ( 0.000000000000000000, -0.9999939076577903929, 0.003490651415223739937 ) ) ;
#51525 = AXIS2_PLACEMENT_3D ( 'NONE', #121870, #23672, #121227 ) ;
#51526 = EDGE_CURVE ( 'NONE', #73897, #123363, #104570, .T. ) ;
#51527 = VECTOR ( 'NONE', #102862, 1000.000000000000000 ) ;
#51528 = DIRECTION ( 'NONE',  ( -0.000000000000000000, 1.000000000000000000, -0.000000000000000000 ) ) ;
#51529 = CIRCLE ( 'NONE', #124686, 0.06509327318403741736 ) ;
#51530 = EDGE_CURVE ( 'NONE', #74881, #55968, #96008, .T. ) ;
#51531 = ORIENTED_EDGE ( 'NONE', *, *, #70989, .F. ) ;
#51532 = ORIENTED_EDGE ( 'NONE', *, *, #5367, .T. ) ;
#51533 = ORIENTED_EDGE ( 'NONE', *, *, #100146, .T. ) ;
#51534 = VERTEX_POINT ( 'NONE', #103898 ) ;
#51535 = VERTEX_POINT ( 'NONE', #63974 ) ;
#51536 = DIRECTION ( 'NONE',  ( 0.000000000000000000, 1.000000000000000000, 0.000000000000000000 ) ) ;
#51537 = DIRECTION ( 'NONE',  ( -0.000000000000000000, 1.000000000000000000, -0.000000000000000000 ) ) ;
#51539 = EDGE_CURVE ( 'NONE', #84566, #34168, #55438, .T. ) ;
#51538 = ORIENTED_EDGE ( 'NONE', *, *, #127638, .T. ) ;
#51540 = FACE_BOUND ( 'NONE', #92029, .T. ) ;
#51541 = CARTESIAN_POINT ( 'NONE',  ( 1.449999999999949551, 2.500000000000000000, 6.841600689897072485 ) ) ;
#51542 = EDGE_CURVE ( 'NONE', #20680, #78871, #94712, .T. ) ;
#51543 = ADVANCED_FACE ( 'NONE', ( #124180 ), #33576, .T. ) ;
#51546 = EDGE_CURVE ( 'NONE', #121027, #56893, #43942, .T. ) ;
#51545 = VECTOR ( 'NONE', #100172, 1000.000000000000000 ) ;
#51544 = CIRCLE ( 'NONE', #3410, 0.06509327318403745899 ) ;
#51547 = ORIENTED_EDGE ( 'NONE', *, *, #13287, .F. ) ;
#51548 = DIRECTION ( 'NONE',  ( -0.000000000000000000, -1.000000000000000000, -0.000000000000000000 ) ) ;
#51549 = CARTESIAN_POINT ( 'NONE',  ( 3.549999999999943867, 12.50000000000000000, -6.148780366869526226 ) ) ;
#51550 = DIRECTION ( 'NONE',  ( 0.000000000000000000, 0.000000000000000000, 1.000000000000000000 ) ) ;
#51551 = DIRECTION ( 'NONE',  ( 0.000000000000000000, -0.9999939076577903929, 0.003490651415223739937 ) ) ;
#51552 = ORIENTED_EDGE ( 'NONE', *, *, #79411, .F. ) ;
#51553 = LINE ( 'NONE', #60720, #88910 ) ;
#51554 = ADVANCED_FACE ( 'NONE', ( #65239 ), #79536, .T. ) ;
#51555 = VERTEX_POINT ( 'NONE', #5672 ) ;
#51556 = ORIENTED_EDGE ( 'NONE', *, *, #103403, .F. ) ;
#51557 = DIRECTION ( 'NONE',  ( 0.000000000000000000, 0.000000000000000000, 1.000000000000000000 ) ) ;
#51558 = DIRECTION ( 'NONE',  ( 0.000000000000000000, 0.000000000000000000, -1.000000000000000000 ) ) ;
#51559 = ORIENTED_EDGE ( 'NONE', *, *, #15268, .F. ) ;
#51560 = DIRECTION ( 'NONE',  ( -0.000000000000000000, -1.000000000000000000, -0.000000000000000000 ) ) ;
#51561 = CARTESIAN_POINT ( 'NONE',  ( 11.89999999999990798, 2.500000000000000000, 3.883716857408421319 ) ) ;
#51562 = LINE ( 'NONE', #120927, #72878 ) ;
#51563 = DIRECTION ( 'NONE',  ( 0.000000000000000000, -0.000000000000000000, 1.000000000000000000 ) ) ;
#51564 = CARTESIAN_POINT ( 'NONE',  ( 187.2395833340161460, 4.445597072760117285, 7.699999999999999289 ) ) ;
#51565 = ORIENTED_EDGE ( 'NONE', *, *, #44535, .T. ) ;
#51566 = DIRECTION ( 'NONE',  ( 0.000000000000000000, 1.000000000000000000, 0.000000000000000000 ) ) ;
#51567 = ADVANCED_FACE ( 'NONE', ( #54780 ), #127560, .T. ) ;
#51568 = EDGE_LOOP ( 'NONE', ( #48622, #111255, #99443, #25629 ) ) ;
#51569 = FACE_OUTER_BOUND ( 'NONE', #99958, .T. ) ;
#51570 = AXIS2_PLACEMENT_3D ( 'NONE', #107415, #110635, #120459 ) ;
#51571 = EDGE_LOOP ( 'NONE', ( #3419, #66894, #121269, #109351 ) ) ;
#51572 = FACE_OUTER_BOUND ( 'NONE', #5728, .T. ) ;
#51573 = VERTEX_POINT ( 'NONE', #6309 ) ;
#51574 = CARTESIAN_POINT ( 'NONE',  ( 1.049999999999953637, 12.50000000000000000, 2.576566944158910744 ) ) ;
#51575 = CARTESIAN_POINT ( 'NONE',  ( -10.40000000000000213, 12.50000000000000000, -0.7579135962115916003 ) ) ;
#51576 = DIRECTION ( 'NONE',  ( 0.000000000000000000, 0.000000000000000000, 1.000000000000000000 ) ) ;
#51577 = PLANE ( 'NONE',  #660 ) ;
#51578 = CARTESIAN_POINT ( 'NONE',  ( 16.89731025888663041, 0.9183091266721068457, -5.698390440797600931 ) ) ;
#51579 = ORIENTED_EDGE ( 'NONE', *, *, #113001, .T. ) ;
#51582 = ORIENTED_EDGE ( 'NONE', *, *, #100856, .T. ) ;
#51581 = AXIS2_PLACEMENT_3D ( 'NONE', #73088, #123463, #34470 ) ;
#51580 = VECTOR ( 'NONE', #3341, 1000.000000000000000 ) ;
#51583 = ORIENTED_EDGE ( 'NONE', *, *, #94770, .T. ) ;
#51584 = DIRECTION ( 'NONE',  ( 0.000000000000000000, 1.000000000000000000, 0.000000000000000000 ) ) ;
#51585 = ADVANCED_FACE ( 'NONE', ( #26623 ), #96235, .T. ) ;
#51586 = PLANE ( 'NONE',  #7604 ) ;
#51587 = DIRECTION ( 'NONE',  ( 0.000000000000000000, 0.000000000000000000, -1.000000000000000000 ) ) ;
#51589 = ORIENTED_EDGE ( 'NONE', *, *, #110864, .T. ) ;
#51588 = VERTEX_POINT ( 'NONE', #115633 ) ;
#51590 = EDGE_LOOP ( 'NONE', ( #60480, #127476, #76073, #33282 ) ) ;
#51591 = DIRECTION ( 'NONE',  ( -0.000000000000000000, 1.000000000000000000, -0.000000000000000000 ) ) ;
#51593 = AXIS2_PLACEMENT_3D ( 'NONE', #98187, #8503, #76626 ) ;
#51592 = CONICAL_SURFACE ( 'NONE', #59919, 0.1000000000000002554, 0.003490658503988666988 ) ;
#51594 = ORIENTED_EDGE ( 'NONE', *, *, #13783, .T. ) ;
#51595 = PLANE ( 'NONE',  #128124 ) ;
#51596 = DIRECTION ( 'NONE',  ( -0.000000000000000000, -1.000000000000000000, -0.000000000000000000 ) ) ;
#51597 = AXIS2_PLACEMENT_3D ( 'NONE', #66058, #66699, #57541 ) ;
#51598 = DIRECTION ( 'NONE',  ( -0.000000000000000000, 1.000000000000000000, -0.000000000000000000 ) ) ;
#51599 = CARTESIAN_POINT ( 'NONE',  ( -10.00000000000000355, 12.50000000000000000, 3.702399969078682407 ) ) ;
#51600 = DIRECTION ( 'NONE',  ( 0.000000000000000000, 0.000000000000000000, -1.000000000000000000 ) ) ;
#51601 = DIRECTION ( 'NONE',  ( -0.000000000000000000, 1.000000000000000000, -0.000000000000000000 ) ) ;
#51602 = CARTESIAN_POINT ( 'NONE',  ( -3.550000000000027356, 12.50000000000000000, 1.818653347947321475 ) ) ;
#51603 = EDGE_CURVE ( 'NONE', #114390, #126294, #23101, .T. ) ;
#51604 = CARTESIAN_POINT ( 'NONE',  ( 10.84999999999991260, 12.50000000000000000, 7.188010851410848723 ) ) ;
#51605 = ORIENTED_EDGE ( 'NONE', *, *, #5063, .T. ) ;
#51606 = CARTESIAN_POINT ( 'NONE',  ( -0.6500000000000394351, 2.500000000000000000, 2.511473670974873507 ) ) ;
#51607 = CARTESIAN_POINT ( 'NONE',  ( 59.74180401148688446, -3.401974578037520125, 5.439313020096691709 ) ) ;
#51608 = EDGE_LOOP ( 'NONE', ( #3275, #121431 ) ) ;
#51609 = ORIENTED_EDGE ( 'NONE', *, *, #92994, .T. ) ;
#51610 = CARTESIAN_POINT ( 'NONE',  ( 184.7343750003414016, 8.734944146203032389, 5.348610694689227483E-16 ) ) ;
#51611 = CARTESIAN_POINT ( 'NONE',  ( 0.6499999999999561684, 2.500000000000000000, -2.611473670974877592 ) ) ;
#51612 = DIRECTION ( 'NONE',  ( 0.000000000000000000, 1.000000000000000000, 0.000000000000000000 ) ) ;
#51613 = CARTESIAN_POINT ( 'NONE',  ( -1.450000000000035483, 12.50000000000000000, 1.818653347947321475 ) ) ;
#51614 = DIRECTION ( 'NONE',  ( 0.000000000000000000, 1.000000000000000000, 0.000000000000000000 ) ) ;
#51615 = DIRECTION ( 'NONE',  ( 0.000000000000000000, 0.000000000000000000, -1.000000000000000000 ) ) ;
#51616 = VECTOR ( 'NONE', #125861, 1000.000000000000000 ) ;
#51617 = FACE_OUTER_BOUND ( 'NONE', #11022, .T. ) ;
#51618 = CARTESIAN_POINT ( 'NONE',  ( -12.04999999999999716, 2.500000000000000000, -2.165063509461097713 ) ) ;
#51619 = CIRCLE ( 'NONE', #53662, 0.06509327318403745899 ) ;
#51620 = CIRCLE ( 'NONE', #39115, 0.06509327318403745899 ) ;
#51621 = CARTESIAN_POINT ( 'NONE',  ( -10.20000000000000462, 12.50000000000000000, 4.676537180435972552 ) ) ;
#51622 = EDGE_LOOP ( 'NONE', ( #18241, #87619 ) ) ;
#51623 = ORIENTED_EDGE ( 'NONE', *, *, #68368, .T. ) ;
#51624 = AXIS2_PLACEMENT_3D ( 'NONE', #115193, #74019, #84483 ) ;
#51625 = EDGE_CURVE ( 'NONE', #5536, #42483, #73265, .T. ) ;
#51626 = ORIENTED_EDGE ( 'NONE', *, *, #101498, .F. ) ;
#51627 = ORIENTED_EDGE ( 'NONE', *, *, #23877, .F. ) ;
#51628 = AXIS2_PLACEMENT_3D ( 'NONE', #104048, #24842, #66688 ) ;
#51629 = DIRECTION ( 'NONE',  ( -0.000000000000000000, 1.000000000000000000, -0.000000000000000000 ) ) ;
#51630 = CARTESIAN_POINT ( 'NONE',  ( -4.800000000000022915, 12.50000000000000000, 3.983716857408420076 ) ) ;
#51631 = AXIS2_PLACEMENT_3D ( 'NONE', #83857, #44591, #23018 ) ;
#51632 = EDGE_LOOP ( 'NONE', ( #65107, #40244 ) ) ;
#51633 = CARTESIAN_POINT ( 'NONE',  ( -3.150000000000029221, 12.50000000000000000, 2.511473670974873507 ) ) ;
#51634 = CARTESIAN_POINT ( 'NONE',  ( -4.150000000000024336, 12.50000000000000000, 1.537336459617582918 ) ) ;
#51636 = AXIS2_PLACEMENT_3D ( 'NONE', #46385, #106601, #104036 ) ;
#51635 = AXIS2_PLACEMENT_3D ( 'NONE', #3605, #12123, #83473 ) ;
#51637 = CARTESIAN_POINT ( 'NONE',  ( 127.5000000000000000, -1.500000000000000000, 6.000000000000000000 ) ) ;
#51639 = ORIENTED_EDGE ( 'NONE', *, *, #12762, .T. ) ;
#51638 = CARTESIAN_POINT ( 'NONE',  ( 14.14999999999989200, 2.500000000000000000, -2.165063509461101710 ) ) ;
#51640 = EDGE_CURVE ( 'NONE', #9353, #7114, #89982, .T. ) ;
#51641 = ADVANCED_FACE ( 'NONE', ( #8898 ), #77639, .T. ) ;
#51642 = ADVANCED_FACE ( 'NONE', ( #69771 ), #100546, .T. ) ;
#51643 = CARTESIAN_POINT ( 'NONE',  ( -4.999999999999990230, 2.500000000000000000, -4.430127018922202176 ) ) ;
#51644 = EDGE_CURVE ( 'NONE', #74427, #86526, #21036, .T. ) ;
#51645 = FACE_OUTER_BOUND ( 'NONE', #90469, .T. ) ;
#51646 = EDGE_LOOP ( 'NONE', ( #63033, #13854, #23332, #129315 ) ) ;
#51647 = EDGE_CURVE ( 'NONE', #26349, #77466, #27254, .T. ) ;
#51648 = EDGE_LOOP ( 'NONE', ( #55986, #1439 ) ) ;
#51649 = ORIENTED_EDGE ( 'NONE', *, *, #76014, .F. ) ;
#51650 = ORIENTED_EDGE ( 'NONE', *, *, #73083, .F. ) ;
#51651 = CARTESIAN_POINT ( 'NONE',  ( 11.64999999999990621, 2.500000000000000000, 6.395190528383296602 ) ) ;
#51653 = EDGE_CURVE ( 'NONE', #93502, #126749, #98388, .T. ) ;
#51652 = AXIS2_PLACEMENT_3D ( 'NONE', #67812, #88071, #18713 ) ;
#51654 = DIRECTION ( 'NONE',  ( 0.000000000000000000, 0.000000000000000000, 1.000000000000000000 ) ) ;
#51655 = LINE ( 'NONE', #22200, #115149 ) ;
#51656 = EDGE_CURVE ( 'NONE', #32318, #118375, #112883, .T. ) ;
#51658 = ORIENTED_EDGE ( 'NONE', *, *, #48269, .F. ) ;
#51657 = EDGE_CURVE ( 'NONE', #24428, #87918, #4279, .T. ) ;
#51659 = LINE ( 'NONE', #100104, #100417 ) ;
#51660 = ORIENTED_EDGE ( 'NONE', *, *, #57775, .F. ) ;
#51661 = DIRECTION ( 'NONE',  ( 0.000000000000000000, -0.000000000000000000, 1.000000000000000000 ) ) ;
#51662 = DIRECTION ( 'NONE',  ( 0.000000000000000000, -0.000000000000000000, 1.000000000000000000 ) ) ;
#51663 = CARTESIAN_POINT ( 'NONE',  ( -3.300000000000027800, 2.500000000000000000, 0.09999999999999772959 ) ) ;
#51664 = CARTESIAN_POINT ( 'NONE',  ( 0.3999999999999559464, 12.50000000000000000, -4.265033745738164406 ) ) ;
#51665 = EDGE_CURVE ( 'NONE', #122222, #12736, #127644, .T. ) ;
#51666 = EDGE_LOOP ( 'NONE', ( #41652, #17343, #26195, #59676 ) ) ;
#51667 = VECTOR ( 'NONE', #7112, 1000.000000000000000 ) ;
#51668 = AXIS2_PLACEMENT_3D ( 'NONE', #20568, #69007, #100415 ) ;
#51669 = ORIENTED_EDGE ( 'NONE', *, *, #60954, .F. ) ;
#51670 = VERTEX_POINT ( 'NONE', #97295 ) ;
#51671 = CARTESIAN_POINT ( 'NONE',  ( 5.649999999999936406, 2.500000000000000000, -6.941600689897077459 ) ) ;
#51672 = DIRECTION ( 'NONE',  ( 0.000000000000000000, 0.000000000000000000, 1.000000000000000000 ) ) ;
#51673 = FACE_BOUND ( 'NONE', #109802, .T. ) ;
#51674 = DIRECTION ( 'NONE',  ( 0.000000000000000000, 0.000000000000000000, 1.000000000000000000 ) ) ;
#51675 = LINE ( 'NONE', #11732, #80045 ) ;
#51676 = AXIS2_PLACEMENT_3D ( 'NONE', #2499, #32001, #43759 ) ;
#51677 = DIRECTION ( 'NONE',  ( -0.000000000000000000, -1.000000000000000000, -0.000000000000000000 ) ) ;
#51678 = CARTESIAN_POINT ( 'NONE',  ( 10.84999999999990905, 12.50000000000000000, -5.802370205355749988 ) ) ;
#51679 = CARTESIAN_POINT ( 'NONE',  ( 106.0514428414850272, 8.500000000000000000, -1.125000000000000222 ) ) ;
#51680 = DIRECTION ( 'NONE',  ( 0.000000000000000000, -0.9999939076577903929, 0.003490651415223739937 ) ) ;
#51681 = EDGE_LOOP ( 'NONE', ( #77081, #15868 ) ) ;
#51683 = VECTOR ( 'NONE', #76475, 1000.000000000000000 ) ;
#51682 = VECTOR ( 'NONE', #109061, 1000.000000000000000 ) ;
#51684 = DIRECTION ( 'NONE',  ( -0.000000000000000000, 1.000000000000000000, -0.000000000000000000 ) ) ;
#51685 = AXIS2_PLACEMENT_3D ( 'NONE', #81479, #101113, #91291 ) ;
#51686 = FACE_OUTER_BOUND ( 'NONE', #59228, .T. ) ;
#51687 = VERTEX_POINT ( 'NONE', #88768 ) ;
#51688 = ORIENTED_EDGE ( 'NONE', *, *, #64332, .F. ) ;
#51689 = CARTESIAN_POINT ( 'NONE',  ( -11.44999999999999751, 12.50000000000000000, 2.576566944158910744 ) ) ;
#51690 = DIRECTION ( 'NONE',  ( 0.000000000000000000, 0.000000000000000000, 1.000000000000000000 ) ) ;
#51691 = FACE_BOUND ( 'NONE', #20793, .T. ) ;
#51692 = LINE ( 'NONE', #98835, #5441 ) ;
#51693 = EDGE_CURVE ( 'NONE', #30477, #29851, #7614, .T. ) ;
#51694 = EDGE_CURVE ( 'NONE', #12100, #53692, #56610, .T. ) ;
#51695 = ORIENTED_EDGE ( 'NONE', *, *, #19844, .T. ) ;
#51696 = DIRECTION ( 'NONE',  ( 0.000000000000000000, 0.000000000000000000, -1.000000000000000000 ) ) ;
#51697 = CARTESIAN_POINT ( 'NONE',  ( 185.2083333333333144, -4.445597072760115509, -7.700000000000001954 ) ) ;
#51698 = ORIENTED_EDGE ( 'NONE', *, *, #61890, .T. ) ;
#51699 = FACE_OUTER_BOUND ( 'NONE', #118946, .T. ) ;
#51700 = CARTESIAN_POINT ( 'NONE',  ( 9.799999999999915445, 12.50000000000000000, 3.983716857408420964 ) ) ;
#51701 = EDGE_CURVE ( 'NONE', #100575, #43976, #77472, .T. ) ;
#51702 = CIRCLE ( 'NONE', #16069, 0.1000000000000000056 ) ;
#51703 = CARTESIAN_POINT ( 'NONE',  ( -14.59999999999998366, 2.500000000000000000, 0.09999999999999989453 ) ) ;
#51704 = DIRECTION ( 'NONE',  ( -0.000000000000000000, -1.000000000000000000, -0.000000000000000000 ) ) ;
#51705 = AXIS2_PLACEMENT_3D ( 'NONE', #84702, #122696, #122063 ) ;
#51706 = AXIS2_PLACEMENT_3D ( 'NONE', #22739, #14165, #113681 ) ;
#51707 = ORIENTED_EDGE ( 'NONE', *, *, #117578, .F. ) ;
#51708 = VECTOR ( 'NONE', #123083, 1000.000000000000000 ) ;
#51709 = VECTOR ( 'NONE', #116507, 1000.000000000000000 ) ;
#51710 = DIRECTION ( 'NONE',  ( 0.000000000000000000, 1.000000000000000000, 0.000000000000000000 ) ) ;
#51711 = CARTESIAN_POINT ( 'NONE',  ( -0.8500000000000390576, 12.50000000000000000, -6.495190528383302464 ) ) ;
#51712 = FACE_OUTER_BOUND ( 'NONE', #71107, .T. ) ;
#51713 = ORIENTED_EDGE ( 'NONE', *, *, #23708, .T. ) ;
#51714 = ORIENTED_EDGE ( 'NONE', *, *, #54126, .F. ) ;
#51715 = CONICAL_SURFACE ( 'NONE', #110206, 0.1000000000000000472, 0.003490658503988666988 ) ;
#51716 = CARTESIAN_POINT ( 'NONE',  ( -6.650000000000018119, 2.500000000000000000, -2.757883832488654097 ) ) ;
#51717 = ORIENTED_EDGE ( 'NONE', *, *, #119905, .T. ) ;
#51718 = CARTESIAN_POINT ( 'NONE',  ( 0.4499999999999569344, 2.500000000000000000, -2.165063509461101710 ) ) ;
#51719 = FACE_OUTER_BOUND ( 'NONE', #76573, .T. ) ;
#51721 = AXIS2_PLACEMENT_3D ( 'NONE', #56995, #100627, #10942 ) ;
#51720 = CIRCLE ( 'NONE', #116452, 0.06509327318403745899 ) ;
#51722 = DIRECTION ( 'NONE',  ( -4.274815082592931898E-19, -0.9999939076577903929, -0.003490651415223739937 ) ) ;
#51723 = ORIENTED_EDGE ( 'NONE', *, *, #101021, .F. ) ;
#51724 = DIRECTION ( 'NONE',  ( -0.000000000000000000, -1.000000000000000000, -0.000000000000000000 ) ) ;
#51725 = DIRECTION ( 'NONE',  ( -0.000000000000000000, 1.000000000000000000, -0.000000000000000000 ) ) ;
#51726 = DIRECTION ( 'NONE',  ( -0.000000000000000000, 1.000000000000000000, -0.000000000000000000 ) ) ;
#51727 =( BOUNDED_SURFACE ( )  B_SPLINE_SURFACE ( 3, 2, ( 
 ( #14167, #63938, #44283 ),
 ( #26591, #67793, #100957 ),
 ( #36427, #126725, #8225 ),
 ( #127373, #70223, #17386 ) ),
 .UNSPECIFIED., .F., .F., .F. ) 
 B_SPLINE_SURFACE_WITH_KNOTS ( ( 4, 4 ),
 ( 3, 3 ),
 ( -9.367506770274758310E-17, 0.002140783067917591091 ),
 ( 0.000000000000000000, 1.000000000000000000 ),
 .UNSPECIFIED. ) 
 GEOMETRIC_REPRESENTATION_ITEM ( )  RATIONAL_B_SPLINE_SURFACE ( (
 ( 1.000000000000000000, 0.7071067811865473507, 1.000000000000000000),
 ( 1.000000000000000000, 0.7083221562484182110, 1.000000000000000000),
 ( 1.000000000000000000, 0.7095583416414843470, 1.000000000000000000),
 ( 1.000000000000000000, 0.7108129113927461606, 1.000000000000000000) ) ) 
 REPRESENTATION_ITEM ( '' )  SURFACE ( )  );
#51728 = FACE_OUTER_BOUND ( 'NONE', #81477, .T. ) ;
#51729 = CARTESIAN_POINT ( 'NONE',  ( 149.5981739382431783, 2.500000000000000000, -1.703575533167231537 ) ) ;
#51730 = CARTESIAN_POINT ( 'NONE',  ( -12.69999999999999218, 2.500000000000000000, -0.3464101615137741286 ) ) ;
#51731 = ORIENTED_EDGE ( 'NONE', *, *, #97197, .T. ) ;
#51732 = ORIENTED_EDGE ( 'NONE', *, *, #87990, .T. ) ;
#51733 = CARTESIAN_POINT ( 'NONE',  ( 4.999999999999973355, 12.50000000000000000, -4.330127018922201643 ) ) ;
#51734 = ORIENTED_EDGE ( 'NONE', *, *, #119756, .F. ) ;
#51735 = CARTESIAN_POINT ( 'NONE',  ( 103.0433693783451616, 7.671897681384138856, 0.6785423624469419934 ) ) ;
#51737 = EDGE_LOOP ( 'NONE', ( #66316, #30079 ) ) ;
#51736 = VERTEX_POINT ( 'NONE', #97936 ) ;
#51738 = ORIENTED_EDGE ( 'NONE', *, *, #123563, .T. ) ;
#51739 = AXIS2_PLACEMENT_3D ( 'NONE', #4491, #64090, #96123 ) ;
#51740 = CARTESIAN_POINT ( 'NONE',  ( 11.84999999999990727, 2.500000000000000000, -2.611473670974877592 ) ) ;
#51741 = PLANE ( 'NONE',  #65308 ) ;
#51742 = DIRECTION ( 'NONE',  ( -0.000000000000000000, -1.000000000000000000, -0.000000000000000000 ) ) ;
#51743 = CARTESIAN_POINT ( 'NONE',  ( -0.8500000000000395017, 12.50000000000000000, 2.099970236277060032 ) ) ;
#51744 = PLANE ( 'NONE',  #64703 ) ;
#51745 = CARTESIAN_POINT ( 'NONE',  ( 179.5000000000000000, 0.000000000000000000, 6.000000000000000000 ) ) ;
#51746 = EDGE_CURVE ( 'NONE', #45239, #36155, #31507, .T. ) ;
#51747 = LINE ( 'NONE', #53034, #76892 ) ;
#51748 = LINE ( 'NONE', #83775, #57077 ) ;
#51749 = EDGE_CURVE ( 'NONE', #128241, #49718, #125574, .T. ) ;
#51750 = CARTESIAN_POINT ( 'NONE',  ( -2.950000000000029932, 12.50000000000000000, 2.165063509461097713 ) ) ;
#51752 = VERTEX_POINT ( 'NONE', #29219 ) ;
#51751 = CIRCLE ( 'NONE', #124904, 0.1000000000000002554 ) ;
#51753 = AXIS2_PLACEMENT_3D ( 'NONE', #36839, #14588, #95749 ) ;
#51754 = DIRECTION ( 'NONE',  ( 0.000000000000000000, -0.000000000000000000, 1.000000000000000000 ) ) ;
#51755 = ORIENTED_EDGE ( 'NONE', *, *, #22245, .T. ) ;
#51756 = EDGE_CURVE ( 'NONE', #21810, #3837, #69117, .T. ) ;
#51757 = EDGE_LOOP ( 'NONE', ( #38936, #29240, #23828, #69924 ) ) ;
#51758 = CARTESIAN_POINT ( 'NONE',  ( -11.25000000000000000, 12.50000000000000000, 2.922977105672686982 ) ) ;
#51759 = CARTESIAN_POINT ( 'NONE',  ( 9.999999999999948486, 2.500000000000000000, 4.430127018922196847 ) ) ;
#51760 = CARTESIAN_POINT ( 'NONE',  ( 10.84999999999990905, 2.500000000000000000, 2.857883832488649301 ) ) ;
#51762 = AXIS2_PLACEMENT_3D ( 'NONE', #91551, #71926, #41826 ) ;
#51761 = CONICAL_SURFACE ( 'NONE', #80999, 0.1000000000000002554, 0.003490658503988666988 ) ;
#51763 = CARTESIAN_POINT ( 'NONE',  ( 4.149999999999939959, 12.50000000000000000, -2.230156782645139391 ) ) ;
#51764 = CIRCLE ( 'NONE', #106132, 0.1000000000000002554 ) ;
#51765 = CARTESIAN_POINT ( 'NONE',  ( -12.89999999999999147, 2.500000000000000000, 4.330127018922196314 ) ) ;
#51766 = CARTESIAN_POINT ( 'NONE',  ( 5.199999999999935341, 12.50000000000000000, -3.983716857408426293 ) ) ;
#51767 = CARTESIAN_POINT ( 'NONE',  ( 10.84999999999991260, 12.50000000000000000, -2.857883832488653741 ) ) ;
#51768 = VERTEX_POINT ( 'NONE', #9565 ) ;
#51769 = VERTEX_POINT ( 'NONE', #49507 ) ;
#51770 = AXIS2_PLACEMENT_3D ( 'NONE', #21760, #110763, #40109 ) ;
#51771 = ORIENTED_EDGE ( 'NONE', *, *, #37048, .T. ) ;
#51772 = EDGE_CURVE ( 'NONE', #121109, #97069, #104645, .T. ) ;
#51773 = ORIENTED_EDGE ( 'NONE', *, *, #41958, .T. ) ;
#51774 = ORIENTED_EDGE ( 'NONE', *, *, #48276, .T. ) ;
#51775 = DIRECTION ( 'NONE',  ( 0.000000000000000000, 0.000000000000000000, -1.000000000000000000 ) ) ;
#51776 = CARTESIAN_POINT ( 'NONE',  ( 2.899999999999945732, 2.500000000000000000, -2.385244779468109755E-15 ) ) ;
#51777 = ADVANCED_FACE ( 'NONE', ( #12760 ), #73352, .T. ) ;
#51778 = AXIS2_PLACEMENT_3D ( 'NONE', #80849, #73581, #44795 ) ;
#51779 = DIRECTION ( 'NONE',  ( 0.000000000000000000, 0.000000000000000000, 1.000000000000000000 ) ) ;
#51780 = CARTESIAN_POINT ( 'NONE',  ( -10.84999999999999964, 2.500000000000000000, 5.902370205355745192 ) ) ;
#51781 = AXIS2_PLACEMENT_3D ( 'NONE', #83452, #1639, #91968 ) ;
#51782 = DIRECTION ( 'NONE',  ( -0.000000000000000000, -1.000000000000000000, -0.000000000000000000 ) ) ;
#51783 = ORIENTED_EDGE ( 'NONE', *, *, #83564, .F. ) ;
#51784 = CARTESIAN_POINT ( 'NONE',  ( -6.700000000000019718, 2.500000000000000000, -2.385244779468109755E-15 ) ) ;
#51785 = DIRECTION ( 'NONE',  ( 0.000000000000000000, 0.000000000000000000, 1.000000000000000000 ) ) ;
#51786 = EDGE_CURVE ( 'NONE', #53209, #74697, #72994, .T. ) ;
#51787 = EDGE_CURVE ( 'NONE', #18239, #61946, #58698, .T. ) ;
#51788 = CARTESIAN_POINT ( 'NONE',  ( -13.29999999999998828, 2.500000000000000000, 4.330127018922196314 ) ) ;
#51789 = ADVANCED_FACE ( 'NONE', ( #40325 ), #117246, .T. ) ;
#51790 = DIRECTION ( 'NONE',  ( 0.000000000000000000, 0.000000000000000000, 1.000000000000000000 ) ) ;
#51791 = CIRCLE ( 'NONE', #124937, 0.1000000000000002554 ) ;
#51792 = EDGE_CURVE ( 'NONE', #84812, #3294, #103094, .T. ) ;
#51793 = DIRECTION ( 'NONE',  ( 0.000000000000000000, 0.000000000000000000, -1.000000000000000000 ) ) ;
#51794 = ORIENTED_EDGE ( 'NONE', *, *, #58726, .T. ) ;
#51795 = CIRCLE ( 'NONE', #118581, 0.09999999999999999167 ) ;
#51796 = VERTEX_POINT ( 'NONE', #112285 ) ;
#51798 = VERTEX_POINT ( 'NONE', #70416 ) ;
#51797 = EDGE_CURVE ( 'NONE', #53658, #25872, #62543, .T. ) ;
#51799 = DIRECTION ( 'NONE',  ( 0.000000000000000000, 1.000000000000000000, 0.000000000000000000 ) ) ;
#51800 = ADVANCED_FACE ( 'NONE', ( #82829 ), #30516, .T. ) ;
#51801 = CIRCLE ( 'NONE', #93651, 0.06509327318403745899 ) ;
#51802 = ORIENTED_EDGE ( 'NONE', *, *, #89115, .F. ) ;
#51803 = CIRCLE ( 'NONE', #3668, 0.1000000000000002554 ) ;
#51804 = DIRECTION ( 'NONE',  ( 0.000000000000000000, -0.9999939076577903929, 0.003490651415223739937 ) ) ;
#51805 = LINE ( 'NONE', #113280, #25196 ) ;
#51806 = EDGE_CURVE ( 'NONE', #121634, #67054, #71062, .T. ) ;
#51807 = CONICAL_SURFACE ( 'NONE', #101976, 0.1000000000000000472, 0.003490658503988666988 ) ;
#51808 = EDGE_CURVE ( 'NONE', #75922, #25044, #75409, .T. ) ;
#51809 = EDGE_LOOP ( 'NONE', ( #31884, #71690, #11135, #94131 ) ) ;
#51810 = DIRECTION ( 'NONE',  ( 0.000000000000000000, 0.000000000000000000, 1.000000000000000000 ) ) ;
#51812 = CIRCLE ( 'NONE', #124959, 0.1000000000000002554 ) ;
#51811 = CARTESIAN_POINT ( 'NONE',  ( 12.49999999999990408, 2.500000000000000000, 5.122947341949749323 ) ) ;
#51813 = DIRECTION ( 'NONE',  ( 0.000000000000000000, 0.000000000000000000, 1.000000000000000000 ) ) ;
#51814 = PLANE ( 'NONE',  #129320 ) ;
#51815 = ADVANCED_FACE ( 'NONE', ( #122737 ), #12700, .T. ) ;
#51817 = CIRCLE ( 'NONE', #118700, 0.1000000000000002554 ) ;
#51816 = AXIS2_PLACEMENT_3D ( 'NONE', #23747, #24385, #13903 ) ;
#51818 = DIRECTION ( 'NONE',  ( 0.000000000000000000, 0.000000000000000000, 1.000000000000000000 ) ) ;
#51819 = VERTEX_POINT ( 'NONE', #12125 ) ;
#51820 = ORIENTED_EDGE ( 'NONE', *, *, #26758, .F. ) ;
#51821 = FACE_OUTER_BOUND ( 'NONE', #71666, .T. ) ;
#51822 = CARTESIAN_POINT ( 'NONE',  ( -4.800000000000022915, 2.500000000000000000, -0.2464101615137783419 ) ) ;
#51823 = DIRECTION ( 'NONE',  ( 0.000000000000000000, 0.000000000000000000, -1.000000000000000000 ) ) ;
#51824 = FACE_OUTER_BOUND ( 'NONE', #47416, .T. ) ;
#51825 = EDGE_LOOP ( 'NONE', ( #14871, #83628 ) ) ;
#51826 = ORIENTED_EDGE ( 'NONE', *, *, #110301, .F. ) ;
#51827 = CARTESIAN_POINT ( 'NONE',  ( -0.6000000000000383915, 2.500000000000000000, -3.883716857408426648 ) ) ;
#51828 = DIRECTION ( 'NONE',  ( 0.000000000000000000, -0.000000000000000000, 1.000000000000000000 ) ) ;
#51829 = DIRECTION ( 'NONE',  ( 0.000000000000000000, -0.000000000000000000, 1.000000000000000000 ) ) ;
#51830 = LINE ( 'NONE', #33487, #36318 ) ;
#51831 = EDGE_LOOP ( 'NONE', ( #52184, #103908 ) ) ;
#51832 = DIRECTION ( 'NONE',  ( 0.000000000000000000, -0.000000000000000000, 1.000000000000000000 ) ) ;
#51833 = CARTESIAN_POINT ( 'NONE',  ( -1.650000000000034772, 12.50000000000000000, 1.472243186433545459 ) ) ;
#51834 = VERTEX_POINT ( 'NONE', #52076 ) ;
#51835 = CIRCLE ( 'NONE', #20541, 0.06509327318403745899 ) ;
#51836 = DIRECTION ( 'NONE',  ( 0.000000000000000000, 0.000000000000000000, -1.000000000000000000 ) ) ;
#51837 = EDGE_LOOP ( 'NONE', ( #127075, #57780 ) ) ;
#51838 = DIRECTION ( 'NONE',  ( -0.000000000000000000, -1.000000000000000000, -0.000000000000000000 ) ) ;
#51839 = AXIS2_PLACEMENT_3D ( 'NONE', #96968, #29530, #89094 ) ;
#51840 = ORIENTED_EDGE ( 'NONE', *, *, #40519, .F. ) ;
#51841 = ADVANCED_FACE ( 'NONE', ( #91986 ), #81675, .T. ) ;
#51842 = AXIS2_PLACEMENT_3D ( 'NONE', #97675, #38119, #47299 ) ;
#51843 = EDGE_LOOP ( 'NONE', ( #6197, #98843 ) ) ;
#51844 = DIRECTION ( 'NONE',  ( -4.274815082592931898E-19, -0.9999939076577903929, -0.003490651415223739937 ) ) ;
#51845 = CARTESIAN_POINT ( 'NONE',  ( 9.599999999999914380, 2.500000000000000000, -5.022947341949754119 ) ) ;
#51846 = EDGE_CURVE ( 'NONE', #87255, #124518, #64942, .T. ) ;
#51847 = ORIENTED_EDGE ( 'NONE', *, *, #84264, .F. ) ;
#51848 = EDGE_LOOP ( 'NONE', ( #84859, #80965 ) ) ;
#51849 = FACE_OUTER_BOUND ( 'NONE', #52911, .T. ) ;
#51850 = CARTESIAN_POINT ( 'NONE',  ( -1.250000000000037526, 12.50000000000000000, -1.472243186433550122 ) ) ;
#51851 = AXIS2_PLACEMENT_3D ( 'NONE', #112612, #109550, #113236 ) ;
#51852 = CARTESIAN_POINT ( 'NONE',  ( 187.1718750003414016, 9.264065473108010111E-16, -7.564683531250000925 ) ) ;
#51853 = CARTESIAN_POINT ( 'NONE',  ( 184.9427083336747160, -6.551208109652278289, 3.782341765624995134 ) ) ;
#51854 = AXIS2_PLACEMENT_3D ( 'NONE', #20904, #2534, #71953 ) ;
#51855 = PLANE ( 'NONE',  #114347 ) ;
#51856 = CARTESIAN_POINT ( 'NONE',  ( -12.09999999999999609, 2.500000000000000000, -0.09999999999999827083 ) ) ;
#51857 = CARTESIAN_POINT ( 'NONE',  ( 3.349999999999943689, 2.500000000000000000, 2.065063509461097624 ) ) ;
#51858 = DIRECTION ( 'NONE',  ( -4.274815082592931898E-19, -0.9999939076577903929, -0.003490651415223739937 ) ) ;
#51859 = DIRECTION ( 'NONE',  ( -4.274815082592931898E-19, -0.9999939076577903929, -0.003490651415223739937 ) ) ;
#51860 = AXIS2_PLACEMENT_3D ( 'NONE', #87741, #116561, #108033 ) ;
#51861 = VERTEX_POINT ( 'NONE', #120164 ) ;
#51862 = ORIENTED_EDGE ( 'NONE', *, *, #67390, .T. ) ;
#51863 = DIRECTION ( 'NONE',  ( 0.000000000000000000, 0.000000000000000000, 1.000000000000000000 ) ) ;
#51864 = ORIENTED_EDGE ( 'NONE', *, *, #68158, .T. ) ;
#51865 = DIRECTION ( 'NONE',  ( 0.000000000000000000, 1.000000000000000000, 0.000000000000000000 ) ) ;
#51866 = DIRECTION ( 'NONE',  ( 0.000000000000000000, 0.000000000000000000, -1.000000000000000000 ) ) ;
#51867 = AXIS2_PLACEMENT_3D ( 'NONE', #63044, #70931, #51313 ) ;
#51868 = CARTESIAN_POINT ( 'NONE',  ( -5.650000000000019895, 2.500000000000000000, 6.148780366869520009 ) ) ;
#51870 = ORIENTED_EDGE ( 'NONE', *, *, #74124, .T. ) ;
#51869 = ORIENTED_EDGE ( 'NONE', *, *, #39649, .F. ) ;
#51871 = FACE_BOUND ( 'NONE', #106285, .T. ) ;
#51872 = ORIENTED_EDGE ( 'NONE', *, *, #58291, .F. ) ;
#51873 = CARTESIAN_POINT ( 'NONE',  ( 14.14999999999989555, 2.500000000000000000, 2.165063509461097713 ) ) ;
#51874 = CARTESIAN_POINT ( 'NONE',  ( 1.049999999999954081, 2.500000000000000000, -6.148780366869526226 ) ) ;
#51875 = DIRECTION ( 'NONE',  ( 0.000000000000000000, 0.000000000000000000, -1.000000000000000000 ) ) ;
#51876 = CONICAL_SURFACE ( 'NONE', #125020, 0.1000000000000002554, 0.003490658503988666988 ) ;
#51877 = CARTESIAN_POINT ( 'NONE',  ( 8.749999999999953815, 12.50000000000000000, -2.165063509461101710 ) ) ;
#51878 = FACE_OUTER_BOUND ( 'NONE', #63722, .T. ) ;
#51879 = CARTESIAN_POINT ( 'NONE',  ( -3.350000000000028955, 2.500000000000000000, -2.165063509461101710 ) ) ;
#51880 = CONICAL_SURFACE ( 'NONE', #125023, 0.1000000000000002554, 0.003490658503988666988 ) ;
#51881 = FACE_OUTER_BOUND ( 'NONE', #2132, .T. ) ;
#51882 = CARTESIAN_POINT ( 'NONE',  ( 129.5000000000000000, 0.000000000000000000, 0.000000000000000000 ) ) ;
#51883 = CARTESIAN_POINT ( 'NONE',  ( 9.199999999999915801, 12.50000000000000000, -4.330127018922201643 ) ) ;
#51884 = FACE_OUTER_BOUND ( 'NONE', #117492, .T. ) ;
#51885 = AXIS2_PLACEMENT_3D ( 'NONE', #196, #92453, #13886 ) ;
#51886 = CIRCLE ( 'NONE', #68590, 0.1000000000000002554 ) ;
#51887 = FACE_OUTER_BOUND ( 'NONE', #55791, .T. ) ;
#51888 = EDGE_CURVE ( 'NONE', #60383, #75351, #20679, .T. ) ;
#51889 = ORIENTED_EDGE ( 'NONE', *, *, #96751, .F. ) ;
#51891 = VERTEX_POINT ( 'NONE', #50778 ) ;
#51890 = VECTOR ( 'NONE', #17147, 1000.000000000000000 ) ;
#51892 = ORIENTED_EDGE ( 'NONE', *, *, #80299, .F. ) ;
#51893 = CARTESIAN_POINT ( 'NONE',  ( -0.8500000000000395017, 12.50000000000000000, 2.165063509461097713 ) ) ;
#51894 = ORIENTED_EDGE ( 'NONE', *, *, #73769, .T. ) ;
#51895 = CARTESIAN_POINT ( 'NONE',  ( 7.049999999999930544, 2.500000000000000000, -6.595190528383302109 ) ) ;
#51896 = CARTESIAN_POINT ( 'NONE',  ( 7.699999999999925571, 2.500000000000000000, 4.083716857408420609 ) ) ;
#51898 = ORIENTED_EDGE ( 'NONE', *, *, #78394, .F. ) ;
#51897 = ORIENTED_EDGE ( 'NONE', *, *, #111689, .F. ) ;
#51900 = ORIENTED_EDGE ( 'NONE', *, *, #124039, .F. ) ;
#51899 = AXIS2_PLACEMENT_3D ( 'NONE', #4047, #42724, #104190 ) ;
#51901 = PLANE ( 'NONE',  #8296 ) ;
#51902 = DIRECTION ( 'NONE',  ( 0.000000000000000000, -0.000000000000000000, 1.000000000000000000 ) ) ;
#51903 = DIRECTION ( 'NONE',  ( 0.000000000000000000, 0.000000000000000000, -1.000000000000000000 ) ) ;
#51904 = LINE ( 'NONE', #99067, #91019 ) ;
#51905 = CARTESIAN_POINT ( 'NONE',  ( -2.100000000000034284, 2.500000000000000000, -2.385244779468109755E-15 ) ) ;
#51906 = EDGE_CURVE ( 'NONE', #98420, #28344, #90701, .T. ) ;
#51907 = FACE_OUTER_BOUND ( 'NONE', #111615, .T. ) ;
#51908 = ADVANCED_FACE ( 'NONE', ( #72362 ), #80891, .T. ) ;
#51909 = ORIENTED_EDGE ( 'NONE', *, *, #13087, .F. ) ;
#51910 = DIRECTION ( 'NONE',  ( 1.000000000000000000, 0.000000000000000000, 0.000000000000000000 ) ) ;
#51911 = VERTEX_POINT ( 'NONE', #31156 ) ;
#51913 = VECTOR ( 'NONE', #78709, 1000.000000000000000 ) ;
#51912 = VECTOR ( 'NONE', #74776, 1000.000000000000000 ) ;
#51914 = VERTEX_POINT ( 'NONE', #1662 ) ;
#51915 = ORIENTED_EDGE ( 'NONE', *, *, #16450, .T. ) ;
#51916 = FACE_OUTER_BOUND ( 'NONE', #100706, .T. ) ;
#51917 = VERTEX_POINT ( 'NONE', #110962 ) ;
#51918 = ADVANCED_FACE ( 'NONE', ( #21304 ), #117153, .T. ) ;
#51919 = VERTEX_POINT ( 'NONE', #105680 ) ;
#51920 = ORIENTED_EDGE ( 'NONE', *, *, #105281, .F. ) ;
#51921 =( NAMED_UNIT ( * ) SI_UNIT ( $, .STERADIAN. ) SOLID_ANGLE_UNIT ( ) );
#51922 = CARTESIAN_POINT ( 'NONE',  ( 194.5000000000000000, 0.000000000000000000, -4.000000000000000000 ) ) ;
#51923 = DIRECTION ( 'NONE',  ( 0.000000000000000000, 1.000000000000000000, 0.000000000000000000 ) ) ;
#51924 = LINE ( 'NONE', #62389, #77728 ) ;
#51925 = DIRECTION ( 'NONE',  ( -0.000000000000000000, -1.000000000000000000, -0.000000000000000000 ) ) ;
#51927 = AXIS2_PLACEMENT_3D ( 'NONE', #109471, #59752, #12543 ) ;
#51926 = FACE_OUTER_BOUND ( 'NONE', #45803, .T. ) ;
#51928 = DIRECTION ( 'NONE',  ( -0.000000000000000000, 1.000000000000000000, -0.000000000000000000 ) ) ;
#51929 = ORIENTED_EDGE ( 'NONE', *, *, #19368, .F. ) ;
#51931 = DIRECTION ( 'NONE',  ( -4.274815082592931898E-19, -0.9999939076577903929, -0.003490651415223739937 ) ) ;
#51930 = AXIS2_PLACEMENT_3D ( 'NONE', #53712, #13778, #73344 ) ;
#51932 = EDGE_LOOP ( 'NONE', ( #61507, #32056, #26556, #93126 ) ) ;
#51933 = DIRECTION ( 'NONE',  ( 0.000000000000000000, 0.000000000000000000, -1.000000000000000000 ) ) ;
#51934 = AXIS2_PLACEMENT_3D ( 'NONE', #41909, #121732, #84393 ) ;
#51935 = ORIENTED_EDGE ( 'NONE', *, *, #15312, .T. ) ;
#51936 = CARTESIAN_POINT ( 'NONE',  ( -7.100000000000013856, 2.500000000000000000, 5.022947341949748790 ) ) ;
#51937 = ORIENTED_EDGE ( 'NONE', *, *, #15615, .F. ) ;
#51938 = CIRCLE ( 'NONE', #54071, 0.1000000000000002554 ) ;
#51939 = CARTESIAN_POINT ( 'NONE',  ( 183.9010416670080588, -4.367472073101519747, 7.564683531249999149 ) ) ;
#51940 = AXIS2_PLACEMENT_3D ( 'NONE', #23569, #3290, #73304 ) ;
#51941 = EDGE_CURVE ( 'NONE', #99488, #97111, #75556, .T. ) ;
#51942 = LINE ( 'NONE', #91860, #71870 ) ;
#51943 = ORIENTED_EDGE ( 'NONE', *, *, #38862, .F. ) ;
#51944 = ORIENTED_EDGE ( 'NONE', *, *, #116787, .F. ) ;
#51945 = DIRECTION ( 'NONE',  ( -0.000000000000000000, -1.000000000000000000, -0.000000000000000000 ) ) ;
#51946 = FACE_OUTER_BOUND ( 'NONE', #121510, .T. ) ;
#51947 = ADVANCED_FACE ( 'NONE', ( #24537 ), #102597, .T. ) ;
#51948 = DIRECTION ( 'NONE',  ( -4.274815082592931898E-19, -0.9999939076577903929, -0.003490651415223739937 ) ) ;
#51949 = DIRECTION ( 'NONE',  ( 0.000000000000000000, -0.9999939076577903929, 0.003490651415223739937 ) ) ;
#51951 = ADVANCED_FACE ( 'NONE', ( #66389 ), #62901, .T. ) ;
#51950 = VECTOR ( 'NONE', #39138, 1000.000000000000000 ) ;
#51952 = FACE_OUTER_BOUND ( 'NONE', #80534, .T. ) ;
#51953 = CIRCLE ( 'NONE', #127258, 0.09999999999999999167 ) ;
#51954 = ORIENTED_EDGE ( 'NONE', *, *, #34948, .F. ) ;
#51955 = CARTESIAN_POINT ( 'NONE',  ( 7.499999999999927169, 2.500000000000000000, 3.737306695894644371 ) ) ;
#51956 = ADVANCED_FACE ( 'NONE', ( #95218 ), #74930, .T. ) ;
#51957 = EDGE_CURVE ( 'NONE', #77408, #27361, #15984, .T. ) ;
#51958 = EDGE_CURVE ( 'NONE', #4494, #69514, #42071, .T. ) ;
#51959 = ADVANCED_FACE ( 'NONE', ( #5520 ), #98471, .T. ) ;
#51960 = ORIENTED_EDGE ( 'NONE', *, *, #24741, .F. ) ;
#51961 = DIRECTION ( 'NONE',  ( 0.000000000000000000, -0.000000000000000000, 1.000000000000000000 ) ) ;
#51963 = AXIS2_PLACEMENT_3D ( 'NONE', #7744, #77764, #117680 ) ;
#51962 = FACE_OUTER_BOUND ( 'NONE', #52965, .T. ) ;
#51964 = EDGE_CURVE ( 'NONE', #97550, #34514, #29545, .T. ) ;
#51965 = DIRECTION ( 'NONE',  ( 0.000000000000000000, 0.000000000000000000, -1.000000000000000000 ) ) ;
#51966 = CARTESIAN_POINT ( 'NONE',  ( 10.84999999999990905, 2.500000000000000000, 1.472243186433545459 ) ) ;
#51967 = DIRECTION ( 'NONE',  ( -4.274815082592931898E-19, -0.9999939076577903929, -0.003490651415223739937 ) ) ;
#51968 = CARTESIAN_POINT ( 'NONE',  ( 165.4999999999999716, 0.000000000000000000, 2.000000000000000000 ) ) ;
#51969 = CARTESIAN_POINT ( 'NONE',  ( 0.5999999999999551248, 12.50000000000000000, -4.611443907251940644 ) ) ;
#51970 = ORIENTED_EDGE ( 'NONE', *, *, #68161, .F. ) ;
#51971 = ADVANCED_FACE ( 'NONE', ( #74290 ), #92219, .T. ) ;
#51972 = CONICAL_SURFACE ( 'NONE', #79069, 0.1000000000000002554, 0.003490658503988666988 ) ;
#51973 = CARTESIAN_POINT ( 'NONE',  ( -5.400000000000023448, 2.500000000000000000, -4.330127018922201643 ) ) ;
#51974 = DIRECTION ( 'NONE',  ( 0.000000000000000000, 0.000000000000000000, 1.000000000000000000 ) ) ;
#51975 = CARTESIAN_POINT ( 'NONE',  ( 3.749999999999942268, 12.50000000000000000, -5.802370205355749988 ) ) ;
#51976 = ORIENTED_EDGE ( 'NONE', *, *, #123535, .F. ) ;
#51977 = ORIENTED_EDGE ( 'NONE', *, *, #50834, .F. ) ;
#51978 = CONICAL_SURFACE ( 'NONE', #39387, 0.1000000000000002554, 0.003490658503988666988 ) ;
#51979 = CARTESIAN_POINT ( 'NONE',  ( 9.349999999999916156, 12.50000000000000000, -2.446380397790840266 ) ) ;
#51980 = AXIS2_PLACEMENT_3D ( 'NONE', #63564, #74660, #113948 ) ;
#51981 = ORIENTED_EDGE ( 'NONE', *, *, #68294, .F. ) ;
#51982 = EDGE_LOOP ( 'NONE', ( #92094, #108763, #109899, #127018 ) ) ;
#51983 = DIRECTION ( 'NONE',  ( 0.000000000000000000, -0.9999939076577903929, 0.003490651415223739937 ) ) ;
#51984 = EDGE_LOOP ( 'NONE', ( #51239, #15569 ) ) ;
#51986 = CONICAL_SURFACE ( 'NONE', #129368, 0.1000000000000002554, 0.003490658503988666988 ) ;
#51985 = DIRECTION ( 'NONE',  ( -0.000000000000000000, 1.000000000000000000, -0.000000000000000000 ) ) ;
#51987 = DIRECTION ( 'NONE',  ( 0.000000000000000000, 0.000000000000000000, -1.000000000000000000 ) ) ;
#51988 = CARTESIAN_POINT ( 'NONE',  ( 11.64999999999990798, 12.50000000000000000, 5.737276932171707422 ) ) ;
#51989 = ORIENTED_EDGE ( 'NONE', *, *, #46038, .F. ) ;
#51990 = CARTESIAN_POINT ( 'NONE',  ( 9.599999999999914380, 12.50000000000000000, 4.330127018922196314 ) ) ;
#51991 = AXIS2_PLACEMENT_3D ( 'NONE', #117799, #18322, #58270 ) ;
#51992 = FACE_OUTER_BOUND ( 'NONE', #15116, .T. ) ;
#51993 = ORIENTED_EDGE ( 'NONE', *, *, #48516, .F. ) ;
#51995 = AXIS2_PLACEMENT_3D ( 'NONE', #94785, #113790, #33933 ) ;
#51994 = CIRCLE ( 'NONE', #125153, 0.1000000000000000056 ) ;
#51997 = EDGE_LOOP ( 'NONE', ( #122165, #81476, #28725, #93208 ) ) ;
#51996 = EDGE_CURVE ( 'NONE', #89246, #113013, #46256, .T. ) ;
#51998 = ORIENTED_EDGE ( 'NONE', *, *, #31119, .T. ) ;
#51999 = DIRECTION ( 'NONE',  ( -4.274815082592931898E-19, -0.9999939076577903929, -0.003490651415223739937 ) ) ;
#52000 = FACE_OUTER_BOUND ( 'NONE', #1126, .T. ) ;
#52001 = LINE ( 'NONE', #80817, #8744 ) ;
#52002 = FACE_BOUND ( 'NONE', #107066, .T. ) ;
#52003 = EDGE_LOOP ( 'NONE', ( #126311, #19170, #83675, #109104 ) ) ;
#52004 = CARTESIAN_POINT ( 'NONE',  ( 10.19999999999991580, 12.50000000000000000, -0.4115034346978157509 ) ) ;
#52005 = DIRECTION ( 'NONE',  ( 0.000000000000000000, 1.000000000000000000, 0.000000000000000000 ) ) ;
#52006 = EDGE_LOOP ( 'NONE', ( #13827, #81416 ) ) ;
#52007 = EDGE_CURVE ( 'NONE', #12189, #87317, #93924, .T. ) ;
#52008 = CARTESIAN_POINT ( 'NONE',  ( -13.94999999999998863, 2.500000000000000000, 2.611473670974877148 ) ) ;
#52009 = DIRECTION ( 'NONE',  ( -4.274815082592931898E-19, -0.9999939076577903929, -0.003490651415223739937 ) ) ;
#52010 = CARTESIAN_POINT ( 'NONE',  ( 7.499999999999960032, 2.500000000000000000, -2.276824562219559311E-15 ) ) ;
#52011 = FACE_OUTER_BOUND ( 'NONE', #13286, .T. ) ;
#52012 = VECTOR ( 'NONE', #115087, 1000.000000000000000 ) ;
#52013 = CARTESIAN_POINT ( 'NONE',  ( 1.649999999999950617, 12.50000000000000000, 2.165063509461097713 ) ) ;
#52014 = DIRECTION ( 'NONE',  ( 0.000000000000000000, -0.9999939076577903929, 0.003490651415223739937 ) ) ;
#52015 = DIRECTION ( 'NONE',  ( 0.000000000000000000, 1.000000000000000000, 0.000000000000000000 ) ) ;
#52016 = VECTOR ( 'NONE', #81720, 1000.000000000000000 ) ;
#52017 = AXIS2_PLACEMENT_3D ( 'NONE', #69630, #19898, #120027 ) ;
#52018 = ORIENTED_EDGE ( 'NONE', *, *, #46641, .T. ) ;
#52019 = ORIENTED_EDGE ( 'NONE', *, *, #48287, .T. ) ;
#52020 = AXIS2_PLACEMENT_3D ( 'NONE', #105829, #123525, #85543 ) ;
#52021 = ORIENTED_EDGE ( 'NONE', *, *, #118862, .F. ) ;
#52022 = ORIENTED_EDGE ( 'NONE', *, *, #76603, .F. ) ;
#52023 = CARTESIAN_POINT ( 'NONE',  ( 6.249999999999928946, 2.500000000000000000, 2.957883832488649389 ) ) ;
#52024 = CARTESIAN_POINT ( 'NONE',  ( -2.700000000000030376, 12.50000000000000000, 3.983716857408420964 ) ) ;
#52025 = ORIENTED_EDGE ( 'NONE', *, *, #86845, .F. ) ;
#52026 = FACE_BOUND ( 'NONE', #1079, .T. ) ;
#52027 = CARTESIAN_POINT ( 'NONE',  ( 6.249999999999932498, 12.50000000000000000, 5.802370205355744659 ) ) ;
#52028 = DIRECTION ( 'NONE',  ( 0.000000000000000000, 1.000000000000000000, 0.000000000000000000 ) ) ;
#52029 = AXIS2_PLACEMENT_3D ( 'NONE', #8768, #109576, #29099 ) ;
#52030 = CIRCLE ( 'NONE', #97981, 0.06509327318403745899 ) ;
#52031 = DIRECTION ( 'NONE',  ( -0.000000000000000000, -1.000000000000000000, -0.000000000000000000 ) ) ;
#52032 = CIRCLE ( 'NONE', #118916, 0.1000000000000002554 ) ;
#52033 = DIRECTION ( 'NONE',  ( 0.000000000000000000, 1.000000000000000000, 0.000000000000000000 ) ) ;
#52034 = DIRECTION ( 'NONE',  ( 0.000000000000000000, 0.000000000000000000, 1.000000000000000000 ) ) ;
#52035 = CARTESIAN_POINT ( 'NONE',  ( -6.050000000000017586, 2.500000000000000000, 6.048780366869520364 ) ) ;
#52036 = LINE ( 'NONE', #42881, #20384 ) ;
#52037 = DIRECTION ( 'NONE',  ( 0.000000000000000000, 0.000000000000000000, -1.000000000000000000 ) ) ;
#52038 = DIRECTION ( 'NONE',  ( 0.000000000000000000, 0.000000000000000000, 1.000000000000000000 ) ) ;
#52039 = AXIS2_PLACEMENT_3D ( 'NONE', #93360, #86087, #123449 ) ;
#52040 = ORIENTED_EDGE ( 'NONE', *, *, #4789, .T. ) ;
#52042 = ADVANCED_FACE ( 'NONE', ( #114209 ), #15337, .T. ) ;
#52041 = CIRCLE ( 'NONE', #60466, 0.06509327318403745899 ) ;
#52043 = ORIENTED_EDGE ( 'NONE', *, *, #88300, .F. ) ;
#52044 = VERTEX_POINT ( 'NONE', #35027 ) ;
#52045 = ORIENTED_EDGE ( 'NONE', *, *, #58926, .F. ) ;
#52046 = ORIENTED_EDGE ( 'NONE', *, *, #96960, .T. ) ;
#52047 = VERTEX_POINT ( 'NONE', #55290 ) ;
#52048 = CARTESIAN_POINT ( 'NONE',  ( 7.499999999999925393, 12.50000000000000000, 5.022947341949748790 ) ) ;
#52049 = ORIENTED_EDGE ( 'NONE', *, *, #74349, .F. ) ;
#52050 = ORIENTED_EDGE ( 'NONE', *, *, #88238, .T. ) ;
#52052 = EDGE_CURVE ( 'NONE', #59320, #73842, #6512, .T. ) ;
#52051 = CIRCLE ( 'NONE', #29073, 0.06509327318403743123 ) ;
#52053 = FACE_OUTER_BOUND ( 'NONE', #23070, .T. ) ;
#52054 = CARTESIAN_POINT ( 'NONE',  ( 13.80679872452937396, -2.499999999999552802, 7.946844944429471980 ) ) ;
#52055 = CARTESIAN_POINT ( 'NONE',  ( -1.250000000000037970, 2.500000000000000000, 2.857883832488649301 ) ) ;
#52056 = DIRECTION ( 'NONE',  ( 0.000000000000000000, -0.000000000000000000, 1.000000000000000000 ) ) ;
#52057 = CIRCLE ( 'NONE', #49913, 0.06509327318403745899 ) ;
#52058 = EDGE_CURVE ( 'NONE', #23160, #98765, #127739, .T. ) ;
#52059 = EDGE_CURVE ( 'NONE', #108189, #28707, #76225, .T. ) ;
#52060 = VERTEX_POINT ( 'NONE', #125314 ) ;
#52061 = DIRECTION ( 'NONE',  ( 0.000000000000000000, 0.000000000000000000, -1.000000000000000000 ) ) ;
#52062 = ORIENTED_EDGE ( 'NONE', *, *, #71907, .F. ) ;
#52063 = VERTEX_POINT ( 'NONE', #35650 ) ;
#52064 = AXIS2_PLACEMENT_3D ( 'NONE', #49522, #8919, #8281 ) ;
#52065 = DIRECTION ( 'NONE',  ( 0.000000000000000000, 1.000000000000000000, 0.000000000000000000 ) ) ;
#52066 = EDGE_CURVE ( 'NONE', #75250, #75194, #23267, .T. ) ;
#52067 = DIRECTION ( 'NONE',  ( -0.000000000000000000, 1.000000000000000000, -0.000000000000000000 ) ) ;
#52068 = EDGE_CURVE ( 'NONE', #65715, #38578, #119402, .T. ) ;
#52069 = VERTEX_POINT ( 'NONE', #78161 ) ;
#52070 = AXIS2_PLACEMENT_3D ( 'NONE', #59832, #48695, #119352 ) ;
#52071 = ORIENTED_EDGE ( 'NONE', *, *, #75858, .F. ) ;
#52072 = FACE_OUTER_BOUND ( 'NONE', #76029, .T. ) ;
#52073 = AXIS2_PLACEMENT_3D ( 'NONE', #75941, #66765, #86401 ) ;
#52074 = CARTESIAN_POINT ( 'NONE',  ( -13.29999999999998828, 2.500000000000000000, 4.430127018922196847 ) ) ;
#52075 = DIRECTION ( 'NONE',  ( -0.000000000000000000, 1.000000000000000000, -0.000000000000000000 ) ) ;
#52076 = CARTESIAN_POINT ( 'NONE',  ( -7.900000000000011013, 12.50000000000000000, 4.395220292106234439 ) ) ;
#52077 = CARTESIAN_POINT ( 'NONE',  ( -4.600000000000024514, 2.500000000000000000, 3.637306695894644726 ) ) ;
#52078 = ORIENTED_EDGE ( 'NONE', *, *, #49462, .F. ) ;
#52079 = DIRECTION ( 'NONE',  ( 0.000000000000000000, -0.000000000000000000, 1.000000000000000000 ) ) ;
#52080 = ORIENTED_EDGE ( 'NONE', *, *, #28024, .T. ) ;
#52081 = CARTESIAN_POINT ( 'NONE',  ( 17.50000000000000000, 2.499999999999999556, -3.333333333333329485 ) ) ;
#52083 = CIRCLE ( 'NONE', #18618, 0.09999999999999982514 ) ;
#52082 = AXIS2_PLACEMENT_3D ( 'NONE', #97655, #7978, #78015 ) ;
#52084 = CARTESIAN_POINT ( 'NONE',  ( -10.40000000000000391, 12.50000000000000000, -3.702399969078682851 ) ) ;
#52085 = CARTESIAN_POINT ( 'NONE',  ( -7.900000000000014566, 2.500000000000000000, 0.5928203230275495006 ) ) ;
#52086 = CIRCLE ( 'NONE', #39584, 0.06509327318403745899 ) ;
#52087 = CARTESIAN_POINT ( 'NONE',  ( -10.60000000000000320, 12.50000000000000000, -3.918623584224384615 ) ) ;
#52088 = DIRECTION ( 'NONE',  ( 0.000000000000000000, 0.000000000000000000, 1.000000000000000000 ) ) ;
#52089 = VERTEX_POINT ( 'NONE', #117395 ) ;
#52090 = FACE_OUTER_BOUND ( 'NONE', #67644, .T. ) ;
#52091 = CONICAL_SURFACE ( 'NONE', #37430, 0.1000000000000000472, 0.003490658503988666988 ) ;
#52092 = LINE ( 'NONE', #22640, #125944 ) ;
#52093 = ORIENTED_EDGE ( 'NONE', *, *, #116162, .T. ) ;
#52094 = ORIENTED_EDGE ( 'NONE', *, *, #117072, .T. ) ;
#52095 = EDGE_LOOP ( 'NONE', ( #96240, #96387 ) ) ;
#52096 = CARTESIAN_POINT ( 'NONE',  ( 2.500000000000002220, -2.750000000000000444, 10.00000000000000178 ) ) ;
#52097 = DIRECTION ( 'NONE',  ( -0.000000000000000000, -1.000000000000000000, -0.000000000000000000 ) ) ;
#52098 = CARTESIAN_POINT ( 'NONE',  ( 8.349999999999919709, 12.50000000000000000, -1.472243186433550122 ) ) ;
#52100 = EDGE_CURVE ( 'NONE', #15328, #30332, #35803, .T. ) ;
#52099 = FACE_OUTER_BOUND ( 'NONE', #101032, .T. ) ;
#52101 = LINE ( 'NONE', #25198, #96984 ) ;
#52102 = DIRECTION ( 'NONE',  ( 0.000000000000000000, 0.000000000000000000, 1.000000000000000000 ) ) ;
#52103 = CARTESIAN_POINT ( 'NONE',  ( 5.199999999999933564, 2.500000000000000000, 0.4464101615137735513 ) ) ;
#52104 = ADVANCED_FACE ( 'NONE', ( #119353 ), #126615, .T. ) ;
#52105 = AXIS2_PLACEMENT_3D ( 'NONE', #42205, #9015, #48972 ) ;
#52106 = EDGE_CURVE ( 'NONE', #31758, #115693, #28412, .T. ) ;
#52107 = EDGE_CURVE ( 'NONE', #10471, #50344, #77550, .T. ) ;
#52108 = EDGE_CURVE ( 'NONE', #126779, #89530, #8111, .T. ) ;
#52109 = CIRCLE ( 'NONE', #106477, 0.09999999999999982514 ) ;
#52110 = AXIS2_PLACEMENT_3D ( 'NONE', #29402, #98120, #28760 ) ;
#52111 = EDGE_LOOP ( 'NONE', ( #101636, #33699, #64668, #74661, #113552, #106522, #33375, #81195, #37257, #30188, #54161, #68466 ) ) ;
#52112 = ADVANCED_FACE ( 'NONE', ( #6792 ), #94280, .T. ) ;
#52113 = CARTESIAN_POINT ( 'NONE',  ( 8.149999999999920419, 12.50000000000000000, -2.446380397790840266 ) ) ;
#52114 = CARTESIAN_POINT ( 'NONE',  ( -9.350000000000004974, 12.50000000000000000, 6.148780366869520897 ) ) ;
#52115 = DIRECTION ( 'NONE',  ( 0.000000000000000000, 1.000000000000000000, 0.000000000000000000 ) ) ;
#52116 = DIRECTION ( 'NONE',  ( -0.000000000000000000, 1.000000000000000000, -0.000000000000000000 ) ) ;
#52117 = ORIENTED_EDGE ( 'NONE', *, *, #122085, .F. ) ;
#52119 = ADVANCED_FACE ( 'NONE', ( #8740 ), #71293, .T. ) ;
#52118 = AXIS2_PLACEMENT_3D ( 'NONE', #37114, #58042, #48210 ) ;
#52120 = CARTESIAN_POINT ( 'NONE',  ( -1.250000000000037970, 12.50000000000000000, 2.857883832488649301 ) ) ;
#52121 = AXIS2_PLACEMENT_3D ( 'NONE', #96957, #87135, #115961 ) ;
#52122 = EDGE_CURVE ( 'NONE', #97182, #104775, #16972, .T. ) ;
#52123 = DIRECTION ( 'NONE',  ( -4.274815082592931898E-19, -0.9999939076577903929, -0.003490651415223739937 ) ) ;
#52125 = VERTEX_POINT ( 'NONE', #109549 ) ;
#52124 = DIRECTION ( 'NONE',  ( -0.000000000000000000, -1.000000000000000000, -0.000000000000000000 ) ) ;
#52126 = AXIS2_PLACEMENT_3D ( 'NONE', #85307, #54544, #125244 ) ;
#52127 = EDGE_LOOP ( 'NONE', ( #98198, #121992 ) ) ;
#52128 = CARTESIAN_POINT ( 'NONE',  ( -13.09999999999999254, 2.500000000000000000, -0.3464101615137741286 ) ) ;
#52129 = CONICAL_SURFACE ( 'NONE', #12400, 0.1000000000000002554, 0.003490658503988666988 ) ;
#52130 = CIRCLE ( 'NONE', #31308, 0.06509327318403745899 ) ;
#52131 = ORIENTED_EDGE ( 'NONE', *, *, #3242, .F. ) ;
#52132 = ORIENTED_EDGE ( 'NONE', *, *, #80307, .F. ) ;
#52133 = DIRECTION ( 'NONE',  ( 0.000000000000000000, 1.000000000000000000, 0.000000000000000000 ) ) ;
#52134 = CARTESIAN_POINT ( 'NONE',  ( 20.80581321129326255, 0.6997403544423165256, -4.161084241360471836 ) ) ;
#52135 = LINE ( 'NONE', #41041, #88143 ) ;
#52136 = FACE_OUTER_BOUND ( 'NONE', #78608, .T. ) ;
#52137 = ORIENTED_EDGE ( 'NONE', *, *, #28925, .F. ) ;
#52138 = DIRECTION ( 'NONE',  ( 0.000000000000000000, 0.000000000000000000, 1.000000000000000000 ) ) ;
#52139 = VERTEX_POINT ( 'NONE', #48697 ) ;
#52140 = CONICAL_SURFACE ( 'NONE', #85579, 0.09999999999999982514, 0.003490658503988666988 ) ;
#52141 = CARTESIAN_POINT ( 'NONE',  ( 17.49100792770887125, 2.144659849951620068, 4.220823783472687829 ) ) ;
#52142 = CARTESIAN_POINT ( 'NONE',  ( 186.5312500006828031, 9.429780353434619030E-16, -7.700000000000000178 ) ) ;
#52143 = EDGE_LOOP ( 'NONE', ( #104936, #120431 ) ) ;
#52144 = ORIENTED_EDGE ( 'NONE', *, *, #24906, .F. ) ;
#52145 = ORIENTED_EDGE ( 'NONE', *, *, #111580, .T. ) ;
#52146 = EDGE_LOOP ( 'NONE', ( #42169, #26229, #93399, #85795 ) ) ;
#52147 = CARTESIAN_POINT ( 'NONE',  ( 6.649999999999930189, 12.50000000000000000, -2.857883832488653741 ) ) ;
#52148 = CARTESIAN_POINT ( 'NONE',  ( 6.449999999999928235, 2.500000000000000000, 2.511473670974873507 ) ) ;
#52149 = FACE_OUTER_BOUND ( 'NONE', #119153, .T. ) ;
#52150 = FACE_BOUND ( 'NONE', #53558, .T. ) ;
#52151 = ORIENTED_EDGE ( 'NONE', *, *, #24614, .F. ) ;
#52152 = CARTESIAN_POINT ( 'NONE',  ( 184.4895833340161460, -4.445597072760115509, -7.700000000000001954 ) ) ;
#52153 = CIRCLE ( 'NONE', #12425, 0.1000000000000002554 ) ;
#52154 = FACE_OUTER_BOUND ( 'NONE', #125038, .T. ) ;
#52155 = PLANE ( 'NONE',  #127474 ) ;
#52156 = EDGE_CURVE ( 'NONE', #47060, #42654, #52524, .T. ) ;
#52157 = DIRECTION ( 'NONE',  ( 0.000000000000000000, 0.000000000000000000, -1.000000000000000000 ) ) ;
#52158 = DIRECTION ( 'NONE',  ( -4.274815082592931898E-19, -0.9999939076577903929, -0.003490651415223739937 ) ) ;
#52159 = UNCERTAINTY_MEASURE_WITH_UNIT (LENGTH_MEASURE( 1.000000000000000082E-05 ), #103580, 'distance_accuracy_value', 'NONE');
#52160 = CIRCLE ( 'NONE', #85599, 0.06509327318403745899 ) ;
#52161 = CARTESIAN_POINT ( 'NONE',  ( 11.84999999999990727, 2.500000000000000000, 6.248780366869520542 ) ) ;
#52162 = CARTESIAN_POINT ( 'NONE',  ( 12.69999999999989804, 2.500000000000000000, 0.3464101615137735735 ) ) ;
#52164 = CIRCLE ( 'NONE', #6175, 0.06509327318403745899 ) ;
#52163 = CONICAL_SURFACE ( 'NONE', #12440, 0.1000000000000002554, 0.003490658503988666988 ) ;
#52165 = EDGE_LOOP ( 'NONE', ( #74430, #36069 ) ) ;
#52166 = ORIENTED_EDGE ( 'NONE', *, *, #33888, .T. ) ;
#52167 = VERTEX_POINT ( 'NONE', #57216 ) ;
#52168 = ORIENTED_EDGE ( 'NONE', *, *, #55600, .T. ) ;
#52169 = EDGE_LOOP ( 'NONE', ( #97257, #80397 ) ) ;
#52170 = LINE ( 'NONE', #80348, #87792 ) ;
#52171 = AXIS2_PLACEMENT_3D ( 'NONE', #91145, #79403, #49957 ) ;
#52172 = LINE ( 'NONE', #31890, #27810 ) ;
#52173 = ORIENTED_EDGE ( 'NONE', *, *, #118537, .T. ) ;
#52174 = FACE_BOUND ( 'NONE', #123127, .T. ) ;
#52175 = DIRECTION ( 'NONE',  ( -0.000000000000000000, -1.000000000000000000, -0.000000000000000000 ) ) ;
#52176 = COLOUR_RGB ( '', 0.66274510, 0.83137255, 0.94901961) ;
#52177 = EDGE_LOOP ( 'NONE', ( #17609, #2516 ) ) ;
#52178 = FACE_OUTER_BOUND ( 'NONE', #41227, .T. ) ;
#52179 = CARTESIAN_POINT ( 'NONE',  ( 5.849999999999933920, 2.500000000000000000, -2.265063509461101798 ) ) ;
#52180 = CARTESIAN_POINT ( 'NONE',  ( 7.899999999999924860, 2.500000000000000000, 4.330127018922196314 ) ) ;
#52181 = ORIENTED_EDGE ( 'NONE', *, *, #119539, .T. ) ;
#52182 = CARTESIAN_POINT ( 'NONE',  ( 3.349999999999945466, 2.500000000000000000, -2.857883832488653741 ) ) ;
#52183 = ORIENTED_EDGE ( 'NONE', *, *, #236, .F. ) ;
#52184 = ORIENTED_EDGE ( 'NONE', *, *, #78366, .F. ) ;
#52185 = ORIENTED_EDGE ( 'NONE', *, *, #54070, .T. ) ;
#52186 = VECTOR ( 'NONE', #99033, 1000.000000000000000 ) ;
#52187 = DIRECTION ( 'NONE',  ( -0.000000000000000000, 1.000000000000000000, -0.000000000000000000 ) ) ;
#52188 = FACE_OUTER_BOUND ( 'NONE', #100938, .T. ) ;
#52189 = ORIENTED_EDGE ( 'NONE', *, *, #62285, .F. ) ;
#52190 = DIRECTION ( 'NONE',  ( 0.000000000000000000, 0.000000000000000000, 1.000000000000000000 ) ) ;
#52191 = AXIS2_PLACEMENT_3D ( 'NONE', #23797, #44071, #83978 ) ;
#52192 = EDGE_CURVE ( 'NONE', #126749, #93502, #110994, .T. ) ;
#52193 = DIRECTION ( 'NONE',  ( 0.000000000000000000, 1.000000000000000000, 0.000000000000000000 ) ) ;
#52194 = CARTESIAN_POINT ( 'NONE',  ( 0.1999999999999571565, 2.500000000000000000, 4.083716857408420609 ) ) ;
#52195 = DIRECTION ( 'NONE',  ( 0.000000000000000000, 0.000000000000000000, 1.000000000000000000 ) ) ;
#52196 = CARTESIAN_POINT ( 'NONE',  ( 186.7395833340161175, 4.445597072760117285, 7.699999999999999289 ) ) ;
#52197 = ORIENTED_EDGE ( 'NONE', *, *, #100282, .T. ) ;
#52198 = EDGE_CURVE ( 'NONE', #84669, #112250, #54561, .T. ) ;
#52199 = DIRECTION ( 'NONE',  ( 0.000000000000000000, -1.000000000000000000, 0.000000000000000000 ) ) ;
#52200 = ADVANCED_FACE ( 'NONE', ( #56558 ), #87310, .F. ) ;
#52202 = EDGE_LOOP ( 'NONE', ( #111258, #114077, #29061, #16288 ) ) ;
#52201 = CONICAL_SURFACE ( 'NONE', #123222, 0.1000000000000002554, 0.003490658503988666988 ) ;
#52203 = LINE ( 'NONE', #62029, #93071 ) ;
#52205 = CIRCLE ( 'NONE', #29235, 0.06509327318403745899 ) ;
#52204 = VECTOR ( 'NONE', #17278, 1000.000000000000114 ) ;
#52206 = ORIENTED_EDGE ( 'NONE', *, *, #86096, .T. ) ;
#52207 = DIRECTION ( 'NONE',  ( -0.000000000000000000, 1.000000000000000000, -0.000000000000000000 ) ) ;
#52208 = EDGE_LOOP ( 'NONE', ( #2816, #67146 ) ) ;
#52209 = FACE_OUTER_BOUND ( 'NONE', #3183, .T. ) ;
#52210 = CARTESIAN_POINT ( 'NONE',  ( 10.39999999999991509, 2.500000000000000000, 0.6928203230275494784 ) ) ;
#52211 = EDGE_CURVE ( 'NONE', #53342, #118322, #113158, .T. ) ;
#52212 = ADVANCED_FACE ( 'NONE', ( #96477 ), #25317, .T. ) ;
#52213 = CARTESIAN_POINT ( 'NONE',  ( 12.69999999999990337, 12.50000000000000000, 4.048810130592458201 ) ) ;
#52214 = EDGE_CURVE ( 'NONE', #62130, #68394, #128572, .T. ) ;
#52215 = CARTESIAN_POINT ( 'NONE',  ( -4.550000000000022915, 12.50000000000000000, 2.165063509461097713 ) ) ;
#52216 = ADVANCED_FACE ( 'NONE', ( #38236 ), #50465, .T. ) ;
#52217 = CARTESIAN_POINT ( 'NONE',  ( 184.4999999999999432, -7.324530227482785705, -2.036292321216437884 ) ) ;
#52218 = AXIS2_PLACEMENT_3D ( 'NONE', #43321, #114612, #64230 ) ;
#52219 = ORIENTED_EDGE ( 'NONE', *, *, #100494, .F. ) ;
#52220 = ORIENTED_EDGE ( 'NONE', *, *, #27070, .T. ) ;
#52221 = AXIS2_PLACEMENT_3D ( 'NONE', #124563, #74812, #122627 ) ;
#52222 = DIRECTION ( 'NONE',  ( -0.000000000000000000, 1.000000000000000000, -0.000000000000000000 ) ) ;
#52223 = DIRECTION ( 'NONE',  ( 0.000000000000000000, 0.000000000000000000, -1.000000000000000000 ) ) ;
#52224 = DIRECTION ( 'NONE',  ( 0.000000000000000000, 0.000000000000000000, -1.000000000000000000 ) ) ;
#52226 = VERTEX_POINT ( 'NONE', #29067 ) ;
#52225 = ORIENTED_EDGE ( 'NONE', *, *, #70323, .F. ) ;
#52227 = ORIENTED_EDGE ( 'NONE', *, *, #124426, .T. ) ;
#52228 = EDGE_CURVE ( 'NONE', #86441, #14402, #10669, .T. ) ;
#52229 = FACE_OUTER_BOUND ( 'NONE', #25841, .T. ) ;
#52230 = CIRCLE ( 'NONE', #8383, 0.06509327318403745899 ) ;
#52231 = ORIENTED_EDGE ( 'NONE', *, *, #30771, .F. ) ;
#52232 = LINE ( 'NONE', #91502, #94657 ) ;
#52233 = DIRECTION ( 'NONE',  ( 0.000000000000000000, 1.000000000000000000, 0.000000000000000000 ) ) ;
#52234 = DIRECTION ( 'NONE',  ( 0.000000000000000000, 1.000000000000000000, 0.000000000000000000 ) ) ;
#52235 = ORIENTED_EDGE ( 'NONE', *, *, #60088, .T. ) ;
#52236 = DIRECTION ( 'NONE',  ( 0.000000000000000000, 0.000000000000000000, 1.000000000000000000 ) ) ;
#52237 = DIRECTION ( 'NONE',  ( 0.000000000000000000, 0.000000000000000000, 1.000000000000000000 ) ) ;
#52238 = CARTESIAN_POINT ( 'NONE',  ( -8.350000000000013856, 2.500000000000000000, 2.065063509461097624 ) ) ;
#52239 = CIRCLE ( 'NONE', #127448, 0.06509327318403743123 ) ;
#52240 = DIRECTION ( 'NONE',  ( -0.000000000000000000, -1.000000000000000000, -0.000000000000000000 ) ) ;
#52241 = LINE ( 'NONE', #50960, #26988 ) ;
#52242 = ORIENTED_EDGE ( 'NONE', *, *, #57458, .F. ) ;
#52243 = PLANE ( 'NONE',  #57133 ) ;
#52244 = CARTESIAN_POINT ( 'NONE',  ( 23.99354682433153130, -2.839181451644544385, 2.508508607398769907 ) ) ;
#52245 = VERTEX_POINT ( 'NONE', #91192 ) ;
#52246 = ORIENTED_EDGE ( 'NONE', *, *, #52949, .T. ) ;
#52247 = EDGE_CURVE ( 'NONE', #11408, #126604, #67158, .T. ) ;
#52248 = CARTESIAN_POINT ( 'NONE',  ( 187.0468750003414300, -8.734944146203032389, -1.604583208406768146E-15 ) ) ;
#52249 = CARTESIAN_POINT ( 'NONE',  ( 8.149999999999923972, 2.500000000000000000, -6.148780366869526226 ) ) ;
#52250 = DIRECTION ( 'NONE',  ( -0.000000000000000000, 1.000000000000000000, -0.000000000000000000 ) ) ;
#52251 = DIRECTION ( 'NONE',  ( 0.000000000000000000, 0.000000000000000000, 1.000000000000000000 ) ) ;
#52252 = CARTESIAN_POINT ( 'NONE',  ( 5.399999999999932854, 2.500000000000000000, 3.737306695894644371 ) ) ;
#52253 = DIRECTION ( 'NONE',  ( 0.000000000000000000, 0.000000000000000000, 1.000000000000000000 ) ) ;
#52254 = PLANE ( 'NONE',  #105511 ) ;
#52255 = CARTESIAN_POINT ( 'NONE',  ( 9.549999999999915445, 2.500000000000000000, 6.495190528383297135 ) ) ;
#52256 = ADVANCED_FACE ( 'NONE', ( #21822 ), #41472, .T. ) ;
#52257 = ADVANCED_FACE ( 'NONE', ( #30361 ), #48319, .T. ) ;
#52258 = DIRECTION ( 'NONE',  ( 0.000000000000000000, 0.000000000000000000, 1.000000000000000000 ) ) ;
#52259 = ORIENTED_EDGE ( 'NONE', *, *, #89963, .T. ) ;
#52260 = ORIENTED_EDGE ( 'NONE', *, *, #96781, .F. ) ;
#52261 = ADVANCED_FACE ( 'NONE', ( #61088 ), #19053, .T. ) ;
#52262 = AXIS2_PLACEMENT_3D ( 'NONE', #69699, #51371, #129295 ) ;
#52263 = ORIENTED_EDGE ( 'NONE', *, *, #79473, .F. ) ;
#52264 = EDGE_LOOP ( 'NONE', ( #87127, #122172, #34016, #55217 ) ) ;
#52265 = ADVANCED_FACE ( 'NONE', ( #121296 ), #65118, .T. ) ;
#52266 = FACE_OUTER_BOUND ( 'NONE', #108873, .T. ) ;
#52267 = DIRECTION ( 'NONE',  ( 0.000000000000000000, 0.000000000000000000, 1.000000000000000000 ) ) ;
#52268 = ADVANCED_FACE ( 'NONE', ( #101006 ), #69323, .T. ) ;
#52271 = EDGE_LOOP ( 'NONE', ( #62070, #65321, #33209, #78970 ) ) ;
#52270 = VECTOR ( 'NONE', #65488, 1000.000000000000000 ) ;
#52269 = CONICAL_SURFACE ( 'NONE', #29288, 0.09999999999999999167, 0.003490658503988666988 ) ;
#52272 = ADVANCED_FACE ( 'NONE', ( #2157 ), #29626, .T. ) ;
#52273 = CARTESIAN_POINT ( 'NONE',  ( -5.850000000000019185, 2.500000000000000000, 6.495190528383297135 ) ) ;
#52274 = EDGE_CURVE ( 'NONE', #91490, #48067, #51924, .T. ) ;
#52275 = DIRECTION ( 'NONE',  ( 0.000000000000000000, -0.000000000000000000, 1.000000000000000000 ) ) ;
#52277 = ORIENTED_EDGE ( 'NONE', *, *, #38969, .F. ) ;
#52276 = DIRECTION ( 'NONE',  ( -0.000000000000000000, 1.000000000000000000, -0.000000000000000000 ) ) ;
#52278 = CARTESIAN_POINT ( 'NONE',  ( -8.300000000000011369, 2.500000000000000000, -4.330127018922201643 ) ) ;
#52279 = EDGE_CURVE ( 'NONE', #83089, #81926, #32305, .T. ) ;
#52280 = DIRECTION ( 'NONE',  ( 0.000000000000000000, 0.000000000000000000, 1.000000000000000000 ) ) ;
#52281 = EDGE_LOOP ( 'NONE', ( #42552, #41889 ) ) ;
#52282 = ORIENTED_EDGE ( 'NONE', *, *, #63931, .F. ) ;
#52283 = ORIENTED_EDGE ( 'NONE', *, *, #68048, .F. ) ;
#52284 = ORIENTED_EDGE ( 'NONE', *, *, #85625, .F. ) ;
#52285 = DIRECTION ( 'NONE',  ( 0.000000000000000000, 0.000000000000000000, 1.000000000000000000 ) ) ;
#52286 = CARTESIAN_POINT ( 'NONE',  ( 7.299999999999926104, 2.500000000000000000, -0.3464101615137782364 ) ) ;
#52287 = CARTESIAN_POINT ( 'NONE',  ( 5.799999999999933209, 2.500000000000000000, -2.385244779468109755E-15 ) ) ;
#52288 = DIRECTION ( 'NONE',  ( 0.000000000000000000, 0.000000000000000000, 1.000000000000000000 ) ) ;
#52289 = AXIS2_PLACEMENT_3D ( 'NONE', #25482, #92963, #24215 ) ;
#52290 = ORIENTED_EDGE ( 'NONE', *, *, #96371, .T. ) ;
#52291 = AXIS2_PLACEMENT_3D ( 'NONE', #14018, #113521, #45444 ) ;
#52292 = DIRECTION ( 'NONE',  ( -0.000000000000000000, -1.000000000000000000, -0.000000000000000000 ) ) ;
#52293 = ORIENTED_EDGE ( 'NONE', *, *, #54873, .T. ) ;
#52294 = CARTESIAN_POINT ( 'NONE',  ( -6.250000000000021316, 2.500000000000000000, -5.702370205355749455 ) ) ;
#52295 = CARTESIAN_POINT ( 'NONE',  ( 15.79999999999989058, 2.500000000000000000, -0.1000000000000023925 ) ) ;
#52296 = DIRECTION ( 'NONE',  ( 0.000000000000000000, 1.000000000000000000, 0.000000000000000000 ) ) ;
#52297 = DIRECTION ( 'NONE',  ( 0.000000000000000000, 0.000000000000000000, 1.000000000000000000 ) ) ;
#52298 = VERTEX_POINT ( 'NONE', #72210 ) ;
#52299 = ORIENTED_EDGE ( 'NONE', *, *, #82251, .T. ) ;
#52300 = VERTEX_POINT ( 'NONE', #112131 ) ;
#52301 = DIRECTION ( 'NONE',  ( -4.274815082592931898E-19, -0.9999939076577903929, -0.003490651415223739937 ) ) ;
#52302 = DIRECTION ( 'NONE',  ( 0.000000000000000000, 1.000000000000000000, 0.000000000000000000 ) ) ;
#52303 = CARTESIAN_POINT ( 'NONE',  ( 9.149999999999915090, 2.500000000000000000, 6.595190528383296780 ) ) ;
#52304 = FACE_BOUND ( 'NONE', #90334, .T. ) ;
#52305 = CARTESIAN_POINT ( 'NONE',  ( 1.699999999999951994, 12.50000000000000000, -4.330127018922201643 ) ) ;
#52306 = CARTESIAN_POINT ( 'NONE',  ( -4.800000000000024691, 12.50000000000000000, 4.676537180435972552 ) ) ;
#52307 = LINE ( 'NONE', #61498, #89635 ) ;
#52308 = AXIS2_PLACEMENT_3D ( 'NONE', #28944, #79339, #100258 ) ;
#52309 = CIRCLE ( 'NONE', #89859, 0.06509327318403741736 ) ;
#52310 = EDGE_CURVE ( 'NONE', #61474, #113589, #4555, .T. ) ;
#52311 = DIRECTION ( 'NONE',  ( 0.000000000000000000, 0.000000000000000000, 1.000000000000000000 ) ) ;
#52312 = DIRECTION ( 'NONE',  ( -0.000000000000000000, -1.000000000000000000, -0.000000000000000000 ) ) ;
#52313 = LINE ( 'NONE', #32700, #19765 ) ;
#52314 = ORIENTED_EDGE ( 'NONE', *, *, #89115, .T. ) ;
#52315 = CONICAL_SURFACE ( 'NONE', #64915, 0.09999999999999999167, 0.003490658503988666988 ) ;
#52316 = CARTESIAN_POINT ( 'NONE',  ( 8.149999999999923972, 2.500000000000000000, -6.048780366869526581 ) ) ;
#52317 = DIRECTION ( 'NONE',  ( 0.000000000000000000, 0.000000000000000000, 1.000000000000000000 ) ) ;
#52318 = AXIS2_PLACEMENT_3D ( 'NONE', #5922, #85785, #36060 ) ;
#52319 = ORIENTED_EDGE ( 'NONE', *, *, #12389, .T. ) ;
#52320 = VERTEX_POINT ( 'NONE', #42768 ) ;
#52321 = CARTESIAN_POINT ( 'NONE',  ( 4.149999999999941735, 12.50000000000000000, -1.407149913249512663 ) ) ;
#52322 = EDGE_CURVE ( 'NONE', #98563, #22598, #120653, .T. ) ;
#52323 = CARTESIAN_POINT ( 'NONE',  ( 9.349999999999919709, 2.500000000000000000, -6.841600689897078702 ) ) ;
#52324 = FACE_BOUND ( 'NONE', #62984, .T. ) ;
#52325 = DIRECTION ( 'NONE',  ( 0.000000000000000000, 0.000000000000000000, 1.000000000000000000 ) ) ;
#52326 = EDGE_LOOP ( 'NONE', ( #16171, #80839 ) ) ;
#52327 = DIRECTION ( 'NONE',  ( 0.000000000000000000, 0.000000000000000000, 1.000000000000000000 ) ) ;
#52328 = CARTESIAN_POINT ( 'NONE',  ( 0.1999999999999627909, 2.500000000000000000, 0.3464101615137758494 ) ) ;
#52329 = ORIENTED_EDGE ( 'NONE', *, *, #4311, .F. ) ;
#52330 = FACE_OUTER_BOUND ( 'NONE', #57973, .T. ) ;
#52331 = DIRECTION ( 'NONE',  ( 0.000000000000000000, -0.000000000000000000, 1.000000000000000000 ) ) ;
#52332 = AXIS2_PLACEMENT_3D ( 'NONE', #39702, #27258, #48198 ) ;
#52333 = ORIENTED_EDGE ( 'NONE', *, *, #129595, .T. ) ;
#52334 = CARTESIAN_POINT ( 'NONE',  ( 1.649999999999951950, 12.50000000000000000, -7.188010851410854052 ) ) ;
#52335 = AXIS2_PLACEMENT_3D ( 'NONE', #82979, #43711, #81670 ) ;
#52336 = CARTESIAN_POINT ( 'NONE',  ( 9.999999999999914735, 2.500000000000000000, 0.6928203230275494784 ) ) ;
#52337 = EDGE_LOOP ( 'NONE', ( #125291, #24258 ) ) ;
#52338 = ADVANCED_FACE ( 'NONE', ( #11343 ), #42099, .T. ) ;
#52339 = CARTESIAN_POINT ( 'NONE',  ( 1.849999999999950573, 2.500000000000000000, -1.818653347947326138 ) ) ;
#52341 = VECTOR ( 'NONE', #59258, 1000.000000000000000 ) ;
#52340 = CONICAL_SURFACE ( 'NONE', #119241, 0.09999999999999982514, 0.003490658503988666988 ) ;
#52342 = CARTESIAN_POINT ( 'NONE',  ( 11.04999999999991012, 2.500000000000000000, -1.718653347947326049 ) ) ;
#52343 = DIRECTION ( 'NONE',  ( 0.000000000000000000, 1.000000000000000000, 0.000000000000000000 ) ) ;
#52344 = ORIENTED_EDGE ( 'NONE', *, *, #95085, .F. ) ;
#52345 = ORIENTED_EDGE ( 'NONE', *, *, #108524, .F. ) ;
#52346 = CARTESIAN_POINT ( 'NONE',  ( -2.499999999999996003, 2.500000000000000000, -2.276824562219559311E-15 ) ) ;
#52347 = EDGE_CURVE ( 'NONE', #118274, #80116, #6606, .T. ) ;
#52348 = EDGE_LOOP ( 'NONE', ( #108075, #2776 ) ) ;
#52349 = CARTESIAN_POINT ( 'NONE',  ( 9.149999999999916866, 2.500000000000000000, -2.857883832488653741 ) ) ;
#52350 = DIRECTION ( 'NONE',  ( 0.000000000000000000, 0.000000000000000000, 1.000000000000000000 ) ) ;
#52351 = CARTESIAN_POINT ( 'NONE',  ( -2.100000000000034728, 12.50000000000000000, 4.330127018922196314 ) ) ;
#52352 = EDGE_LOOP ( 'NONE', ( #6048, #128255, #106246, #114048 ) ) ;
#52353 = LINE ( 'NONE', #81805, #26559 ) ;
#52354 = DIRECTION ( 'NONE',  ( 0.000000000000000000, 1.000000000000000000, 0.000000000000000000 ) ) ;
#52355 = CARTESIAN_POINT ( 'NONE',  ( 13.09999999999990195, 2.500000000000000000, 4.676537180435972552 ) ) ;
#52356 = EDGE_CURVE ( 'NONE', #19644, #16889, #48412, .T. ) ;
#52357 = EDGE_CURVE ( 'NONE', #46368, #110642, #119507, .T. ) ;
#52358 = DIRECTION ( 'NONE',  ( -0.000000000000000000, -1.000000000000000000, -0.000000000000000000 ) ) ;
#52359 = DIRECTION ( 'NONE',  ( -0.000000000000000000, -1.000000000000000000, -0.000000000000000000 ) ) ;
#52360 = EDGE_CURVE ( 'NONE', #92622, #36126, #23350, .T. ) ;
#52361 = ADVANCED_FACE ( 'NONE', ( #43399 ), #125783, .T. ) ;
#52362 = ADVANCED_FACE ( 'NONE', ( #4089 ), #42154, .T. ) ;
#52363 = PLANE ( 'NONE',  #45314 ) ;
#52364 = EDGE_LOOP ( 'NONE', ( #21764, #127613, #36215, #14151 ) ) ;
#52365 = VERTEX_POINT ( 'NONE', #84595 ) ;
#52366 = DIRECTION ( 'NONE',  ( 0.000000000000000000, -0.000000000000000000, 1.000000000000000000 ) ) ;
#52367 = ORIENTED_EDGE ( 'NONE', *, *, #127433, .T. ) ;
#52368 = DIRECTION ( 'NONE',  ( 0.000000000000000000, 1.000000000000000000, 0.000000000000000000 ) ) ;
#52370 = EDGE_LOOP ( 'NONE', ( #100921, #86266, #111536, #2364 ) ) ;
#52369 = ORIENTED_EDGE ( 'NONE', *, *, #67577, .F. ) ;
#52371 = ORIENTED_EDGE ( 'NONE', *, *, #71860, .F. ) ;
#52372 = EDGE_CURVE ( 'NONE', #32930, #122361, #13258, .T. ) ;
#52373 = CARTESIAN_POINT ( 'NONE',  ( 0.3999999999999559464, 12.50000000000000000, -4.395220292106239768 ) ) ;
#52374 = ADVANCED_FACE ( 'NONE', ( #83932 ), #4714, .T. ) ;
#52375 = AXIS2_PLACEMENT_3D ( 'NONE', #18442, #28268, #86534 ) ;
#52376 = DIRECTION ( 'NONE',  ( 0.000000000000000000, 0.000000000000000000, -1.000000000000000000 ) ) ;
#52377 = EDGE_CURVE ( 'NONE', #103313, #114323, #113249, .T. ) ;
#52378 = AXIS2_PLACEMENT_3D ( 'NONE', #93442, #83632, #123531 ) ;
#52379 = DIRECTION ( 'NONE',  ( 0.000000000000000000, 0.000000000000000000, 1.000000000000000000 ) ) ;
#52380 = DIRECTION ( 'NONE',  ( 0.000000000000000000, -0.000000000000000000, 1.000000000000000000 ) ) ;
#52381 = DIRECTION ( 'NONE',  ( 0.000000000000000000, 1.000000000000000000, 0.000000000000000000 ) ) ;
#52382 = DIRECTION ( 'NONE',  ( -0.000000000000000000, -1.000000000000000000, -0.000000000000000000 ) ) ;
#52383 = DIRECTION ( 'NONE',  ( -4.274815082592931898E-19, -0.9999939076577903929, -0.003490651415223739937 ) ) ;
#52384 = FACE_OUTER_BOUND ( 'NONE', #90890, .T. ) ;
#52386 = CONICAL_SURFACE ( 'NONE', #125535, 0.1000000000000002554, 0.003490658503988666988 ) ;
#52385 = DIRECTION ( 'NONE',  ( -0.000000000000000000, -1.000000000000000000, -0.000000000000000000 ) ) ;
#52387 = ORIENTED_EDGE ( 'NONE', *, *, #48389, .T. ) ;
#52388 = DIRECTION ( 'NONE',  ( 0.000000000000000000, 0.000000000000000000, 1.000000000000000000 ) ) ;
#52389 = ORIENTED_EDGE ( 'NONE', *, *, #114389, .T. ) ;
#52390 = EDGE_LOOP ( 'NONE', ( #15828, #58530 ) ) ;
#52391 = DIRECTION ( 'NONE',  ( 0.000000000000000000, 0.000000000000000000, 1.000000000000000000 ) ) ;
#52392 = DIRECTION ( 'NONE',  ( 0.000000000000000000, 0.000000000000000000, -1.000000000000000000 ) ) ;
#52393 = CARTESIAN_POINT ( 'NONE',  ( 1.649999999999949729, 2.500000000000000000, 5.802370205355744659 ) ) ;
#52394 = AXIS2_PLACEMENT_3D ( 'NONE', #41980, #93654, #81258 ) ;
#52395 = CARTESIAN_POINT ( 'NONE',  ( 10.59999999999991260, 12.50000000000000000, -0.2813168883297409439 ) ) ;
#52396 = AXIS2_PLACEMENT_3D ( 'NONE', #35251, #83696, #26708 ) ;
#52398 = DIRECTION ( 'NONE',  ( 0.000000000000000000, 0.000000000000000000, 1.000000000000000000 ) ) ;
#52397 = PRODUCT ( 'Rechargeable Battery Pack Module', 'Rechargeable Battery Pack Module', '', ( #107919 ) ) ;
#52399 = CARTESIAN_POINT ( 'NONE',  ( -4.800000000000022915, 12.50000000000000000, -0.3464101615137783474 ) ) ;
#52400 = DIRECTION ( 'NONE',  ( 0.000000000000000000, 0.000000000000000000, -1.000000000000000000 ) ) ;
#52401 = ORIENTED_EDGE ( 'NONE', *, *, #44369, .F. ) ;
#52402 = AXIS2_PLACEMENT_3D ( 'NONE', #98651, #129451, #39774 ) ;
#52403 = ORIENTED_EDGE ( 'NONE', *, *, #3486, .F. ) ;
#52404 = ORIENTED_EDGE ( 'NONE', *, *, #51792, .F. ) ;
#52405 = AXIS2_PLACEMENT_3D ( 'NONE', #11747, #90959, #62160 ) ;
#52406 = ORIENTED_EDGE ( 'NONE', *, *, #33951, .F. ) ;
#52407 = ADVANCED_FACE ( 'NONE', ( #54479 ), #94399, .T. ) ;
#52408 = EDGE_LOOP ( 'NONE', ( #1569, #20747, #64247, #123419 ) ) ;
#52409 = CARTESIAN_POINT ( 'NONE',  ( 15.19999999999989093, 12.50000000000000000, 0.3464101615137735735 ) ) ;
#52410 = CARTESIAN_POINT ( 'NONE',  ( -8.350000000000012079, 12.50000000000000000, 1.537336459617582918 ) ) ;
#52411 = EDGE_CURVE ( 'NONE', #60152, #2388, #21214, .T. ) ;
#52412 = DIRECTION ( 'NONE',  ( 0.000000000000000000, 1.000000000000000000, 0.000000000000000000 ) ) ;
#52413 = DIRECTION ( 'NONE',  ( 0.000000000000000000, 0.000000000000000000, -1.000000000000000000 ) ) ;
#52414 = EDGE_CURVE ( 'NONE', #49812, #60985, #73528, .T. ) ;
#52415 = DIRECTION ( 'NONE',  ( 0.000000000000000000, -0.000000000000000000, 1.000000000000000000 ) ) ;
#52416 = ORIENTED_EDGE ( 'NONE', *, *, #124157, .T. ) ;
#52417 = DIRECTION ( 'NONE',  ( 0.000000000000000000, 0.000000000000000000, 1.000000000000000000 ) ) ;
#52418 = FACE_OUTER_BOUND ( 'NONE', #56507, .T. ) ;
#52419 = DIRECTION ( 'NONE',  ( 0.000000000000000000, 0.000000000000000000, -1.000000000000000000 ) ) ;
#52420 = EDGE_CURVE ( 'NONE', #5314, #69112, #56791, .T. ) ;
#52421 = CARTESIAN_POINT ( 'NONE',  ( 187.1979166673494603, 6.668395609140176816, 3.850000000000000977 ) ) ;
#52422 = ORIENTED_EDGE ( 'NONE', *, *, #87419, .F. ) ;
#52423 = ORIENTED_EDGE ( 'NONE', *, *, #93776, .T. ) ;
#52424 = ORIENTED_EDGE ( 'NONE', *, *, #68329, .T. ) ;
#52425 = AXIS2_PLACEMENT_3D ( 'NONE', #3930, #21650, #52391 ) ;
#52426 = DIRECTION ( 'NONE',  ( 0.000000000000000000, -0.9999939076577903929, 0.003490651415223739937 ) ) ;
#52427 = AXIS2_PLACEMENT_3D ( 'NONE', #121307, #61760, #51933 ) ;
#52428 = AXIS2_PLACEMENT_3D ( 'NONE', #81528, #26477, #124020 ) ;
#52429 = EDGE_LOOP ( 'NONE', ( #126686, #84987 ) ) ;
#52430 = DIRECTION ( 'NONE',  ( 0.000000000000000000, 1.000000000000000000, 0.000000000000000000 ) ) ;
#52431 = CARTESIAN_POINT ( 'NONE',  ( -1.250000000000036193, 2.500000000000000000, 1.372243186433545370 ) ) ;
#52432 = AXIS2_PLACEMENT_3D ( 'NONE', #88492, #76752, #17815 ) ;
#52434 = ORIENTED_EDGE ( 'NONE', *, *, #47318, .F. ) ;
#52433 = CIRCLE ( 'NONE', #27376, 0.09999999999999982514 ) ;
#52435 = DIRECTION ( 'NONE',  ( 0.000000000000000000, 0.000000000000000000, 1.000000000000000000 ) ) ;
#52436 = CARTESIAN_POINT ( 'NONE',  ( 0.7999999999999612976, 2.500000000000000000, -1.084202172485504434E-16 ) ) ;
#52437 = DIRECTION ( 'NONE',  ( -0.000000000000000000, -1.000000000000000000, -0.000000000000000000 ) ) ;
#52438 = EDGE_CURVE ( 'NONE', #24620, #11460, #64934, .T. ) ;
#52439 = FACE_OUTER_BOUND ( 'NONE', #105227, .T. ) ;
#52440 = DIRECTION ( 'NONE',  ( 0.000000000000000000, 0.000000000000000000, 1.000000000000000000 ) ) ;
#52441 = ORIENTED_EDGE ( 'NONE', *, *, #27350, .T. ) ;
#52442 = VERTEX_POINT ( 'NONE', #36142 ) ;
#52443 = CARTESIAN_POINT ( 'NONE',  ( -1.050000000000038236, 12.50000000000000000, -1.753560074763288679 ) ) ;
#52444 = CARTESIAN_POINT ( 'NONE',  ( -7.900000000000011013, 2.500000000000000000, 5.022947341949748790 ) ) ;
#52445 = DIRECTION ( 'NONE',  ( 0.000000000000000000, 0.000000000000000000, 1.000000000000000000 ) ) ;
#52446 = DIRECTION ( 'NONE',  ( 0.000000000000000000, -0.9999939076577903929, 0.003490651415223739937 ) ) ;
#52447 = VERTEX_POINT ( 'NONE', #105527 ) ;
#52448 = CIRCLE ( 'NONE', #92163, 0.1000000000000002554 ) ;
#52449 = EDGE_CURVE ( 'NONE', #118122, #76584, #112776, .T. ) ;
#52450 = ORIENTED_EDGE ( 'NONE', *, *, #76730, .T. ) ;
#52451 = LINE ( 'NONE', #70174, #33365 ) ;
#52452 = DIRECTION ( 'NONE',  ( 0.000000000000000000, 0.000000000000000000, 1.000000000000000000 ) ) ;
#52453 = CARTESIAN_POINT ( 'NONE',  ( 13.54999999999989946, 2.500000000000000000, 2.611473670974873151 ) ) ;
#52454 = CARTESIAN_POINT ( 'NONE',  ( -8.150000000000012790, 12.50000000000000000, -2.576566944158915184 ) ) ;
#52455 = VERTEX_POINT ( 'NONE', #114060 ) ;
#52456 = CIRCLE ( 'NONE', #125608, 0.06509327318403745899 ) ;
#52457 = CARTESIAN_POINT ( 'NONE',  ( -12.89999999999999147, 2.500000000000000000, 3.637306695894644726 ) ) ;
#52458 = CIRCLE ( 'NONE', #90100, 0.06509327318403745899 ) ;
#52459 = CARTESIAN_POINT ( 'NONE',  ( -5.400000000000023448, 2.500000000000000000, -4.922947341949753586 ) ) ;
#52460 = ORIENTED_EDGE ( 'NONE', *, *, #65468, .T. ) ;
#52461 = DIRECTION ( 'NONE',  ( 0.000000000000000000, 0.000000000000000000, -1.000000000000000000 ) ) ;
#52462 = EDGE_CURVE ( 'NONE', #101658, #16388, #17071, .T. ) ;
#52463 = ORIENTED_EDGE ( 'NONE', *, *, #40588, .T. ) ;
#52464 = CIRCLE ( 'NONE', #37897, 0.09999999999999982514 ) ;
#52465 = FACE_OUTER_BOUND ( 'NONE', #70715, .T. ) ;
#52466 = AXIS2_PLACEMENT_3D ( 'NONE', #67499, #97631, #106169 ) ;
#52467 = ORIENTED_EDGE ( 'NONE', *, *, #98170, .T. ) ;
#52468 = CARTESIAN_POINT ( 'NONE',  ( 6.649999999999929301, 12.50000000000000000, -2.165063509461101710 ) ) ;
#52469 = DIRECTION ( 'NONE',  ( -0.000000000000000000, -1.000000000000000000, -0.000000000000000000 ) ) ;
#52470 = EDGE_LOOP ( 'NONE', ( #117757, #59300 ) ) ;
#52471 = ADVANCED_FACE ( 'NONE', ( #104858 ), #14923, .T. ) ;
#52472 = ORIENTED_EDGE ( 'NONE', *, *, #18127, .F. ) ;
#52473 = DIRECTION ( 'NONE',  ( -0.000000000000000000, -1.000000000000000000, -0.000000000000000000 ) ) ;
#52475 = CARTESIAN_POINT ( 'NONE',  ( 9.599999999999914380, 12.50000000000000000, -3.572213422710612374 ) ) ;
#52474 = CIRCLE ( 'NONE', #121516, 0.06509327318403745899 ) ;
#52476 = CARTESIAN_POINT ( 'NONE',  ( 185.5677083336747160, -4.367472073101514418, -7.564683531250002702 ) ) ;
#52477 = CIRCLE ( 'NONE', #71262, 0.06509327318403745899 ) ;
#52478 = LINE ( 'NONE', #41400, #103893 ) ;
#52479 = CARTESIAN_POINT ( 'NONE',  ( 4.149999999999938183, 12.50000000000000000, 5.737276932171707422 ) ) ;
#52480 = CARTESIAN_POINT ( 'NONE',  ( 12.89999999999990088, 2.500000000000000000, 4.330127018922196314 ) ) ;
#52481 = DIRECTION ( 'NONE',  ( 0.000000000000000000, 0.000000000000000000, 1.000000000000000000 ) ) ;
#52482 = DIRECTION ( 'NONE',  ( 0.000000000000000000, -0.000000000000000000, 1.000000000000000000 ) ) ;
#52483 = CIRCLE ( 'NONE', #6484, 0.06509327318403745899 ) ;
#52484 = ORIENTED_EDGE ( 'NONE', *, *, #24596, .T. ) ;
#52486 = ORIENTED_EDGE ( 'NONE', *, *, #120257, .F. ) ;
#52485 = ADVANCED_FACE ( 'NONE', ( #73471 ), #81849, .T. ) ;
#52487 = CARTESIAN_POINT ( 'NONE',  ( -8.749999999999971578, 12.50000000000000000, 6.495190528383297135 ) ) ;
#52488 = VERTEX_POINT ( 'NONE', #5379 ) ;
#52489 = CIRCLE ( 'NONE', #106775, 0.1000000000000000056 ) ;
#52490 = VECTOR ( 'NONE', #115644, 1000.000000000000000 ) ;
#52491 = DIRECTION ( 'NONE',  ( -0.000000000000000000, -1.000000000000000000, -0.000000000000000000 ) ) ;
#52492 = DIRECTION ( 'NONE',  ( 0.000000000000000000, 1.000000000000000000, 0.000000000000000000 ) ) ;
#52493 = CARTESIAN_POINT ( 'NONE',  ( -2.700000000000030376, 12.50000000000000000, 4.048810130592458201 ) ) ;
#52495 = ORIENTED_EDGE ( 'NONE', *, *, #68206, .T. ) ;
#52494 = EDGE_LOOP ( 'NONE', ( #92466, #39892, #72663, #38402 ) ) ;
#52496 = FACE_BOUND ( 'NONE', #119718, .T. ) ;
#52497 = EDGE_LOOP ( 'NONE', ( #73849, #76599 ) ) ;
#52498 = DIRECTION ( 'NONE',  ( 0.000000000000000000, -0.9999939076577903929, 0.003490651415223739937 ) ) ;
#52499 = CARTESIAN_POINT ( 'NONE',  ( 20.59313469514014017, -2.666874593322329456, 2.243770147468747034 ) ) ;
#52501 = ADVANCED_FACE ( 'NONE', ( #63677 ), #13905, .T. ) ;
#52500 = DIRECTION ( 'NONE',  ( -0.000000000000000000, -1.000000000000000000, -0.000000000000000000 ) ) ;
#52502 = DIRECTION ( 'NONE',  ( -4.274815082592931898E-19, -0.9999939076577903929, -0.003490651415223739937 ) ) ;
#52503 = CARTESIAN_POINT ( 'NONE',  ( 184.3645833340161175, -6.668395609140180369, 3.849999999999994760 ) ) ;
#52504 = CARTESIAN_POINT ( 'NONE',  ( -0.6000000000000383915, 2.500000000000000000, -4.676537180435977881 ) ) ;
#52505 = CARTESIAN_POINT ( 'NONE',  ( 0.8499999999999553468, 2.500000000000000000, 2.065063509461097624 ) ) ;
#52506 = DIRECTION ( 'NONE',  ( 0.000000000000000000, -0.9999939076577903929, 0.003490651415223739937 ) ) ;
#52507 = EDGE_CURVE ( 'NONE', #104306, #75844, #94373, .T. ) ;
#52508 = EDGE_CURVE ( 'NONE', #106389, #128383, #37950, .T. ) ;
#52509 = CARTESIAN_POINT ( 'NONE',  ( 10.64999999999990976, 12.50000000000000000, -6.841600689897077814 ) ) ;
#52510 = CARTESIAN_POINT ( 'NONE',  ( -3.350000000000028955, 2.500000000000000000, 7.188010851410848723 ) ) ;
#52511 = EDGE_CURVE ( 'NONE', #94677, #21207, #7301, .T. ) ;
#52512 = EDGE_CURVE ( 'NONE', #71164, #21407, #71378, .T. ) ;
#52513 = CARTESIAN_POINT ( 'NONE',  ( -8.350000000000013856, 12.50000000000000000, 2.099970236277060032 ) ) ;
#52514 = VERTEX_POINT ( 'NONE', #87797 ) ;
#52515 = VERTEX_POINT ( 'NONE', #115982 ) ;
#52516 = VERTEX_POINT ( 'NONE', #76706 ) ;
#52517 = CARTESIAN_POINT ( 'NONE',  ( 11.84999999999990727, 2.500000000000000000, 6.148780366869520009 ) ) ;
#52518 = ORIENTED_EDGE ( 'NONE', *, *, #122813, .T. ) ;
#52519 = PLANE ( 'NONE',  #24661 ) ;
#52520 = EDGE_CURVE ( 'NONE', #18680, #62169, #25405, .T. ) ;
#52521 = CIRCLE ( 'NONE', #79706, 0.1000000000000002554 ) ;
#52522 = CARTESIAN_POINT ( 'NONE',  ( -8.950000000000004619, 2.500000000000000000, 6.248780366869521430 ) ) ;
#52523 = CIRCLE ( 'NONE', #75493, 0.1000000000000002554 ) ;
#52524 = CIRCLE ( 'NONE', #62990, 0.1000000000000000472 ) ;
#52527 = ORIENTED_EDGE ( 'NONE', *, *, #83125, .F. ) ;
#52526 = ORIENTED_EDGE ( 'NONE', *, *, #64487, .F. ) ;
#52525 = EDGE_CURVE ( 'NONE', #105322, #21282, #58883, .T. ) ;
#52528 = EDGE_LOOP ( 'NONE', ( #20556, #96868, #72572, #80997 ) ) ;
#52529 = ADVANCED_FACE ( 'NONE', ( #107452 ), #96326, .T. ) ;
#52530 = DIRECTION ( 'NONE',  ( 0.000000000000000000, 1.000000000000000000, 0.000000000000000000 ) ) ;
#52531 = ADVANCED_FACE ( 'NONE', ( #9257 ), #49203, .T. ) ;
#52533 = EDGE_CURVE ( 'NONE', #67175, #40177, #109030, .T. ) ;
#52532 = AXIS2_PLACEMENT_3D ( 'NONE', #56295, #105413, #66758 ) ;
#52534 = CARTESIAN_POINT ( 'NONE',  ( 6.649999999999928413, 2.500000000000000000, 1.372243186433545370 ) ) ;
#52535 = AXIS2_PLACEMENT_3D ( 'NONE', #99224, #46900, #78304 ) ;
#52536 = CARTESIAN_POINT ( 'NONE',  ( 9.399999999999915090, 2.500000000000000000, -3.883716857408426648 ) ) ;
#52537 = CARTESIAN_POINT ( 'NONE',  ( 87.50000000000001421, -3.975350567648449740, -6.360562287258772152 ) ) ;
#52538 = FACE_OUTER_BOUND ( 'NONE', #86302, .T. ) ;
#52539 = AXIS2_PLACEMENT_3D ( 'NONE', #105004, #114826, #84080 ) ;
#52540 = DIRECTION ( 'NONE',  ( -0.000000000000000000, -1.000000000000000000, -0.000000000000000000 ) ) ;
#52541 = EDGE_LOOP ( 'NONE', ( #814, #25669, #55556, #105154 ) ) ;
#52542 = EDGE_CURVE ( 'NONE', #73050, #35098, #44387, .T. ) ;
#52543 = DIRECTION ( 'NONE',  ( -0.000000000000000000, 1.000000000000000000, -0.000000000000000000 ) ) ;
#52544 = ORIENTED_EDGE ( 'NONE', *, *, #68714, .F. ) ;
#52545 = ORIENTED_EDGE ( 'NONE', *, *, #46770, .T. ) ;
#52546 = ORIENTED_EDGE ( 'NONE', *, *, #94052, .T. ) ;
#52547 = DIRECTION ( 'NONE',  ( -4.274815082592931898E-19, -0.9999939076577903929, -0.003490651415223739937 ) ) ;
#52548 = ORIENTED_EDGE ( 'NONE', *, *, #76888, .F. ) ;
#52549 = ORIENTED_EDGE ( 'NONE', *, *, #23226, .T. ) ;
#52550 = ORIENTED_EDGE ( 'NONE', *, *, #121826, .T. ) ;
#52551 = DIRECTION ( 'NONE',  ( 0.000000000000000000, 0.000000000000000000, -1.000000000000000000 ) ) ;
#52552 = CARTESIAN_POINT ( 'NONE',  ( -12.69999999999999218, 2.500000000000000000, -4.776537180435974861 ) ) ;
#52553 = CARTESIAN_POINT ( 'NONE',  ( 0.3999999999999619971, 12.50000000000000000, -1.084202172485504434E-16 ) ) ;
#52554 = DIRECTION ( 'NONE',  ( 0.000000000000000000, -0.000000000000000000, 1.000000000000000000 ) ) ;
#52555 = DIRECTION ( 'NONE',  ( -4.274815082592931898E-19, -0.9999939076577903929, -0.003490651415223739937 ) ) ;
#52556 = CARTESIAN_POINT ( 'NONE',  ( -7.100000000000018296, 2.500000000000000000, -4.430127018922202176 ) ) ;
#52557 = CIRCLE ( 'NONE', #25352, 0.06509327318403745899 ) ;
#52558 = EDGE_LOOP ( 'NONE', ( #68671, #111488 ) ) ;
#52559 = CARTESIAN_POINT ( 'NONE',  ( -11.24999999999996270, 12.50000000000000000, 2.099970236277060032 ) ) ;
#52560 = ORIENTED_EDGE ( 'NONE', *, *, #2762, .F. ) ;
#52561 = CARTESIAN_POINT ( 'NONE',  ( 8.099999999999923261, 12.50000000000000000, -4.048810130592463530 ) ) ;
#52562 = ORIENTED_EDGE ( 'NONE', *, *, #99969, .F. ) ;
#52563 = LINE ( 'NONE', #40840, #61472 ) ;
#52564 = ORIENTED_EDGE ( 'NONE', *, *, #17653, .F. ) ;
#52565 = CIRCLE ( 'NONE', #121603, 0.06509327318403745899 ) ;
#52566 = CARTESIAN_POINT ( 'NONE',  ( 183.8593750003413732, 0.000000000000000000, 7.564683531250000925 ) ) ;
#52567 = AXIS2_PLACEMENT_3D ( 'NONE', #28095, #7800, #109215 ) ;
#52568 = EDGE_CURVE ( 'NONE', #33832, #125681, #25503, .T. ) ;
#52569 = CARTESIAN_POINT ( 'NONE',  ( 0.7999999999999553024, 12.50000000000000000, -4.265033745738164406 ) ) ;
#52570 = ADVANCED_FACE ( 'NONE', ( #98268 ), #102861, .T. ) ;
#52571 = ORIENTED_EDGE ( 'NONE', *, *, #57561, .T. ) ;
#52572 = ORIENTED_EDGE ( 'NONE', *, *, #123992, .F. ) ;
#52573 = DIRECTION ( 'NONE',  ( -0.000000000000000000, -1.000000000000000000, -0.000000000000000000 ) ) ;
#52574 = DIRECTION ( 'NONE',  ( 0.000000000000000000, -0.000000000000000000, 1.000000000000000000 ) ) ;
#52575 = FACE_OUTER_BOUND ( 'NONE', #53595, .T. ) ;
#52576 = CARTESIAN_POINT ( 'NONE',  ( -10.20000000000000462, 2.500000000000000000, 4.676537180435972552 ) ) ;
#52577 = CIRCLE ( 'NONE', #73403, 0.06509327318403741736 ) ;
#52578 = EDGE_CURVE ( 'NONE', #71646, #92201, #96598, .T. ) ;
#52579 = CIRCLE ( 'NONE', #46224, 0.06509327318403745899 ) ;
#52580 = DIRECTION ( 'NONE',  ( 0.000000000000000000, 0.000000000000000000, 1.000000000000000000 ) ) ;
#52581 = ORIENTED_EDGE ( 'NONE', *, *, #63871, .T. ) ;
#52582 = DIRECTION ( 'NONE',  ( -0.000000000000000000, -1.000000000000000000, -0.000000000000000000 ) ) ;
#52583 = AXIS2_PLACEMENT_3D ( 'NONE', #71759, #92681, #42973 ) ;
#52584 = AXIS2_PLACEMENT_3D ( 'NONE', #67083, #118794, #27829 ) ;
#52585 = ORIENTED_EDGE ( 'NONE', *, *, #2567, .F. ) ;
#52586 = CARTESIAN_POINT ( 'NONE',  ( -4.550000000000022915, 12.50000000000000000, 6.495190528383297135 ) ) ;
#52587 = DIRECTION ( 'NONE',  ( -0.000000000000000000, 1.000000000000000000, -0.000000000000000000 ) ) ;
#52588 = AXIS2_PLACEMENT_3D ( 'NONE', #29628, #28352, #69544 ) ;
#52589 = AXIS2_PLACEMENT_3D ( 'NONE', #43562, #93289, #34391 ) ;
#52590 = CARTESIAN_POINT ( 'NONE',  ( 187.2916666666666572, 4.445597072760120838, -7.699999999999998401 ) ) ;
#52591 = CARTESIAN_POINT ( 'NONE',  ( -3.950000000000024603, 2.500000000000000000, -2.411473670974877859 ) ) ;
#52592 = DIRECTION ( 'NONE',  ( 0.000000000000000000, 0.000000000000000000, 1.000000000000000000 ) ) ;
#52593 = CARTESIAN_POINT ( 'NONE',  ( -5.200000000000022382, 12.50000000000000000, 0.3464101615137735735 ) ) ;
#52594 = CARTESIAN_POINT ( 'NONE',  ( 6.249999999999932498, 12.50000000000000000, 5.802370205355744659 ) ) ;
#52595 = EDGE_LOOP ( 'NONE', ( #70906, #12002 ) ) ;
#52596 = DIRECTION ( 'NONE',  ( 0.000000000000000000, 0.000000000000000000, 1.000000000000000000 ) ) ;
#52597 = CARTESIAN_POINT ( 'NONE',  ( -10.84999999999999964, 2.500000000000000000, 2.757883832488649656 ) ) ;
#52598 = FACE_OUTER_BOUND ( 'NONE', #55388, .T. ) ;
#52599 = ORIENTED_EDGE ( 'NONE', *, *, #46519, .F. ) ;
#52600 = ORIENTED_EDGE ( 'NONE', *, *, #117211, .F. ) ;
#52601 = CARTESIAN_POINT ( 'NONE',  ( 5.649999999999932854, 2.500000000000000000, 1.818653347947321475 ) ) ;
#52602 = EDGE_CURVE ( 'NONE', #79758, #67593, #40198, .T. ) ;
#52603 = EDGE_LOOP ( 'NONE', ( #41770, #103411 ) ) ;
#52604 = VERTEX_POINT ( 'NONE', #89106 ) ;
#52605 = DIRECTION ( 'NONE',  ( 0.000000000000000000, 0.000000000000000000, -1.000000000000000000 ) ) ;
#52606 = AXIS2_PLACEMENT_3D ( 'NONE', #121464, #112951, #81560 ) ;
#52607 = VECTOR ( 'NONE', #91841, 1000.000000000000000 ) ;
#52608 = EDGE_LOOP ( 'NONE', ( #91711, #116262, #78454, #48824 ) ) ;
#52609 = CARTESIAN_POINT ( 'NONE',  ( 20.25366426268886499, -2.573118374677165754, -4.179292740214979318 ) ) ;
#52610 = DIRECTION ( 'NONE',  ( -0.000000000000000000, -1.000000000000000000, -0.000000000000000000 ) ) ;
#52611 = CARTESIAN_POINT ( 'NONE',  ( 17.34645602450315138, 0.4686430837609508737, 5.377443133677435760 ) ) ;
#52612 = EDGE_LOOP ( 'NONE', ( #64473, #86739 ) ) ;
#52614 = DIRECTION ( 'NONE',  ( 0.000000000000000000, 0.000000000000000000, 1.000000000000000000 ) ) ;
#52613 = AXIS2_PLACEMENT_3D ( 'NONE', #106538, #114422, #46993 ) ;
#52615 = AXIS2_PLACEMENT_3D ( 'NONE', #32439, #71688, #52061 ) ;
#52616 = DIRECTION ( 'NONE',  ( 0.000000000000000000, 1.000000000000000000, 0.000000000000000000 ) ) ;
#52618 = ADVANCED_FACE ( 'NONE', ( #27583 ), #107069, .T. ) ;
#52617 = VECTOR ( 'NONE', #20007, 1000.000000000000000 ) ;
#52619 = EDGE_CURVE ( 'NONE', #20692, #61976, #46439, .T. ) ;
#52620 = EDGE_LOOP ( 'NONE', ( #78914, #116623, #23435, #112965 ) ) ;
#52621 = AXIS2_PLACEMENT_3D ( 'NONE', #88715, #69068, #99189 ) ;
#52622 = EDGE_LOOP ( 'NONE', ( #100416, #84944 ) ) ;
#52623 = EDGE_LOOP ( 'NONE', ( #2311, #19938 ) ) ;
#52624 = FACE_OUTER_BOUND ( 'NONE', #45472, .T. ) ;
#52625 = CARTESIAN_POINT ( 'NONE',  ( 6.649999999999929301, 2.500000000000000000, 6.595190528383296780 ) ) ;
#52626 = CARTESIAN_POINT ( 'NONE',  ( -8.350000000000013856, 2.500000000000000000, -5.802370205355744659 ) ) ;
#52627 = EDGE_CURVE ( 'NONE', #76, #16047, #59002, .T. ) ;
#52628 = FACE_BOUND ( 'NONE', #123614, .T. ) ;
#52629 = ORIENTED_EDGE ( 'NONE', *, *, #78108, .F. ) ;
#52630 = FACE_OUTER_BOUND ( 'NONE', #112537, .T. ) ;
#52631 = DIRECTION ( 'NONE',  ( 0.000000000000000000, 0.000000000000000000, -1.000000000000000000 ) ) ;
#52632 = VERTEX_POINT ( 'NONE', #26966 ) ;
#52633 = CARTESIAN_POINT ( 'NONE',  ( 87.50000000000000000, 2.780337595463734419E-15, -7.500000000000000000 ) ) ;
#52634 = DIRECTION ( 'NONE',  ( -0.000000000000000000, 1.000000000000000000, -0.000000000000000000 ) ) ;
#52635 = CARTESIAN_POINT ( 'NONE',  ( -11.24999999999999822, 12.50000000000000000, 5.737276932171707422 ) ) ;
#52636 = DIRECTION ( 'NONE',  ( 0.000000000000000000, 1.000000000000000000, 0.000000000000000000 ) ) ;
#52637 = FACE_OUTER_BOUND ( 'NONE', #50829, .T. ) ;
#52638 = LINE ( 'NONE', #90636, #86918 ) ;
#52639 = FACE_OUTER_BOUND ( 'NONE', #28856, .T. ) ;
#52640 = VECTOR ( 'NONE', #81565, 1000.000000000000000 ) ;
#52641 = AXIS2_PLACEMENT_3D ( 'NONE', #12625, #22486, #114065 ) ;
#52642 = ORIENTED_EDGE ( 'NONE', *, *, #84726, .T. ) ;
#52643 = VERTEX_POINT ( 'NONE', #87157 ) ;
#52644 = ORIENTED_EDGE ( 'NONE', *, *, #37721, .T. ) ;
#52645 = VERTEX_POINT ( 'NONE', #96987 ) ;
#52646 = CARTESIAN_POINT ( 'NONE',  ( -7.100000000000017408, 12.50000000000000000, -5.022947341949754119 ) ) ;
#52647 = DIRECTION ( 'NONE',  ( 0.000000000000000000, 0.000000000000000000, -1.000000000000000000 ) ) ;
#52648 = CARTESIAN_POINT ( 'NONE',  ( -2.900000000000030109, 12.50000000000000000, 0.6277270498435120194 ) ) ;
#52649 = ORIENTED_EDGE ( 'NONE', *, *, #126642, .F. ) ;
#52650 = FACE_BOUND ( 'NONE', #58658, .T. ) ;
#52651 = AXIS2_PLACEMENT_3D ( 'NONE', #40401, #20102, #119572 ) ;
#52652 = DIRECTION ( 'NONE',  ( 0.000000000000000000, 0.000000000000000000, -1.000000000000000000 ) ) ;
#52653 = DIRECTION ( 'NONE',  ( 0.000000000000000000, 1.000000000000000000, 0.000000000000000000 ) ) ;
#52654 = AXIS2_PLACEMENT_3D ( 'NONE', #124674, #24534, #65734 ) ;
#52657 = EDGE_CURVE ( 'NONE', #108562, #49122, #127108, .T. ) ;
#52656 = FACE_OUTER_BOUND ( 'NONE', #36998, .T. ) ;
#52655 = AXIS2_PLACEMENT_3D ( 'NONE', #108747, #40692, #19065 ) ;
#52658 = VECTOR ( 'NONE', #23940, 1000.000000000000000 ) ;
#52659 = AXIS2_PLACEMENT_3D ( 'NONE', #99695, #110781, #40790 ) ;
#52660 = CARTESIAN_POINT ( 'NONE',  ( 1.849999999999951017, 2.500000000000000000, -6.148780366869526226 ) ) ;
#52661 = DIRECTION ( 'NONE',  ( -4.274815082592931898E-19, -0.9999939076577903929, -0.003490651415223739937 ) ) ;
#52662 = LINE ( 'NONE', #112237, #95611 ) ;
#52663 = FACE_OUTER_BOUND ( 'NONE', #29407, .T. ) ;
#52664 = DIRECTION ( 'NONE',  ( 0.000000000000000000, 0.000000000000000000, -1.000000000000000000 ) ) ;
#52665 = EDGE_CURVE ( 'NONE', #87872, #95698, #71476, .T. ) ;
#52666 = FACE_OUTER_BOUND ( 'NONE', #91501, .T. ) ;
#52667 = ADVANCED_FACE ( 'NONE', ( #119848 ), #12973, .T. ) ;
#52668 = AXIS2_PLACEMENT_3D ( 'NONE', #99150, #79510, #38297 ) ;
#52669 = ORIENTED_EDGE ( 'NONE', *, *, #89947, .F. ) ;
#52670 = CONICAL_SURFACE ( 'NONE', #31754, 0.1000000000000002554, 0.003490658503988666988 ) ;
#52671 = EDGE_LOOP ( 'NONE', ( #35375, #113261 ) ) ;
#52672 = EDGE_LOOP ( 'NONE', ( #48197, #66264 ) ) ;
#52673 = ORIENTED_EDGE ( 'NONE', *, *, #120807, .F. ) ;
#52674 = EDGE_LOOP ( 'NONE', ( #111330, #41690, #27031, #55636 ) ) ;
#52675 = AXIS2_PLACEMENT_3D ( 'NONE', #45962, #33564, #85855 ) ;
#52676 = AXIS2_PLACEMENT_3D ( 'NONE', #113033, #114324, #24664 ) ;
#52677 = EDGE_CURVE ( 'NONE', #60915, #101221, #17160, .T. ) ;
#52678 = ORIENTED_EDGE ( 'NONE', *, *, #30215, .T. ) ;
#52680 = EDGE_CURVE ( 'NONE', #16531, #16470, #89745, .T. ) ;
#52679 = FACE_OUTER_BOUND ( 'NONE', #22313, .T. ) ;
#52682 = ORIENTED_EDGE ( 'NONE', *, *, #16829, .T. ) ;
#52681 = EDGE_CURVE ( 'NONE', #122810, #122820, #6695, .T. ) ;
#52683 = EDGE_LOOP ( 'NONE', ( #15758, #124925, #77512, #35018 ) ) ;
#52684 = AXIS2_PLACEMENT_3D ( 'NONE', #111216, #9176, #51052 ) ;
#52685 = ADVANCED_FACE ( 'NONE', ( #100214 ), #79297, .T. ) ;
#52686 = CONICAL_SURFACE ( 'NONE', #83970, 0.09999999999999999167, 0.003490658503988666988 ) ;
#52687 = FACE_OUTER_BOUND ( 'NONE', #65070, .T. ) ;
#52688 = PLANE ( 'NONE',  #14395 ) ;
#52689 = LINE ( 'NONE', #69749, #25942 ) ;
#52690 = ORIENTED_EDGE ( 'NONE', *, *, #101931, .T. ) ;
#52691 = CARTESIAN_POINT ( 'NONE',  ( 6.049999999999932321, 2.500000000000000000, 1.818653347947321475 ) ) ;
#52692 = EDGE_CURVE ( 'NONE', #60192, #118069, #40013, .T. ) ;
#52693 = VERTEX_POINT ( 'NONE', #713 ) ;
#52694 = ORIENTED_EDGE ( 'NONE', *, *, #77434, .F. ) ;
#52695 = DIRECTION ( 'NONE',  ( 0.000000000000000000, 0.000000000000000000, 1.000000000000000000 ) ) ;
#52696 = LINE ( 'NONE', #90690, #25231 ) ;
#52697 = VERTEX_POINT ( 'NONE', #51131 ) ;
#52698 = EDGE_LOOP ( 'NONE', ( #34518, #100875, #61889, #46536 ) ) ;
#52699 = CARTESIAN_POINT ( 'NONE',  ( -8.350000000000012079, 12.50000000000000000, 2.857883832488649301 ) ) ;
#52700 = FACE_OUTER_BOUND ( 'NONE', #123427, .T. ) ;
#52701 = CARTESIAN_POINT ( 'NONE',  ( 1.249999999999988454, 2.500000000000000000, -2.165063509461101710 ) ) ;
#52703 = DIRECTION ( 'NONE',  ( 0.000000000000000000, -0.9999939076577903929, 0.003490651415223739937 ) ) ;
#52702 = AXIS2_PLACEMENT_3D ( 'NONE', #72445, #35111, #64545 ) ;
#52704 = CONICAL_SURFACE ( 'NONE', #63168, 0.09999999999999999167, 0.003490658503988666988 ) ;
#52705 = AXIS2_PLACEMENT_3D ( 'NONE', #72693, #75256, #53689 ) ;
#52706 = DIRECTION ( 'NONE',  ( 0.000000000000000000, 1.000000000000000000, 0.000000000000000000 ) ) ;
#52707 = ORIENTED_EDGE ( 'NONE', *, *, #78463, .F. ) ;
#52708 = DIRECTION ( 'NONE',  ( 0.000000000000000000, 0.000000000000000000, -1.000000000000000000 ) ) ;
#52709 = CONICAL_SURFACE ( 'NONE', #59070, 0.09999999999999982514, 0.003490658503988666988 ) ;
#52711 = ORIENTED_EDGE ( 'NONE', *, *, #123234, .F. ) ;
#52710 = CIRCLE ( 'NONE', #123792, 0.09999999999999982514 ) ;
#52712 = CARTESIAN_POINT ( 'NONE',  ( -5.000000000000022204, 2.500000000000000000, -0.6928203230275541413 ) ) ;
#52713 = VECTOR ( 'NONE', #690, 1000.000000000000000 ) ;
#52714 = CARTESIAN_POINT ( 'NONE',  ( -13.09999999999999254, 2.500000000000000000, 0.2464101615137777868 ) ) ;
#52715 = DIRECTION ( 'NONE',  ( 0.000000000000000000, 0.000000000000000000, -1.000000000000000000 ) ) ;
#52716 = AXIS2_PLACEMENT_3D ( 'NONE', #17901, #76838, #87282 ) ;
#52717 = AXIS2_PLACEMENT_3D ( 'NONE', #63719, #22524, #82730 ) ;
#52718 = DIRECTION ( 'NONE',  ( 0.000000000000000000, -0.9999939076577903929, 0.003490651415223739937 ) ) ;
#52719 = DIRECTION ( 'NONE',  ( -0.000000000000000000, 1.000000000000000000, -0.000000000000000000 ) ) ;
#52720 = VERTEX_POINT ( 'NONE', #101507 ) ;
#52721 = VECTOR ( 'NONE', #99431, 1000.000000000000000 ) ;
#52722 = CARTESIAN_POINT ( 'NONE',  ( 0.6499999999999566125, 2.500000000000000000, -6.741600689897077281 ) ) ;
#52723 = EDGE_CURVE ( 'NONE', #33429, #66127, #65206, .T. ) ;
#52724 = DIRECTION ( 'NONE',  ( -0.000000000000000000, 1.000000000000000000, -0.000000000000000000 ) ) ;
#52725 = ORIENTED_EDGE ( 'NONE', *, *, #22251, .F. ) ;
#52726 = ORIENTED_EDGE ( 'NONE', *, *, #114875, .T. ) ;
#52727 = VERTEX_POINT ( 'NONE', #119209 ) ;
#52728 = DIRECTION ( 'NONE',  ( 0.000000000000000000, 1.000000000000000000, 0.000000000000000000 ) ) ;
#52729 = DIRECTION ( 'NONE',  ( 0.000000000000000000, 1.000000000000000000, 0.000000000000000000 ) ) ;
#52730 = CARTESIAN_POINT ( 'NONE',  ( 186.1093750003413732, 9.264065473108010111E-16, -7.564683531250000925 ) ) ;
#52731 = LINE ( 'NONE', #92660, #128586 ) ;
#52732 = CARTESIAN_POINT ( 'NONE',  ( 4.799999999999937650, 2.500000000000000000, -0.3464101615137782364 ) ) ;
#52733 = EDGE_CURVE ( 'NONE', #113918, #109879, #94555, .T. ) ;
#52734 = DIRECTION ( 'NONE',  ( 0.000000000000000000, 0.000000000000000000, 1.000000000000000000 ) ) ;
#52735 = LINE ( 'NONE', #92667, #115277 ) ;
#52736 = CIRCLE ( 'NONE', #15154, 0.06509327318403745899 ) ;
#52737 = LINE ( 'NONE', #33745, #127964 ) ;
#52738 = VERTEX_POINT ( 'NONE', #40676 ) ;
#52739 = CARTESIAN_POINT ( 'NONE',  ( -9.400000000000009237, 2.500000000000000000, -4.676537180435974328 ) ) ;
#52740 = CARTESIAN_POINT ( 'NONE',  ( 4.349999999999940137, 2.500000000000000000, -6.941600689897078347 ) ) ;
#52741 = DIRECTION ( 'NONE',  ( 0.000000000000000000, 1.000000000000000000, 0.000000000000000000 ) ) ;
#52742 = DIRECTION ( 'NONE',  ( 0.000000000000000000, 0.000000000000000000, 1.000000000000000000 ) ) ;
#52743 = AXIS2_PLACEMENT_3D ( 'NONE', #95923, #94624, #84808 ) ;
#52744 = AXIS2_PLACEMENT_3D ( 'NONE', #40823, #32302, #110816 ) ;
#52745 = ORIENTED_EDGE ( 'NONE', *, *, #71553, .F. ) ;
#52746 = CARTESIAN_POINT ( 'NONE',  ( -11.25000000000000000, 12.50000000000000000, 7.122917578226811486 ) ) ;
#52747 = VECTOR ( 'NONE', #116807, 1000.000000000000000 ) ;
#52748 = CARTESIAN_POINT ( 'NONE',  ( -14.79999999999998472, 2.500000000000000000, 0.4464101615137758272 ) ) ;
#52750 = ORIENTED_EDGE ( 'NONE', *, *, #38682, .T. ) ;
#52749 = CARTESIAN_POINT ( 'NONE',  ( -2.500000000000030642, 2.500000000000000000, -0.5928203230275541635 ) ) ;
#52751 = AXIS2_PLACEMENT_3D ( 'NONE', #30425, #34111, #84498 ) ;
#52752 = ORIENTED_EDGE ( 'NONE', *, *, #27569, .T. ) ;
#52754 = AXIS2_PLACEMENT_3D ( 'NONE', #91755, #3374, #14462 ) ;
#52753 = DIRECTION ( 'NONE',  ( 0.000000000000000000, 1.000000000000000000, 0.000000000000000000 ) ) ;
#52755 = ADVANCED_FACE ( 'NONE', ( #99582 ), #115368, .T. ) ;
#52756 = ORIENTED_EDGE ( 'NONE', *, *, #76923, .T. ) ;
#52757 = AXIS2_PLACEMENT_3D ( 'NONE', #27412, #55603, #115807 ) ;
#52759 = ORIENTED_EDGE ( 'NONE', *, *, #1074, .T. ) ;
#52758 = AXIS2_PLACEMENT_3D ( 'NONE', #41299, #92307, #121131 ) ;
#52760 = AXIS2_PLACEMENT_3D ( 'NONE', #113365, #42060, #103563 ) ;
#52761 = DIRECTION ( 'NONE',  ( 0.000000000000000000, -0.9999939076577903929, 0.003490651415223739937 ) ) ;
#52762 = VECTOR ( 'NONE', #102697, 1000.000000000000000 ) ;
#52763 = LINE ( 'NONE', #54674, #30046 ) ;
#52764 = LINE ( 'NONE', #120862, #92274 ) ;
#52765 = CARTESIAN_POINT ( 'NONE',  ( -8.950000000000008171, 2.500000000000000000, -2.611473670974877592 ) ) ;
#52766 = EDGE_CURVE ( 'NONE', #39661, #78151, #88182, .T. ) ;
#52767 = VERTEX_POINT ( 'NONE', #81224 ) ;
#52768 = CIRCLE ( 'NONE', #50718, 0.06509327318403743123 ) ;
#52769 = DIRECTION ( 'NONE',  ( -0.000000000000000000, 1.000000000000000000, -0.000000000000000000 ) ) ;
#52771 = ORIENTED_EDGE ( 'NONE', *, *, #86537, .T. ) ;
#52770 = LINE ( 'NONE', #60202, #95888 ) ;
#52772 = EDGE_CURVE ( 'NONE', #121359, #69185, #102150, .T. ) ;
#52773 = DIRECTION ( 'NONE',  ( -0.000000000000000000, 1.000000000000000000, -0.000000000000000000 ) ) ;
#52774 = CARTESIAN_POINT ( 'NONE',  ( 17.49862860983209600, -2.500000000000000000, 4.081131818001135336 ) ) ;
#52775 = EDGE_CURVE ( 'NONE', #96170, #109430, #100807, .T. ) ;
#52776 = ORIENTED_EDGE ( 'NONE', *, *, #10641, .F. ) ;
#52777 = ORIENTED_EDGE ( 'NONE', *, *, #98044, .T. ) ;
#52778 = EDGE_CURVE ( 'NONE', #12245, #125864, #79896, .T. ) ;
#52779 = ORIENTED_EDGE ( 'NONE', *, *, #125847, .T. ) ;
#52780 = VERTEX_POINT ( 'NONE', #21656 ) ;
#52781 = DIRECTION ( 'NONE',  ( 0.000000000000000000, -0.000000000000000000, 1.000000000000000000 ) ) ;
#52782 = CARTESIAN_POINT ( 'NONE',  ( 14.93723468939127841, 2.500000000000000000, 6.174425106950392816 ) ) ;
#52783 = DIRECTION ( 'NONE',  ( 0.000000000000000000, 0.000000000000000000, -1.000000000000000000 ) ) ;
#52784 = AXIS2_PLACEMENT_3D ( 'NONE', #79323, #128430, #9275 ) ;
#52785 = EDGE_CURVE ( 'NONE', #86677, #46102, #111262, .T. ) ;
#52786 = FACE_BOUND ( 'NONE', #102993, .T. ) ;
#52787 = ORIENTED_EDGE ( 'NONE', *, *, #75858, .T. ) ;
#52788 = CARTESIAN_POINT ( 'NONE',  ( 184.3229166673494603, -4.445597072760122614, 7.699999999999998401 ) ) ;
#52789 = CARTESIAN_POINT ( 'NONE',  ( 7.299999999999924327, 2.500000000000000000, 0.3464101615137735735 ) ) ;
#52790 = CARTESIAN_POINT ( 'NONE',  ( -9.400000000000007461, 12.50000000000000000, 3.983716857408420076 ) ) ;
#52791 = VECTOR ( 'NONE', #102397, 1000.000000000000000 ) ;
#52792 = CIRCLE ( 'NONE', #105104, 0.06509327318403745899 ) ;
#52794 = AXIS2_PLACEMENT_3D ( 'NONE', #3625, #121452, #92007 ) ;
#52793 = CARTESIAN_POINT ( 'NONE',  ( -1.250000000000037970, 2.500000000000000000, 7.188010851410848723 ) ) ;
#52795 = DIRECTION ( 'NONE',  ( 0.000000000000000000, 0.000000000000000000, -1.000000000000000000 ) ) ;
#52796 = DIRECTION ( 'NONE',  ( 0.000000000000000000, -0.000000000000000000, 1.000000000000000000 ) ) ;
#52797 = CIRCLE ( 'NONE', #117523, 0.1000000000000000056 ) ;
#52799 = DIRECTION ( 'NONE',  ( 0.000000000000000000, 0.000000000000000000, 1.000000000000000000 ) ) ;
#52798 = CONICAL_SURFACE ( 'NONE', #121752, 0.09999999999999982514, 0.003490658503988666988 ) ;
#52800 = CIRCLE ( 'NONE', #42454, 0.1000000000000002554 ) ;
#52801 = EDGE_LOOP ( 'NONE', ( #74048, #96560, #3269, #82906 ) ) ;
#52802 = EDGE_LOOP ( 'NONE', ( #32722, #82457 ) ) ;
#52803 = ORIENTED_EDGE ( 'NONE', *, *, #53272, .T. ) ;
#52804 = ORIENTED_EDGE ( 'NONE', *, *, #102954, .F. ) ;
#52806 = VERTEX_POINT ( 'NONE', #91680 ) ;
#52805 = AXIS2_PLACEMENT_3D ( 'NONE', #75855, #93109, #13878 ) ;
#52807 = DIRECTION ( 'NONE',  ( 0.000000000000000000, 0.000000000000000000, -1.000000000000000000 ) ) ;
#52808 = AXIS2_PLACEMENT_3D ( 'NONE', #5832, #45148, #106623 ) ;
#52809 = DIRECTION ( 'NONE',  ( 0.000000000000000000, -0.9999939076577903929, 0.003490651415223739937 ) ) ;
#52810 = VERTEX_POINT ( 'NONE', #111976 ) ;
#52811 = FACE_BOUND ( 'NONE', #77148, .T. ) ;
#52812 = AXIS2_PLACEMENT_3D ( 'NONE', #58692, #78346, #38426 ) ;
#52813 = DIRECTION ( 'NONE',  ( 0.000000000000000000, 1.000000000000000000, 0.000000000000000000 ) ) ;
#52814 = ADVANCED_FACE ( 'NONE', ( #50458 ), #86129, .T. ) ;
#52815 = EDGE_LOOP ( 'NONE', ( #94754, #57225 ) ) ;
#52816 = DIRECTION ( 'NONE',  ( -0.000000000000000000, 1.000000000000000000, -0.000000000000000000 ) ) ;
#52817 = DIRECTION ( 'NONE',  ( -0.000000000000000000, 1.000000000000000000, -0.000000000000000000 ) ) ;
#52818 = DIRECTION ( 'NONE',  ( 0.000000000000000000, 1.000000000000000000, 0.000000000000000000 ) ) ;
#52819 = EDGE_LOOP ( 'NONE', ( #30348, #54399, #112334, #48025 ) ) ;
#52820 = CARTESIAN_POINT ( 'NONE',  ( -0.8500000000000382805, 12.50000000000000000, -5.802370205355749988 ) ) ;
#52821 = ADVANCED_FACE ( 'NONE', ( #62236 ), #2510, .T. ) ;
#52822 = CONICAL_SURFACE ( 'NONE', #86257, 0.1000000000000000472, 0.003490658503988666988 ) ;
#52823 = ORIENTED_EDGE ( 'NONE', *, *, #14959, .T. ) ;
#52824 = VERTEX_POINT ( 'NONE', #123690 ) ;
#52825 = ORIENTED_EDGE ( 'NONE', *, *, #109163, .F. ) ;
#52826 = ADVANCED_FACE ( 'NONE', ( #4548 ), #92406, .T. ) ;
#52827 = CARTESIAN_POINT ( 'NONE',  ( -3.749999999999994671, 12.50000000000000000, -6.560283801567339701 ) ) ;
#52828 = FACE_OUTER_BOUND ( 'NONE', #9660, .T. ) ;
#52829 = CARTESIAN_POINT ( 'NONE',  ( -7.100000000000018296, 2.500000000000000000, -4.230127018922201998 ) ) ;
#52831 = ORIENTED_EDGE ( 'NONE', *, *, #65352, .T. ) ;
#52830 = ADVANCED_FACE ( 'NONE', ( #32787 ), #77833, .T. ) ;
#52832 = CARTESIAN_POINT ( 'NONE',  ( -13.54999999999999005, 2.500000000000000000, 2.511473670974877503 ) ) ;
#52833 = EDGE_CURVE ( 'NONE', #72795, #30951, #21399, .T. ) ;
#52834 = CIRCLE ( 'NONE', #71705, 0.1000000000000002554 ) ;
#52835 = AXIS2_PLACEMENT_3D ( 'NONE', #16071, #105106, #95944 ) ;
#52837 = DIRECTION ( 'NONE',  ( 0.6795087154616719083, 3.181775308912716821E-15, 0.7336674352945131705 ) ) ;
#52836 = CIRCLE ( 'NONE', #71611, 0.09999999999999982514 ) ;
#52839 = EDGE_CURVE ( 'NONE', #2439, #53221, #90341, .T. ) ;
#52838 = CARTESIAN_POINT ( 'NONE',  ( -4.350000000000023626, 2.500000000000000000, -1.818653347947325916 ) ) ;
#52840 = CARTESIAN_POINT ( 'NONE',  ( 186.4062500006828031, -8.891194145520236347, -1.633285867636356693E-15 ) ) ;
#52841 = EDGE_LOOP ( 'NONE', ( #16376, #23335, #86768, #116227 ) ) ;
#52842 = DIRECTION ( 'NONE',  ( 0.000000000000000000, 0.000000000000000000, 1.000000000000000000 ) ) ;
#52843 = CONICAL_SURFACE ( 'NONE', #100950, 0.09999999999999982514, 0.003490658503988666988 ) ;
#52844 = VERTEX_POINT ( 'NONE', #73973 ) ;
#52845 = FACE_OUTER_BOUND ( 'NONE', #367, .T. ) ;
#52846 = EDGE_CURVE ( 'NONE', #126729, #114539, #33927, .T. ) ;
#52847 = VECTOR ( 'NONE', #86473, 1000.000000000000000 ) ;
#52848 = EDGE_CURVE ( 'NONE', #112012, #37787, #98759, .T. ) ;
#52849 = VERTEX_POINT ( 'NONE', #65431 ) ;
#52850 = CIRCLE ( 'NONE', #38282, 0.09999999999999982514 ) ;
#52851 = ORIENTED_EDGE ( 'NONE', *, *, #13191, .F. ) ;
#52852 = PLANE ( 'NONE',  #15749 ) ;
#52853 = DIRECTION ( 'NONE',  ( 0.000000000000000000, -0.000000000000000000, 1.000000000000000000 ) ) ;
#52854 = CARTESIAN_POINT ( 'NONE',  ( -1.850000000000033396, 12.50000000000000000, -6.841600689897077814 ) ) ;
#52855 = FACE_OUTER_BOUND ( 'NONE', #15679, .T. ) ;
#52856 = CARTESIAN_POINT ( 'NONE',  ( 184.4999999999999716, -6.306458657965935188, -4.321730308584150748 ) ) ;
#52857 = AXIS2_PLACEMENT_3D ( 'NONE', #112526, #62141, #24141 ) ;
#52858 = ORIENTED_EDGE ( 'NONE', *, *, #65829, .T. ) ;
#52859 = ORIENTED_EDGE ( 'NONE', *, *, #50474, .T. ) ;
#52860 = VECTOR ( 'NONE', #127660, 1000.000000000000000 ) ;
#52861 = CARTESIAN_POINT ( 'NONE',  ( 0.5999999999999547917, 12.50000000000000000, 3.983716857408420076 ) ) ;
#52863 = AXIS2_PLACEMENT_3D ( 'NONE', #79753, #98735, #9077 ) ;
#52862 = DIRECTION ( 'NONE',  ( 0.000000000000000000, -0.000000000000000000, 1.000000000000000000 ) ) ;
#52864 = AXIS2_PLACEMENT_3D ( 'NONE', #71714, #22635, #111647 ) ;
#52865 = VECTOR ( 'NONE', #120458, 1000.000000000000000 ) ;
#52866 = DIRECTION ( 'NONE',  ( -0.000000000000000000, 1.000000000000000000, -0.000000000000000000 ) ) ;
#52867 = EDGE_LOOP ( 'NONE', ( #6020, #39383, #120685, #47913 ) ) ;
#52868 = ORIENTED_EDGE ( 'NONE', *, *, #77508, .T. ) ;
#52869 = DIRECTION ( 'NONE',  ( 0.000000000000000000, 1.000000000000000000, 0.000000000000000000 ) ) ;
#52870 = CIRCLE ( 'NONE', #128180, 0.09999999999999982514 ) ;
#52871 = ORIENTED_EDGE ( 'NONE', *, *, #61301, .F. ) ;
#52872 = CARTESIAN_POINT ( 'NONE',  ( 7.899999999999924860, 2.500000000000000000, 5.122947341949749323 ) ) ;
#52873 = CARTESIAN_POINT ( 'NONE',  ( 0.6499999999999561684, 12.50000000000000000, -1.818653347947325916 ) ) ;
#52874 = CARTESIAN_POINT ( 'NONE',  ( 1.649999999999951950, 2.500000000000000000, -7.188010851410854052 ) ) ;
#52875 = ORIENTED_EDGE ( 'NONE', *, *, #107637, .T. ) ;
#52876 = VECTOR ( 'NONE', #20152, 1000.000000000000000 ) ;
#52877 = CARTESIAN_POINT ( 'NONE',  ( 7.099999999999928590, 12.50000000000000000, -4.265033745738164406 ) ) ;
#52878 = CARTESIAN_POINT ( 'NONE',  ( 9.149999999999916866, 2.500000000000000000, -1.472243186433550122 ) ) ;
#52879 = CARTESIAN_POINT ( 'NONE',  ( -3.150000000000033218, 2.500000000000000000, -6.941600689897078347 ) ) ;
#52880 = CARTESIAN_POINT ( 'NONE',  ( -14.34999999999998543, 12.50000000000000000, 1.753560074763288013 ) ) ;
#52881 = FACE_OUTER_BOUND ( 'NONE', #99700, .T. ) ;
#52882 = EDGE_LOOP ( 'NONE', ( #51993, #77858, #50600, #31685 ) ) ;
#52883 = CARTESIAN_POINT ( 'NONE',  ( 10.19999999999991047, 2.500000000000000000, -3.883716857408426648 ) ) ;
#52884 = EDGE_CURVE ( 'NONE', #20798, #60736, #111355, .T. ) ;
#52885 = CARTESIAN_POINT ( 'NONE',  ( 32.28071041560937715, -1.401423001991335182, 4.680142630335650367 ) ) ;
#52886 = ORIENTED_EDGE ( 'NONE', *, *, #126095, .T. ) ;
#52887 = ORIENTED_EDGE ( 'NONE', *, *, #45132, .T. ) ;
#52888 = AXIS2_PLACEMENT_3D ( 'NONE', #73334, #74633, #114545 ) ;
#52889 = CARTESIAN_POINT ( 'NONE',  ( 186.0885416670080872, -6.551208109652273848, -3.782341765625003571 ) ) ;
#52890 = DIRECTION ( 'NONE',  ( 0.000000000000000000, -0.000000000000000000, 1.000000000000000000 ) ) ;
#52891 = DIRECTION ( 'NONE',  ( -0.000000000000000000, 1.000000000000000000, -0.000000000000000000 ) ) ;
#52892 = CARTESIAN_POINT ( 'NONE',  ( 11.64999999999990443, 2.500000000000000000, 2.857883832488649301 ) ) ;
#52893 = FACE_OUTER_BOUND ( 'NONE', #64491, .T. ) ;
#52894 = EDGE_CURVE ( 'NONE', #26891, #112496, #96692, .T. ) ;
#52895 = CIRCLE ( 'NONE', #86320, 0.1000000000000002554 ) ;
#52896 = CARTESIAN_POINT ( 'NONE',  ( -3.550000000000030909, 12.50000000000000000, -6.776507416713040577 ) ) ;
#52897 = DIRECTION ( 'NONE',  ( 0.000000000000000000, 0.000000000000000000, 1.000000000000000000 ) ) ;
#52898 = AXIS2_PLACEMENT_3D ( 'NONE', #60860, #60241, #81772 ) ;
#52899 = PLANE ( 'NONE',  #40687 ) ;
#52900 = CARTESIAN_POINT ( 'NONE',  ( 5.399999999999932854, 2.500000000000000000, 3.537306695894645081 ) ) ;
#52901 = CONICAL_SURFACE ( 'NONE', #17359, 0.1000000000000002554, 0.003490658503988666988 ) ;
#52902 = AXIS2_PLACEMENT_3D ( 'NONE', #112936, #91358, #31807 ) ;
#52903 = CARTESIAN_POINT ( 'NONE',  ( 3.299999999999944755, 2.500000000000000000, -2.385244779468109755E-15 ) ) ;
#52904 = ORIENTED_EDGE ( 'NONE', *, *, #48424, .F. ) ;
#52905 = AXIS2_PLACEMENT_3D ( 'NONE', #26805, #98752, #56878 ) ;
#52906 = ORIENTED_EDGE ( 'NONE', *, *, #29059, .F. ) ;
#52907 = CONICAL_SURFACE ( 'NONE', #109326, 0.1000000000000002554, 0.003490658503988666988 ) ;
#52908 = ORIENTED_EDGE ( 'NONE', *, *, #85329, .F. ) ;
#52909 = CIRCLE ( 'NONE', #126047, 0.06509327318403745899 ) ;
#52910 = AXIS2_PLACEMENT_3D ( 'NONE', #120959, #31316, #12282 ) ;
#52911 = EDGE_LOOP ( 'NONE', ( #113912, #81330 ) ) ;
#52912 = FACE_OUTER_BOUND ( 'NONE', #49814, .T. ) ;
#52913 = DIRECTION ( 'NONE',  ( 0.000000000000000000, 0.000000000000000000, 1.000000000000000000 ) ) ;
#52914 = AXIS2_PLACEMENT_3D ( 'NONE', #69466, #60942, #108748 ) ;
#52915 = ORIENTED_EDGE ( 'NONE', *, *, #30978, .F. ) ;
#52916 = DIRECTION ( 'NONE',  ( 0.000000000000000000, 1.000000000000000000, 0.000000000000000000 ) ) ;
#52917 = DIRECTION ( 'NONE',  ( -0.000000000000000000, -1.000000000000000000, -0.000000000000000000 ) ) ;
#52919 = VERTEX_POINT ( 'NONE', #104082 ) ;
#52918 = CARTESIAN_POINT ( 'NONE',  ( -11.64999999999999680, 2.500000000000000000, 2.065063509461097624 ) ) ;
#52920 = DIRECTION ( 'NONE',  ( -0.000000000000000000, 1.000000000000000000, -0.000000000000000000 ) ) ;
#52922 = PLANE ( 'NONE',  #102285 ) ;
#52921 = AXIS2_PLACEMENT_3D ( 'NONE', #86579, #115371, #8016 ) ;
#52923 = ORIENTED_EDGE ( 'NONE', *, *, #44218, .T. ) ;
#52924 = ORIENTED_EDGE ( 'NONE', *, *, #68032, .F. ) ;
#52925 = ORIENTED_EDGE ( 'NONE', *, *, #104485, .T. ) ;
#52926 = ORIENTED_EDGE ( 'NONE', *, *, #107088, .F. ) ;
#52927 = CARTESIAN_POINT ( 'NONE',  ( 12.89999999999990088, 2.500000000000000000, 4.330127018922196314 ) ) ;
#52928 = DIRECTION ( 'NONE',  ( 0.000000000000000000, 0.000000000000000000, 1.000000000000000000 ) ) ;
#52929 = CARTESIAN_POINT ( 'NONE',  ( 6.849999999999929479, 12.50000000000000000, 6.083687093685482772 ) ) ;
#52930 = CIRCLE ( 'NONE', #111503, 0.1000000000000002554 ) ;
#52931 = FACE_OUTER_BOUND ( 'NONE', #107562, .T. ) ;
#52932 = EDGE_CURVE ( 'NONE', #106610, #65076, #128015, .T. ) ;
#52933 = AXIS2_PLACEMENT_3D ( 'NONE', #85176, #14479, #115923 ) ;
#52934 = EDGE_LOOP ( 'NONE', ( #55623, #3377 ) ) ;
#52935 = DIRECTION ( 'NONE',  ( -4.274815082592931898E-19, -0.9999939076577903929, -0.003490651415223739937 ) ) ;
#52936 = ORIENTED_EDGE ( 'NONE', *, *, #60767, .F. ) ;
#52937 = CARTESIAN_POINT ( 'NONE',  ( -3.350000000000028511, 12.50000000000000000, -1.472243186433550122 ) ) ;
#52938 = CARTESIAN_POINT ( 'NONE',  ( 7.306656945292925975, -2.500000000000506706, -9.704971168059893571 ) ) ;
#52939 = EDGE_CURVE ( 'NONE', #126753, #103801, #50749, .T. ) ;
#52940 = DIRECTION ( 'NONE',  ( 0.000000000000000000, 0.000000000000000000, 1.000000000000000000 ) ) ;
#52941 = PLANE ( 'NONE',  #38085 ) ;
#52942 = AXIS2_PLACEMENT_3D ( 'NONE', #22871, #63422, #2542 ) ;
#52943 = EDGE_CURVE ( 'NONE', #29223, #54633, #36076, .T. ) ;
#52944 = CIRCLE ( 'NONE', #13211, 0.1000000000000002554 ) ;
#52945 = AXIS2_PLACEMENT_3D ( 'NONE', #45614, #55423, #85521 ) ;
#52946 = ORIENTED_EDGE ( 'NONE', *, *, #100693, .F. ) ;
#52947 = VECTOR ( 'NONE', #88145, 1000.000000000000000 ) ;
#52948 = ORIENTED_EDGE ( 'NONE', *, *, #11316, .F. ) ;
#52949 = EDGE_CURVE ( 'NONE', #56299, #102282, #56982, .T. ) ;
#52951 = EDGE_LOOP ( 'NONE', ( #5434, #88004, #124589, #90970 ) ) ;
#52950 = EDGE_CURVE ( 'NONE', #87296, #112974, #84436, .T. ) ;
#52952 = FACE_OUTER_BOUND ( 'NONE', #125605, .T. ) ;
#52953 = CARTESIAN_POINT ( 'NONE',  ( -12.89999999999999147, 2.500000000000000000, 0.1000000000000018513 ) ) ;
#52954 = DIRECTION ( 'NONE',  ( -0.000000000000000000, -1.000000000000000000, -0.000000000000000000 ) ) ;
#52955 = EDGE_CURVE ( 'NONE', #30530, #114894, #63518, .T. ) ;
#52956 = FACE_BOUND ( 'NONE', #56899, .T. ) ;
#52957 = DIRECTION ( 'NONE',  ( 0.000000000000000000, 0.000000000000000000, 1.000000000000000000 ) ) ;
#52958 = CARTESIAN_POINT ( 'NONE',  ( 12.49999999999990408, 2.500000000000000000, -3.637306695894650055 ) ) ;
#52959 = CARTESIAN_POINT ( 'NONE',  ( -9.350000000000004974, 2.500000000000000000, 6.941600689897073018 ) ) ;
#52960 = AXIS2_PLACEMENT_3D ( 'NONE', #98426, #59845, #68982 ) ;
#52961 = DIRECTION ( 'NONE',  ( -1.000000000000000000, -0.000000000000000000, -0.000000000000000000 ) ) ;
#52962 = CARTESIAN_POINT ( 'NONE',  ( 184.2500000000000000, 9.429780353434619030E-16, -7.700000000000000178 ) ) ;
#52963 = AXIS2_PLACEMENT_3D ( 'NONE', #17375, #66487, #4324 ) ;
#52964 = DIRECTION ( 'NONE',  ( 0.000000000000000000, 1.000000000000000000, 0.000000000000000000 ) ) ;
#52965 = EDGE_LOOP ( 'NONE', ( #14727, #29996, #76676, #89538 ) ) ;
#52966 = DIRECTION ( 'NONE',  ( 0.000000000000000000, 1.000000000000000000, 0.000000000000000000 ) ) ;
#52967 = ORIENTED_EDGE ( 'NONE', *, *, #66364, .T. ) ;
#52968 = ORIENTED_EDGE ( 'NONE', *, *, #64482, .F. ) ;
#52969 = FACE_OUTER_BOUND ( 'NONE', #103735, .T. ) ;
#52970 = DIRECTION ( 'NONE',  ( 0.000000000000000000, 0.000000000000000000, -1.000000000000000000 ) ) ;
#52971 = FACE_BOUND ( 'NONE', #20108, .T. ) ;
#52972 = DIRECTION ( 'NONE',  ( -0.000000000000000000, -1.000000000000000000, -0.000000000000000000 ) ) ;
#52974 = ORIENTED_EDGE ( 'NONE', *, *, #98971, .F. ) ;
#52973 = AXIS2_PLACEMENT_3D ( 'NONE', #15004, #25485, #124990 ) ;
#52976 = AXIS2_PLACEMENT_3D ( 'NONE', #31355, #111160, #101373 ) ;
#52975 = LINE ( 'NONE', #83729, #82231 ) ;
#52977 = DIRECTION ( 'NONE',  ( -4.274815082592931898E-19, -0.9999939076577903929, -0.003490651415223739937 ) ) ;
#52978 = ORIENTED_EDGE ( 'NONE', *, *, #117003, .T. ) ;
#52979 = DIRECTION ( 'NONE',  ( 0.000000000000000000, 1.000000000000000000, 0.000000000000000000 ) ) ;
#52980 = PLANE ( 'NONE',  #32415 ) ;
#52981 = CIRCLE ( 'NONE', #2804, 0.1000000000000002554 ) ;
#52982 = CONICAL_SURFACE ( 'NONE', #11204, 0.1000000000000000472, 0.003490658503988666988 ) ;
#52983 = AXIS2_PLACEMENT_3D ( 'NONE', #98679, #68583, #118979 ) ;
#52984 = EDGE_CURVE ( 'NONE', #66538, #105977, #73317, .T. ) ;
#52985 = ORIENTED_EDGE ( 'NONE', *, *, #124170, .F. ) ;
#52986 = EDGE_CURVE ( 'NONE', #117024, #123082, #54938, .T. ) ;
#52987 = DIRECTION ( 'NONE',  ( -4.274815082592931898E-19, -0.9999939076577903929, -0.003490651415223739937 ) ) ;
#52988 = DIRECTION ( 'NONE',  ( 0.000000000000000000, 0.000000000000000000, 1.000000000000000000 ) ) ;
#52989 = EDGE_CURVE ( 'NONE', #67694, #97521, #24875, .T. ) ;
#52990 = CONICAL_SURFACE ( 'NONE', #67648, 0.09999999999999982514, 0.003490658503988666988 ) ;
#52991 = ORIENTED_EDGE ( 'NONE', *, *, #36264, .T. ) ;
#52992 = CONICAL_SURFACE ( 'NONE', #25804, 0.1000000000000000472, 0.003490658503988666988 ) ;
#52993 = DIRECTION ( 'NONE',  ( -0.000000000000000000, 1.000000000000000000, -0.000000000000000000 ) ) ;
#52994 = DIRECTION ( 'NONE',  ( -0.000000000000000000, 1.000000000000000000, -0.000000000000000000 ) ) ;
#52995 = LINE ( 'NONE', #81167, #78623 ) ;
#52996 = AXIS2_PLACEMENT_3D ( 'NONE', #29214, #118859, #119496 ) ;
#52997 = EDGE_CURVE ( 'NONE', #87479, #43021, #69507, .T. ) ;
#52999 = ORIENTED_EDGE ( 'NONE', *, *, #77810, .F. ) ;
#52998 = AXIS2_PLACEMENT_3D ( 'NONE', #14548, #25033, #114062 ) ;
#53000 = ORIENTED_EDGE ( 'NONE', *, *, #68882, .F. ) ;
#53001 = EDGE_CURVE ( 'NONE', #123441, #18337, #45169, .T. ) ;
#53002 = FACE_OUTER_BOUND ( 'NONE', #12681, .T. ) ;
#53004 = ORIENTED_EDGE ( 'NONE', *, *, #65149, .F. ) ;
#53003 = EDGE_CURVE ( 'NONE', #88166, #129005, #71578, .T. ) ;
#53005 = LINE ( 'NONE', #13045, #97173 ) ;
#53006 = DIRECTION ( 'NONE',  ( 0.000000000000000000, 1.000000000000000000, 0.000000000000000000 ) ) ;
#53007 = EDGE_CURVE ( 'NONE', #66455, #6359, #88280, .T. ) ;
#53008 = EDGE_CURVE ( 'NONE', #82164, #53598, #8864, .T. ) ;
#53009 = VERTEX_POINT ( 'NONE', #26809 ) ;
#53010 = DIRECTION ( 'NONE',  ( 0.000000000000000000, 0.000000000000000000, -1.000000000000000000 ) ) ;
#53011 = CARTESIAN_POINT ( 'NONE',  ( -0.4000000000000339950, 2.500000000000000000, 0.5928203230275517210 ) ) ;
#53012 = DIRECTION ( 'NONE',  ( 0.000000000000000000, 1.000000000000000000, 0.000000000000000000 ) ) ;
#53013 = DIRECTION ( 'NONE',  ( 0.000000000000000000, 0.000000000000000000, 1.000000000000000000 ) ) ;
#53015 = EDGE_CURVE ( 'NONE', #22721, #98931, #31876, .T. ) ;
#53014 = DIRECTION ( 'NONE',  ( -4.274815082592931898E-19, -0.9999939076577903929, -0.003490651415223739937 ) ) ;
#53016 = VECTOR ( 'NONE', #113962, 1000.000000000000000 ) ;
#53017 = VERTEX_POINT ( 'NONE', #40345 ) ;
#53018 = ORIENTED_EDGE ( 'NONE', *, *, #86026, .T. ) ;
#53019 = DIRECTION ( 'NONE',  ( 0.000000000000000000, 1.000000000000000000, 0.000000000000000000 ) ) ;
#53020 = ORIENTED_EDGE ( 'NONE', *, *, #15968, .F. ) ;
#53021 = CARTESIAN_POINT ( 'NONE',  ( -11.44999999999999929, 2.500000000000000000, -6.248780366869523206 ) ) ;
#53023 = ORIENTED_EDGE ( 'NONE', *, *, #74553, .T. ) ;
#53022 = VERTEX_POINT ( 'NONE', #107940 ) ;
#53024 = ORIENTED_EDGE ( 'NONE', *, *, #84045, .T. ) ;
#53025 = CARTESIAN_POINT ( 'NONE',  ( -4.800000000000026468, 2.500000000000000000, -4.676537180435978769 ) ) ;
#53026 = AXIS2_PLACEMENT_3D ( 'NONE', #105241, #15561, #95432 ) ;
#53027 = VECTOR ( 'NONE', #47345, 1000.000000000000000 ) ;
#53028 = DIRECTION ( 'NONE',  ( 0.000000000000000000, 0.000000000000000000, 1.000000000000000000 ) ) ;
#53029 = AXIS2_PLACEMENT_3D ( 'NONE', #73694, #14127, #95286 ) ;
#53030 = DIRECTION ( 'NONE',  ( -0.000000000000000000, -1.000000000000000000, -0.000000000000000000 ) ) ;
#53031 = FACE_OUTER_BOUND ( 'NONE', #114333, .T. ) ;
#53032 = CARTESIAN_POINT ( 'NONE',  ( 9.149999999999920419, 2.500000000000000000, -7.088010851410853519 ) ) ;
#53033 = PLANE ( 'NONE',  #33989 ) ;
#53034 = CARTESIAN_POINT ( 'NONE',  ( 12.89999999999990266, 2.500000000000000000, -5.122947341949753763 ) ) ;
#53035 = CARTESIAN_POINT ( 'NONE',  ( 7.899999999999924860, 12.50000000000000000, -3.637306695894650055 ) ) ;
#53036 = EDGE_CURVE ( 'NONE', #112593, #11592, #7801, .T. ) ;
#53037 = AXIS2_PLACEMENT_3D ( 'NONE', #58759, #129460, #78419 ) ;
#53038 = AXIS2_PLACEMENT_3D ( 'NONE', #12140, #92650, #120820 ) ;
#53039 = CYLINDRICAL_SURFACE ( 'NONE', #51940, 5.000000000000004441 ) ;
#53040 = CIRCLE ( 'NONE', #94890, 0.09999999999999999167 ) ;
#53041 = EDGE_LOOP ( 'NONE', ( #125787, #58248 ) ) ;
#53042 = AXIS2_PLACEMENT_3D ( 'NONE', #84476, #94945, #29268 ) ;
#53043 = DIRECTION ( 'NONE',  ( 0.000000000000000000, 1.000000000000000000, 0.000000000000000000 ) ) ;
#53044 = ORIENTED_EDGE ( 'NONE', *, *, #64285, .F. ) ;
#53045 = ORIENTED_EDGE ( 'NONE', *, *, #28759, .F. ) ;
#53046 = CARTESIAN_POINT ( 'NONE',  ( -13.74999999999995381, 12.50000000000000000, -2.099970236277062252 ) ) ;
#53047 = DIRECTION ( 'NONE',  ( -0.000000000000000000, -1.000000000000000000, -0.000000000000000000 ) ) ;
#53048 = FACE_OUTER_BOUND ( 'NONE', #15311, .T. ) ;
#53049 = FACE_OUTER_BOUND ( 'NONE', #12664, .T. ) ;
#53050 = EDGE_CURVE ( 'NONE', #95287, #67756, #121745, .T. ) ;
#53051 = DIRECTION ( 'NONE',  ( 0.000000000000000000, 0.000000000000000000, -1.000000000000000000 ) ) ;
#53052 = AXIS2_PLACEMENT_3D ( 'NONE', #6077, #96395, #46672 ) ;
#53053 = PLANE ( 'NONE',  #40948 ) ;
#53054 = AXIS2_PLACEMENT_3D ( 'NONE', #60481, #92487, #50633 ) ;
#53055 = AXIS2_PLACEMENT_3D ( 'NONE', #114342, #123511, #15488 ) ;
#53056 = DIRECTION ( 'NONE',  ( -0.000000000000000000, -1.000000000000000000, -0.000000000000000000 ) ) ;
#53057 = VERTEX_POINT ( 'NONE', #66716 ) ;
#53058 = CIRCLE ( 'NONE', #111535, 0.09999999999999982514 ) ;
#53059 = AXIS2_PLACEMENT_3D ( 'NONE', #57801, #98344, #56490 ) ;
#53060 = EDGE_LOOP ( 'NONE', ( #72968, #104951, #47023, #29153 ) ) ;
#53061 = ORIENTED_EDGE ( 'NONE', *, *, #34029, .F. ) ;
#53062 = ORIENTED_EDGE ( 'NONE', *, *, #91397, .F. ) ;
#53063 = ORIENTED_EDGE ( 'NONE', *, *, #7885, .F. ) ;
#53064 = DIRECTION ( 'NONE',  ( -0.000000000000000000, -1.000000000000000000, -0.000000000000000000 ) ) ;
#53065 = DIRECTION ( 'NONE',  ( 0.000000000000000000, -0.9999939076577903929, 0.003490651415223739937 ) ) ;
#53066 = CARTESIAN_POINT ( 'NONE',  ( 0.6499999999999543920, 12.50000000000000000, 6.083687093685483660 ) ) ;
#53067 = CARTESIAN_POINT ( 'NONE',  ( -0.8500000000000395017, 12.50000000000000000, 2.165063509461097713 ) ) ;
#53068 = FACE_OUTER_BOUND ( 'NONE', #50676, .T. ) ;
#53069 = ORIENTED_EDGE ( 'NONE', *, *, #3017, .T. ) ;
#53071 = AXIS2_PLACEMENT_3D ( 'NONE', #14848, #66547, #125475 ) ;
#53070 = DIRECTION ( 'NONE',  ( -0.000000000000000000, -1.000000000000000000, -0.000000000000000000 ) ) ;
#53072 = CIRCLE ( 'NONE', #76057, 0.1000000000000002554 ) ;
#53073 = DIRECTION ( 'NONE',  ( -0.000000000000000000, 1.000000000000000000, -0.000000000000000000 ) ) ;
#53074 = FACE_OUTER_BOUND ( 'NONE', #72901, .T. ) ;
#53075 = CARTESIAN_POINT ( 'NONE',  ( 10.84999999999990905, 12.50000000000000000, 2.857883832488649301 ) ) ;
#53076 = VERTEX_POINT ( 'NONE', #18269 ) ;
#53077 = AXIS2_PLACEMENT_3D ( 'NONE', #79619, #21337, #41657 ) ;
#53078 = CIRCLE ( 'NONE', #843, 0.06509327318403745899 ) ;
#53079 = ORIENTED_EDGE ( 'NONE', *, *, #54680, .F. ) ;
#53080 = ORIENTED_EDGE ( 'NONE', *, *, #126696, .F. ) ;
#53081 = AXIS2_PLACEMENT_3D ( 'NONE', #121158, #62252, #122461 ) ;
#53082 = DIRECTION ( 'NONE',  ( 0.000000000000000000, 1.000000000000000000, 0.000000000000000000 ) ) ;
#53083 = CARTESIAN_POINT ( 'NONE',  ( 1.649999999999950617, 2.500000000000000000, 2.265063509461097357 ) ) ;
#53084 = DIRECTION ( 'NONE',  ( 0.000000000000000000, 0.000000000000000000, 1.000000000000000000 ) ) ;
#53085 = VECTOR ( 'NONE', #3821, 1000.000000000000000 ) ;
#53086 = AXIS2_PLACEMENT_3D ( 'NONE', #27560, #124510, #106773 ) ;
#53088 = EDGE_CURVE ( 'NONE', #99498, #96622, #65301, .T. ) ;
#53087 = AXIS2_PLACEMENT_3D ( 'NONE', #46054, #85945, #57149 ) ;
#53089 = AXIS2_PLACEMENT_3D ( 'NONE', #29542, #61598, #69450 ) ;
#53090 = VERTEX_POINT ( 'NONE', #56880 ) ;
#53091 = CARTESIAN_POINT ( 'NONE',  ( 2.499999999999947153, 12.50000000000000000, 3.637306695894644726 ) ) ;
#53092 = DIRECTION ( 'NONE',  ( 0.000000000000000000, 1.000000000000000000, 0.000000000000000000 ) ) ;
#53093 = CARTESIAN_POINT ( 'NONE',  ( 5.449999999999934452, 12.50000000000000000, 2.165063509461097713 ) ) ;
#53094 = CARTESIAN_POINT ( 'NONE',  ( -7.100000000000013856, 12.50000000000000000, 3.637306695894644726 ) ) ;
#53095 = ADVANCED_FACE ( 'NONE', ( #99902 ), #82036, .T. ) ;
#53096 = DIRECTION ( 'NONE',  ( 0.000000000000000000, 0.000000000000000000, 1.000000000000000000 ) ) ;
#53097 = ORIENTED_EDGE ( 'NONE', *, *, #111799, .F. ) ;
#53098 = ADVANCED_FACE ( 'NONE', ( #35982 ), #77920, .T. ) ;
#53099 = ADVANCED_FACE ( 'NONE', ( #116461 ), #34020, .T. ) ;
#53100 = ORIENTED_EDGE ( 'NONE', *, *, #85889, .T. ) ;
#53101 = EDGE_CURVE ( 'NONE', #53201, #53951, #61214, .T. ) ;
#53103 = EDGE_CURVE ( 'NONE', #125340, #95314, #77198, .T. ) ;
#53102 = DIRECTION ( 'NONE',  ( 0.000000000000000000, -0.9999939076577903929, 0.003490651415223739937 ) ) ;
#53104 = EDGE_CURVE ( 'NONE', #53828, #121663, #91083, .T. ) ;
#53105 = DIRECTION ( 'NONE',  ( 0.000000000000000000, 1.000000000000000000, 0.000000000000000000 ) ) ;
#53106 = DIRECTION ( 'NONE',  ( -0.000000000000000000, 1.000000000000000000, -0.000000000000000000 ) ) ;
#53107 = CONICAL_SURFACE ( 'NONE', #126263, 0.1000000000000002554, 0.003490658503988666988 ) ;
#53108 = DIRECTION ( 'NONE',  ( -0.000000000000000000, -1.000000000000000000, -0.000000000000000000 ) ) ;
#53109 = CARTESIAN_POINT ( 'NONE',  ( 17.49862860983166257, -2.500000000000000000, -4.081131818001380474 ) ) ;
#53110 = ORIENTED_EDGE ( 'NONE', *, *, #123733, .F. ) ;
#53111 = ORIENTED_EDGE ( 'NONE', *, *, #123153, .F. ) ;
#53112 = CARTESIAN_POINT ( 'NONE',  ( 10.64999999999990976, 12.50000000000000000, 2.511473670974873507 ) ) ;
#53113 = DIRECTION ( 'NONE',  ( -0.000000000000000000, 1.000000000000000000, -0.000000000000000000 ) ) ;
#53114 = EDGE_CURVE ( 'NONE', #87285, #46700, #117606, .T. ) ;
#53115 = FACE_OUTER_BOUND ( 'NONE', #104694, .T. ) ;
#53116 = LINE ( 'NONE', #96093, #74852 ) ;
#53117 = FACE_OUTER_BOUND ( 'NONE', #64522, .T. ) ;
#53118 = ORIENTED_EDGE ( 'NONE', *, *, #78984, .F. ) ;
#53119 = CONICAL_SURFACE ( 'NONE', #28076, 0.1000000000000002554, 0.003490658503988666988 ) ;
#53121 = EDGE_CURVE ( 'NONE', #117879, #75839, #67335, .T. ) ;
#53120 = DIRECTION ( 'NONE',  ( -0.000000000000000000, -1.000000000000000000, -0.000000000000000000 ) ) ;
#53122 = FACE_OUTER_BOUND ( 'NONE', #37251, .T. ) ;
#53123 = ORIENTED_EDGE ( 'NONE', *, *, #10108, .T. ) ;
#53124 = LINE ( 'NONE', #43314, #51099 ) ;
#53125 = CIRCLE ( 'NONE', #46562, 4.000000000000000000 ) ;
#53126 = EDGE_LOOP ( 'NONE', ( #127364, #76166 ) ) ;
#53127 = PLANE ( 'NONE',  #129009 ) ;
#53128 = AXIS2_PLACEMENT_3D ( 'NONE', #3659, #73051, #112966 ) ;
#53129 = EDGE_LOOP ( 'NONE', ( #37926, #90205 ) ) ;
#53130 = CARTESIAN_POINT ( 'NONE',  ( -3.350000000000031619, 12.50000000000000000, -7.188010851410854052 ) ) ;
#53131 = DIRECTION ( 'NONE',  ( 0.000000000000000000, -0.9999939076577903929, 0.003490651415223739937 ) ) ;
#53132 = ORIENTED_EDGE ( 'NONE', *, *, #72768, .T. ) ;
#53133 = ORIENTED_EDGE ( 'NONE', *, *, #101279, .T. ) ;
#53134 = CARTESIAN_POINT ( 'NONE',  ( 185.4218750003414016, 0.000000000000000000, 7.564683531250000925 ) ) ;
#53135 = DIRECTION ( 'NONE',  ( 0.000000000000000000, 0.000000000000000000, 1.000000000000000000 ) ) ;
#53136 = CARTESIAN_POINT ( 'NONE',  ( 186.7968750003414300, 8.734944146203032389, 5.348610694689227483E-16 ) ) ;
#53137 = CARTESIAN_POINT ( 'NONE',  ( 185.6093750003413732, 9.264065473108010111E-16, -7.564683531250000925 ) ) ;
#53138 = AXIS2_PLACEMENT_3D ( 'NONE', #85779, #45880, #36056 ) ;
#53140 = CIRCLE ( 'NONE', #69866, 0.1000000000000000472 ) ;
#53139 = FACE_OUTER_BOUND ( 'NONE', #60771, .T. ) ;
#53141 = VECTOR ( 'NONE', #79586, 1000.000000000000000 ) ;
#53142 = CARTESIAN_POINT ( 'NONE',  ( -9.200000000000006395, 12.50000000000000000, -2.385244779468109755E-15 ) ) ;
#53143 = CARTESIAN_POINT ( 'NONE',  ( -1.250000000000001110, 2.500000000000000000, -2.165063509461101710 ) ) ;
#53144 = CARTESIAN_POINT ( 'NONE',  ( -11.24999999999996270, 2.500000000000000000, 2.065063509461097624 ) ) ;
#53145 = CONICAL_SURFACE ( 'NONE', #59428, 0.09999999999999982514, 0.003490658503988666988 ) ;
#53146 = LINE ( 'NONE', #11272, #15000 ) ;
#53147 = EDGE_CURVE ( 'NONE', #49253, #32790, #127587, .T. ) ;
#53148 = ORIENTED_EDGE ( 'NONE', *, *, #38049, .F. ) ;
#53149 = ADVANCED_FACE ( 'NONE', ( #68015 ), #61920, .T. ) ;
#53150 = ORIENTED_EDGE ( 'NONE', *, *, #23881, .F. ) ;
#53151 = LINE ( 'NONE', #5317, #57026 ) ;
#53152 = EDGE_LOOP ( 'NONE', ( #88773, #68707 ) ) ;
#53153 = DIRECTION ( 'NONE',  ( 0.000000000000000000, 1.000000000000000000, 0.000000000000000000 ) ) ;
#53154 = DIRECTION ( 'NONE',  ( 0.000000000000000000, 1.000000000000000000, 0.000000000000000000 ) ) ;
#53155 = CARTESIAN_POINT ( 'NONE',  ( -0.8500000000000386136, 2.500000000000000000, 2.857883832488649301 ) ) ;
#53157 = VERTEX_POINT ( 'NONE', #41001 ) ;
#53156 = EDGE_LOOP ( 'NONE', ( #79376, #30940, #129311, #118323 ) ) ;
#53158 = FACE_BOUND ( 'NONE', #27712, .T. ) ;
#53159 = VERTEX_POINT ( 'NONE', #60632 ) ;
#53160 = EDGE_CURVE ( 'NONE', #99317, #62165, #100526, .T. ) ;
#53161 = CARTESIAN_POINT ( 'NONE',  ( -12.69999999999999396, 2.500000000000000000, -3.983716857408423628 ) ) ;
#53162 = DIRECTION ( 'NONE',  ( -0.000000000000000000, 1.000000000000000000, -0.000000000000000000 ) ) ;
#53163 = EDGE_CURVE ( 'NONE', #9132, #39516, #52092, .T. ) ;
#53164 = CARTESIAN_POINT ( 'NONE',  ( -11.64999999999999680, 2.500000000000000000, 6.395190528383296602 ) ) ;
#53165 = DIRECTION ( 'NONE',  ( 0.000000000000000000, -0.000000000000000000, 1.000000000000000000 ) ) ;
#53166 = DIRECTION ( 'NONE',  ( 0.000000000000000000, -0.9999939076577903929, 0.003490651415223739937 ) ) ;
#53167 = ADVANCED_FACE ( 'NONE', ( #80905 ), #1679, .T. ) ;
#53169 = CARTESIAN_POINT ( 'NONE',  ( 2.299999999999948752, 2.500000000000000000, -3.983716857408426293 ) ) ;
#53168 = VECTOR ( 'NONE', #37286, 1000.000000000000000 ) ;
#53170 = VECTOR ( 'NONE', #45012, 1000.000000000000000 ) ;
#53171 = DIRECTION ( 'NONE',  ( -0.000000000000000000, 1.000000000000000000, -0.000000000000000000 ) ) ;
#53172 = CARTESIAN_POINT ( 'NONE',  ( 14.14999999999989377, 2.500000000000000000, -2.957883832488653830 ) ) ;
#53173 = AXIS2_PLACEMENT_3D ( 'NONE', #114997, #57388, #15511 ) ;
#53174 = CIRCLE ( 'NONE', #48970, 0.06509327318403743123 ) ;
#53175 = PLANE ( 'NONE',  #91391 ) ;
#53176 = DIRECTION ( 'NONE',  ( 0.000000000000000000, 0.000000000000000000, -1.000000000000000000 ) ) ;
#53178 = ADVANCED_FACE ( 'NONE', ( #21323 ), #4750, .T. ) ;
#53177 = DIRECTION ( 'NONE',  ( 0.000000000000000000, 1.000000000000000000, 0.000000000000000000 ) ) ;
#53179 = AXIS2_PLACEMENT_3D ( 'NONE', #15896, #117293, #37499 ) ;
#53181 = VERTEX_POINT ( 'NONE', #43574 ) ;
#53180 = AXIS2_PLACEMENT_3D ( 'NONE', #105993, #30024, #29380 ) ;
#53182 = VERTEX_POINT ( 'NONE', #23251 ) ;
#53183 = ORIENTED_EDGE ( 'NONE', *, *, #67077, .F. ) ;
#53185 = CARTESIAN_POINT ( 'NONE',  ( -7.900000000000014566, 12.50000000000000000, -3.572213422710612374 ) ) ;
#53184 = AXIS2_PLACEMENT_3D ( 'NONE', #111640, #33097, #52708 ) ;
#53186 = ORIENTED_EDGE ( 'NONE', *, *, #46162, .T. ) ;
#53187 = DIRECTION ( 'NONE',  ( -4.274815082592931898E-19, -0.9999939076577903929, -0.003490651415223739937 ) ) ;
#53189 = ORIENTED_EDGE ( 'NONE', *, *, #18097, .T. ) ;
#53188 = ORIENTED_EDGE ( 'NONE', *, *, #13914, .F. ) ;
#53190 = ORIENTED_EDGE ( 'NONE', *, *, #77498, .F. ) ;
#53191 = DIRECTION ( 'NONE',  ( 0.000000000000000000, -0.000000000000000000, 1.000000000000000000 ) ) ;
#53192 = VECTOR ( 'NONE', #69956, 1000.000000000000000 ) ;
#53193 = AXIS2_PLACEMENT_3D ( 'NONE', #66798, #55065, #94995 ) ;
#53194 = CARTESIAN_POINT ( 'NONE',  ( -10.85000000000000142, 12.50000000000000000, 6.560283801567334372 ) ) ;
#53195 = CARTESIAN_POINT ( 'NONE',  ( 0.000000000000000000, 0.000000000000000000, 0.000000000000000000 ) ) ;
#53196 = CARTESIAN_POINT ( 'NONE',  ( 7.499999999999925393, 2.500000000000000000, -3.537306695894649966 ) ) ;
#53197 = LINE ( 'NONE', #42082, #68588 ) ;
#53198 = AXIS2_PLACEMENT_3D ( 'NONE', #1848, #41809, #81700 ) ;
#53199 = DIRECTION ( 'NONE',  ( 0.000000000000000000, -0.9999939076577903929, 0.003490651415223739937 ) ) ;
#53200 = ADVANCED_FACE ( 'NONE', ( #2314 ), #102472, .T. ) ;
#53201 = VERTEX_POINT ( 'NONE', #10840 ) ;
#53202 = DIRECTION ( 'NONE',  ( 0.000000000000000000, 1.000000000000000000, 0.000000000000000000 ) ) ;
#53203 = EDGE_LOOP ( 'NONE', ( #52549, #60675 ) ) ;
#53204 = ORIENTED_EDGE ( 'NONE', *, *, #85323, .T. ) ;
#53205 = VERTEX_POINT ( 'NONE', #101186 ) ;
#53206 = PLANE ( 'NONE',  #421 ) ;
#53207 = ORIENTED_EDGE ( 'NONE', *, *, #118599, .F. ) ;
#53208 = ORIENTED_EDGE ( 'NONE', *, *, #36444, .F. ) ;
#53209 = VERTEX_POINT ( 'NONE', #41649 ) ;
#53210 = CIRCLE ( 'NONE', #28154, 0.06509327318403745899 ) ;
#53211 = FACE_OUTER_BOUND ( 'NONE', #102114, .T. ) ;
#53212 = PLANE ( 'NONE',  #120760 ) ;
#53213 = CARTESIAN_POINT ( 'NONE',  ( 5.799999999999934985, 12.50000000000000000, -4.330127018922201643 ) ) ;
#53214 = EDGE_CURVE ( 'NONE', #11848, #69557, #22001, .T. ) ;
#53215 = CARTESIAN_POINT ( 'NONE',  ( 13.34999999999989662, 12.50000000000000000, -1.472243186433550122 ) ) ;
#53216 = DIRECTION ( 'NONE',  ( -0.000000000000000000, -1.000000000000000000, -0.000000000000000000 ) ) ;
#53217 = CARTESIAN_POINT ( 'NONE',  ( 129.5000000000000000, -1.375000000000002442, -6.000000000000000888 ) ) ;
#53218 = PLANE ( 'NONE',  #67720 ) ;
#53219 = AXIS2_PLACEMENT_3D ( 'NONE', #103209, #33202, #73110 ) ;
#53220 = AXIS2_PLACEMENT_3D ( 'NONE', #38651, #68720, #108002 ) ;
#53221 = VERTEX_POINT ( 'NONE', #71077 ) ;
#53222 = FACE_OUTER_BOUND ( 'NONE', #84917, .T. ) ;
#53223 = ORIENTED_EDGE ( 'NONE', *, *, #63674, .F. ) ;
#53224 = CARTESIAN_POINT ( 'NONE',  ( 184.8750000000000000, 8.891194145520236347, 5.444286225454521982E-16 ) ) ;
#53225 = EDGE_LOOP ( 'NONE', ( #67640, #74397 ) ) ;
#53226 = EDGE_CURVE ( 'NONE', #68394, #68963, #107163, .T. ) ;
#53227 = VERTEX_POINT ( 'NONE', #33729 ) ;
#53228 = DIRECTION ( 'NONE',  ( -0.000000000000000000, -1.000000000000000000, -0.000000000000000000 ) ) ;
#53229 = DIRECTION ( 'NONE',  ( 0.000000000000000000, 0.000000000000000000, 1.000000000000000000 ) ) ;
#53230 = CIRCLE ( 'NONE', #61543, 0.1000000000000002554 ) ;
#53231 = LINE ( 'NONE', #13277, #36282 ) ;
#53232 = AXIS2_PLACEMENT_3D ( 'NONE', #86446, #104785, #14470 ) ;
#53233 = EDGE_LOOP ( 'NONE', ( #102225, #57110, #96233, #74007 ) ) ;
#53234 = EDGE_LOOP ( 'NONE', ( #86958, #2419 ) ) ;
#53235 = CARTESIAN_POINT ( 'NONE',  ( 7.499999999999960032, 2.500000000000000000, 0.09999999999999772959 ) ) ;
#53236 = DIRECTION ( 'NONE',  ( -4.274815082592931898E-19, -0.9999939076577903929, -0.003490651415223739937 ) ) ;
#53237 = CARTESIAN_POINT ( 'NONE',  ( 6.849999999999930367, 12.50000000000000000, -6.841600689897078702 ) ) ;
#53238 = LINE ( 'NONE', #70934, #107810 ) ;
#53239 = DIRECTION ( 'NONE',  ( 0.000000000000000000, 0.000000000000000000, 1.000000000000000000 ) ) ;
#53240 = ORIENTED_EDGE ( 'NONE', *, *, #52525, .T. ) ;
#53241 = CONICAL_SURFACE ( 'NONE', #128568, 0.1000000000000002554, 0.003490658503988666988 ) ;
#53242 = AXIS2_PLACEMENT_3D ( 'NONE', #57331, #79552, #97248 ) ;
#53243 = CARTESIAN_POINT ( 'NONE',  ( 8.149999999999920419, 2.500000000000000000, -2.511473670974877948 ) ) ;
#53244 = VECTOR ( 'NONE', #33521, 1000.000000000000000 ) ;
#53245 = ORIENTED_EDGE ( 'NONE', *, *, #34044, .T. ) ;
#53246 = AXIS2_PLACEMENT_3D ( 'NONE', #65822, #34458, #16065 ) ;
#53247 = DIRECTION ( 'NONE',  ( 0.000000000000000000, 1.000000000000000000, 0.000000000000000000 ) ) ;
#53248 = EDGE_CURVE ( 'NONE', #24257, #77451, #12142, .T. ) ;
#53249 = CARTESIAN_POINT ( 'NONE',  ( 184.1302083336747160, -4.367472073101514418, -7.564683531250002702 ) ) ;
#53250 = CARTESIAN_POINT ( 'NONE',  ( 2.899999999999946620, 2.500000000000000000, 0.7928203230275495672 ) ) ;
#53251 = CARTESIAN_POINT ( 'NONE',  ( 2.299999999999948752, 2.500000000000000000, -3.983716857408426293 ) ) ;
#53252 = CARTESIAN_POINT ( 'NONE',  ( 2.499999999999947153, 2.500000000000000000, -3.537306695894649966 ) ) ;
#53253 = DIRECTION ( 'NONE',  ( -4.274815082592931898E-19, -0.9999939076577903929, -0.003490651415223739937 ) ) ;
#53254 = ORIENTED_EDGE ( 'NONE', *, *, #88836, .F. ) ;
#53255 = ADVANCED_FACE ( 'NONE', ( #112300 ), #123988, .T. ) ;
#53256 = CARTESIAN_POINT ( 'NONE',  ( -7.300000000000013145, 12.50000000000000000, 3.983716857408420076 ) ) ;
#53258 = CARTESIAN_POINT ( 'NONE',  ( -4.150000000000027889, 2.500000000000000000, -6.495190528383302464 ) ) ;
#53257 = VECTOR ( 'NONE', #110522, 1000.000000000000000 ) ;
#53259 = DIRECTION ( 'NONE',  ( 0.000000000000000000, 0.000000000000000000, 1.000000000000000000 ) ) ;
#53260 = CONICAL_SURFACE ( 'NONE', #90900, 0.1000000000000000472, 0.003490658503988666988 ) ;
#53261 = ORIENTED_EDGE ( 'NONE', *, *, #32968, .F. ) ;
#53262 = AXIS2_PLACEMENT_3D ( 'NONE', #35662, #54014, #65096 ) ;
#53263 = EDGE_CURVE ( 'NONE', #76531, #92529, #75865, .T. ) ;
#53264 = ADVANCED_FACE ( 'NONE', ( #61268 ), #62564, .T. ) ;
#53265 = EDGE_CURVE ( 'NONE', #112003, #67433, #103064, .T. ) ;
#53266 = ADVANCED_FACE ( 'NONE', ( #12781 ), #73816, .T. ) ;
#53267 = DIRECTION ( 'NONE',  ( -0.000000000000000000, 1.000000000000000000, -0.000000000000000000 ) ) ;
#53268 = AXIS2_PLACEMENT_3D ( 'NONE', #123529, #14215, #63980 ) ;
#53269 = AXIS2_PLACEMENT_3D ( 'NONE', #72650, #102722, #41264 ) ;
#53270 = ORIENTED_EDGE ( 'NONE', *, *, #87681, .T. ) ;
#53271 = VECTOR ( 'NONE', #89262, 1000.000000000000000 ) ;
#53272 = EDGE_CURVE ( 'NONE', #76489, #95522, #119785, .T. ) ;
#53273 = CARTESIAN_POINT ( 'NONE',  ( -1.050000000000038236, 12.50000000000000000, -6.148780366869526226 ) ) ;
#53274 = ADVANCED_FACE ( 'NONE', ( #55311 ), #75577, .T. ) ;
#53275 = CIRCLE ( 'NONE', #63731, 0.1000000000000002554 ) ;
#53276 = VERTEX_POINT ( 'NONE', #104406 ) ;
#53277 = CARTESIAN_POINT ( 'NONE',  ( 15.86953761859728118, -2.463355995079595129, -3.896699429482295418 ) ) ;
#53278 = CARTESIAN_POINT ( 'NONE',  ( 8.749999999999921840, 2.500000000000000000, -5.802370205355749988 ) ) ;
#53279 = EDGE_CURVE ( 'NONE', #12586, #3575, #2698, .T. ) ;
#53280 = DIRECTION ( 'NONE',  ( -0.000000000000000000, -1.000000000000000000, -0.000000000000000000 ) ) ;
#53281 = ORIENTED_EDGE ( 'NONE', *, *, #63713, .T. ) ;
#53282 = EDGE_CURVE ( 'NONE', #13086, #35232, #109320, .T. ) ;
#53283 = AXIS2_PLACEMENT_3D ( 'NONE', #45010, #103922, #14233 ) ;
#53284 = AXIS2_PLACEMENT_3D ( 'NONE', #102082, #22888, #12398 ) ;
#53286 = EDGE_CURVE ( 'NONE', #18475, #11947, #46128, .T. ) ;
#53285 = DIRECTION ( 'NONE',  ( 0.000000000000000000, 1.000000000000000000, 0.000000000000000000 ) ) ;
#53287 = DIRECTION ( 'NONE',  ( 0.000000000000000000, 1.000000000000000000, 0.000000000000000000 ) ) ;
#53288 = CIRCLE ( 'NONE', #109718, 0.06509327318403745899 ) ;
#53289 = EDGE_CURVE ( 'NONE', #57293, #13968, #4851, .T. ) ;
#53290 = EDGE_LOOP ( 'NONE', ( #121243, #45815, #49721, #125511 ) ) ;
#53291 = ORIENTED_EDGE ( 'NONE', *, *, #85722, .F. ) ;
#53292 = ORIENTED_EDGE ( 'NONE', *, *, #56026, .T. ) ;
#53293 = CARTESIAN_POINT ( 'NONE',  ( -5.400000000000019895, 2.500000000000000000, 3.537306695894645081 ) ) ;
#53294 = DIRECTION ( 'NONE',  ( -0.000000000000000000, 1.000000000000000000, -0.000000000000000000 ) ) ;
#53295 = LINE ( 'NONE', #40912, #67212 ) ;
#53296 = ORIENTED_EDGE ( 'NONE', *, *, #55506, .F. ) ;
#53297 = DIRECTION ( 'NONE',  ( 0.000000000000000000, 0.000000000000000000, -1.000000000000000000 ) ) ;
#53298 = CARTESIAN_POINT ( 'NONE',  ( -5.200000000000022382, 2.500000000000000000, 4.676537180435972552 ) ) ;
#53299 = CIRCLE ( 'NONE', #97195, 0.06509327318403745899 ) ;
#53300 = VERTEX_POINT ( 'NONE', #54021 ) ;
#53301 = FACE_OUTER_BOUND ( 'NONE', #114451, .T. ) ;
#53302 = DIRECTION ( 'NONE',  ( 0.000000000000000000, -0.9999939076577903929, 0.003490651415223739937 ) ) ;
#53303 = DIRECTION ( 'NONE',  ( -0.000000000000000000, -1.000000000000000000, -0.000000000000000000 ) ) ;
#53304 = CARTESIAN_POINT ( 'NONE',  ( 2.699999999999947331, 2.500000000000000000, -0.4464101615137783252 ) ) ;
#53305 = DIRECTION ( 'NONE',  ( -0.000000000000000000, 1.000000000000000000, -0.000000000000000000 ) ) ;
#53306 = LINE ( 'NONE', #12071, #59765 ) ;
#53307 = DIRECTION ( 'NONE',  ( 0.000000000000000000, -0.000000000000000000, 1.000000000000000000 ) ) ;
#53308 = AXIS2_PLACEMENT_3D ( 'NONE', #93248, #31118, #102420 ) ;
#53309 = AXIS2_PLACEMENT_3D ( 'NONE', #109795, #127503, #110427 ) ;
#53310 = ORIENTED_EDGE ( 'NONE', *, *, #50975, .F. ) ;
#53311 = ORIENTED_EDGE ( 'NONE', *, *, #9492, .T. ) ;
#53312 = ORIENTED_EDGE ( 'NONE', *, *, #123634, .T. ) ;
#53313 = ORIENTED_EDGE ( 'NONE', *, *, #64158, .T. ) ;
#53314 = DIRECTION ( 'NONE',  ( -4.274815082592931898E-19, -0.9999939076577903929, -0.003490651415223739937 ) ) ;
#53315 = CARTESIAN_POINT ( 'NONE',  ( -11.84999999999999787, 2.500000000000000000, -6.841600689897074261 ) ) ;
#53316 = DIRECTION ( 'NONE',  ( 0.000000000000000000, -0.9999939076577903929, 0.003490651415223739937 ) ) ;
#53317 = ORIENTED_EDGE ( 'NONE', *, *, #107023, .T. ) ;
#53318 = FACE_BOUND ( 'NONE', #94798, .T. ) ;
#53319 = FACE_OUTER_BOUND ( 'NONE', #106323, .T. ) ;
#53320 = DIRECTION ( 'NONE',  ( 0.000000000000000000, 0.000000000000000000, -1.000000000000000000 ) ) ;
#53321 = AXIS2_PLACEMENT_3D ( 'NONE', #102364, #63072, #45382 ) ;
#53322 = EDGE_CURVE ( 'NONE', #79354, #64399, #80088, .T. ) ;
#53323 = CARTESIAN_POINT ( 'NONE',  ( 5.649999999999934630, 2.500000000000000000, -2.511473670974877948 ) ) ;
#53324 = DIRECTION ( 'NONE',  ( -0.000000000000000000, 1.000000000000000000, -0.000000000000000000 ) ) ;
#53326 = EDGE_CURVE ( 'NONE', #124333, #103811, #50840, .T. ) ;
#53325 = CIRCLE ( 'NONE', #26125, 0.1000000000000000056 ) ;
#53327 = CARTESIAN_POINT ( 'NONE',  ( 13.94999999999989626, 2.500000000000000000, 2.611473670974873151 ) ) ;
#53328 = FACE_OUTER_BOUND ( 'NONE', #33357, .T. ) ;
#53329 = DIRECTION ( 'NONE',  ( -4.274815082592931898E-19, -0.9999939076577903929, -0.003490651415223739937 ) ) ;
#53330 = DIRECTION ( 'NONE',  ( -0.000000000000000000, -1.000000000000000000, -0.000000000000000000 ) ) ;
#53331 = CARTESIAN_POINT ( 'NONE',  ( -5.200000000000024158, 12.50000000000000000, -4.611443907251939756 ) ) ;
#53332 = ADVANCED_FACE ( 'NONE', ( #86697 ), #6187, .T. ) ;
#53333 = ORIENTED_EDGE ( 'NONE', *, *, #8213, .F. ) ;
#53334 = AXIS2_PLACEMENT_3D ( 'NONE', #42857, #4164, #121373 ) ;
#53335 = EDGE_LOOP ( 'NONE', ( #118263, #71263 ) ) ;
#53336 = ORIENTED_EDGE ( 'NONE', *, *, #51625, .F. ) ;
#53337 = EDGE_LOOP ( 'NONE', ( #35210, #69455 ) ) ;
#53338 = ORIENTED_EDGE ( 'NONE', *, *, #103488, .T. ) ;
#53339 = ORIENTED_EDGE ( 'NONE', *, *, #73652, .T. ) ;
#53340 = DIRECTION ( 'NONE',  ( -0.000000000000000000, -1.000000000000000000, -0.000000000000000000 ) ) ;
#53341 = ORIENTED_EDGE ( 'NONE', *, *, #45619, .T. ) ;
#53342 = VERTEX_POINT ( 'NONE', #14067 ) ;
#53343 = DIRECTION ( 'NONE',  ( -0.000000000000000000, 1.000000000000000000, -0.000000000000000000 ) ) ;
#53344 = DIRECTION ( 'NONE',  ( 0.000000000000000000, 1.000000000000000000, 0.000000000000000000 ) ) ;
#53345 = CARTESIAN_POINT ( 'NONE',  ( -4.150000000000025224, 2.500000000000000000, 6.395190528383296602 ) ) ;
#53346 = CIRCLE ( 'NONE', #86773, 0.1000000000000002554 ) ;
#53347 = ORIENTED_EDGE ( 'NONE', *, *, #123702, .T. ) ;
#53348 = DIRECTION ( 'NONE',  ( 0.000000000000000000, 1.000000000000000000, 0.000000000000000000 ) ) ;
#53349 = ORIENTED_EDGE ( 'NONE', *, *, #94325, .F. ) ;
#53351 = ORIENTED_EDGE ( 'NONE', *, *, #34956, .T. ) ;
#53350 = AXIS2_PLACEMENT_3D ( 'NONE', #109659, #101123, #31745 ) ;
#53352 = DIRECTION ( 'NONE',  ( 0.000000000000000000, -0.000000000000000000, 1.000000000000000000 ) ) ;
#53353 = AXIS2_PLACEMENT_3D ( 'NONE', #47222, #46554, #96299 ) ;
#53354 = CARTESIAN_POINT ( 'NONE',  ( -10.40000000000000213, 2.500000000000000000, -4.330127018922197202 ) ) ;
#53355 = ORIENTED_EDGE ( 'NONE', *, *, #69459, .F. ) ;
#53356 = EDGE_LOOP ( 'NONE', ( #27540, #23682 ) ) ;
#53357 = CARTESIAN_POINT ( 'NONE',  ( -9.350000000000004974, 12.50000000000000000, 6.906693963081109722 ) ) ;
#53358 = VECTOR ( 'NONE', #47571, 1000.000000000000000 ) ;
#53359 = VECTOR ( 'NONE', #86522, 1000.000000000000000 ) ;
#53360 = CARTESIAN_POINT ( 'NONE',  ( 8.549999999999918998, 2.500000000000000000, 6.941600689897073018 ) ) ;
#53361 = CARTESIAN_POINT ( 'NONE',  ( 179.5000000000000000, -0.6250000000000028866, -7.634788798650553154 ) ) ;
#53362 = CARTESIAN_POINT ( 'NONE',  ( 4.999999999999936939, 2.500000000000000000, -3.637306695894650055 ) ) ;
#53363 = AXIS2_PLACEMENT_3D ( 'NONE', #49549, #89459, #129418 ) ;
#53364 = DIRECTION ( 'NONE',  ( 0.000000000000000000, 1.000000000000000000, 0.000000000000000000 ) ) ;
#53365 = EDGE_CURVE ( 'NONE', #36522, #129616, #92607, .T. ) ;
#53366 = ORIENTED_EDGE ( 'NONE', *, *, #41575, .F. ) ;
#53367 = CARTESIAN_POINT ( 'NONE',  ( 15.62876697814516369, -2.500000000000000000, 5.624417669420343380 ) ) ;
#53368 = AXIS2_PLACEMENT_3D ( 'NONE', #41654, #30539, #70442 ) ;
#53369 = VECTOR ( 'NONE', #1617, 1000.000000000000000 ) ;
#53370 = EDGE_LOOP ( 'NONE', ( #104674, #127454 ) ) ;
#53371 = FACE_OUTER_BOUND ( 'NONE', #89401, .T. ) ;
#53372 = ORIENTED_EDGE ( 'NONE', *, *, #14086, .F. ) ;
#53373 = DIRECTION ( 'NONE',  ( 0.000000000000000000, 0.000000000000000000, 1.000000000000000000 ) ) ;
#53374 = DIRECTION ( 'NONE',  ( 0.000000000000000000, 1.000000000000000000, 0.000000000000000000 ) ) ;
#53375 = CIRCLE ( 'NONE', #74202, 0.06509327318403745899 ) ;
#53376 = EDGE_CURVE ( 'NONE', #121167, #94312, #6889, .T. ) ;
#53377 = CARTESIAN_POINT ( 'NONE',  ( 0.3999999999999563904, 2.500000000000000000, 3.737306695894644371 ) ) ;
#53378 = EDGE_CURVE ( 'NONE', #64213, #79919, #78024, .T. ) ;
#53379 = CARTESIAN_POINT ( 'NONE',  ( -0.6500000000000398792, 2.500000000000000000, -6.941600689897078347 ) ) ;
#53380 = EDGE_LOOP ( 'NONE', ( #21047, #52416 ) ) ;
#53381 = CARTESIAN_POINT ( 'NONE',  ( -7.500000000000013323, 12.50000000000000000, 5.088040615133786027 ) ) ;
#53382 = DIRECTION ( 'NONE',  ( 0.000000000000000000, 0.000000000000000000, -1.000000000000000000 ) ) ;
#53383 = EDGE_LOOP ( 'NONE', ( #116609, #116170, #59249, #31453 ) ) ;
#53384 = EDGE_LOOP ( 'NONE', ( #67782, #125109 ) ) ;
#53386 = ORIENTED_EDGE ( 'NONE', *, *, #35732, .T. ) ;
#53385 = EDGE_CURVE ( 'NONE', #43544, #106720, #8961, .T. ) ;
#53387 = CARTESIAN_POINT ( 'NONE',  ( 5.849999999999935696, 2.500000000000000000, -6.495190528383302464 ) ) ;
#53388 = CARTESIAN_POINT ( 'NONE',  ( 185.5260416670080588, -6.551208109652273848, -3.782341765625003571 ) ) ;
#53389 = AXIS2_PLACEMENT_3D ( 'NONE', #112071, #52492, #92418 ) ;
#53390 = DIRECTION ( 'NONE',  ( 0.000000000000000000, -0.9999939076577903929, 0.003490651415223739937 ) ) ;
#53391 = DIRECTION ( 'NONE',  ( -0.000000000000000000, 1.000000000000000000, -0.000000000000000000 ) ) ;
#53392 = CARTESIAN_POINT ( 'NONE',  ( 8.349999999999919709, 2.500000000000000000, 6.495190528383297135 ) ) ;
#53393 = DIRECTION ( 'NONE',  ( 0.000000000000000000, 0.000000000000000000, -1.000000000000000000 ) ) ;
#53394 = AXIS2_PLACEMENT_3D ( 'NONE', #110138, #32248, #40782 ) ;
#53395 = AXIS2_PLACEMENT_3D ( 'NONE', #24475, #61838, #72300 ) ;
#53396 = EDGE_LOOP ( 'NONE', ( #54612, #44983 ) ) ;
#53397 = AXIS2_PLACEMENT_3D ( 'NONE', #15431, #46858, #14771 ) ;
#53398 = FACE_OUTER_BOUND ( 'NONE', #66171, .T. ) ;
#53399 = EDGE_CURVE ( 'NONE', #119766, #88678, #44576, .T. ) ;
#53400 = ORIENTED_EDGE ( 'NONE', *, *, #93369, .F. ) ;
#53401 = CARTESIAN_POINT ( 'NONE',  ( 5.849999999999933920, 2.500000000000000000, 6.595190528383296780 ) ) ;
#53402 = DIRECTION ( 'NONE',  ( 0.000000000000000000, -0.000000000000000000, 1.000000000000000000 ) ) ;
#53403 = LINE ( 'NONE', #14730, #79833 ) ;
#53404 = DIRECTION ( 'NONE',  ( 0.000000000000000000, -0.000000000000000000, 1.000000000000000000 ) ) ;
#53405 = ORIENTED_EDGE ( 'NONE', *, *, #10823, .F. ) ;
#53406 = CIRCLE ( 'NONE', #26209, 0.1000000000000000472 ) ;
#53407 = EDGE_CURVE ( 'NONE', #101832, #92344, #67537, .T. ) ;
#53408 = AXIS2_PLACEMENT_3D ( 'NONE', #128843, #118339, #28682 ) ;
#53409 = CARTESIAN_POINT ( 'NONE',  ( -9.600000000000006750, 12.50000000000000000, 0.7579135962115869374 ) ) ;
#53411 = VERTEX_POINT ( 'NONE', #76883 ) ;
#53410 = LINE ( 'NONE', #100560, #58849 ) ;
#53412 = EDGE_CURVE ( 'NONE', #104601, #32860, #125337, .T. ) ;
#53413 = ADVANCED_FACE ( 'NONE', ( #24555 ), #117708, .T. ) ;
#53414 = EDGE_CURVE ( 'NONE', #12173, #87251, #38328, .T. ) ;
#53415 = EDGE_CURVE ( 'NONE', #19409, #15503, #13154, .T. ) ;
#53416 = EDGE_LOOP ( 'NONE', ( #58798, #46727 ) ) ;
#53417 = DIRECTION ( 'NONE',  ( 0.000000000000000000, 0.000000000000000000, 1.000000000000000000 ) ) ;
#53418 = AXIS2_PLACEMENT_3D ( 'NONE', #125250, #15921, #65672 ) ;
#53419 = AXIS2_PLACEMENT_3D ( 'NONE', #16584, #4186, #114797 ) ;
#53420 = ORIENTED_EDGE ( 'NONE', *, *, #52214, .T. ) ;
#53421 = ORIENTED_EDGE ( 'NONE', *, *, #46588, .F. ) ;
#53422 = CARTESIAN_POINT ( 'NONE',  ( 10.39999999999990976, 2.500000000000000000, 4.430127018922196847 ) ) ;
#53423 = EDGE_CURVE ( 'NONE', #112989, #73598, #107265, .T. ) ;
#53424 = EDGE_CURVE ( 'NONE', #16575, #87037, #647, .T. ) ;
#53425 = VERTEX_POINT ( 'NONE', #9432 ) ;
#53426 = CARTESIAN_POINT ( 'NONE',  ( 17.88933034088960028, 0.4802206367767866690, -4.999988745079795294 ) ) ;
#53427 = CARTESIAN_POINT ( 'NONE',  ( -5.000000000000024869, 2.500000000000000000, -4.922947341949753586 ) ) ;
#53428 = DIRECTION ( 'NONE',  ( -0.000000000000000000, -1.000000000000000000, -0.000000000000000000 ) ) ;
#53429 = EDGE_LOOP ( 'NONE', ( #38755, #24337, #123514, #24574 ) ) ;
#53430 = EDGE_CURVE ( 'NONE', #58340, #52125, #15309, .T. ) ;
#53431 = AXIS2_PLACEMENT_3D ( 'NONE', #120307, #79732, #30648 ) ;
#53432 = DIRECTION ( 'NONE',  ( -0.000000000000000000, -1.000000000000000000, -0.000000000000000000 ) ) ;
#53434 = ORIENTED_EDGE ( 'NONE', *, *, #32619, .F. ) ;
#53433 = CARTESIAN_POINT ( 'NONE',  ( 187.5000000000000000, 0.000000000000000000, 7.700000000000000178 ) ) ;
#53435 = CARTESIAN_POINT ( 'NONE',  ( 17.45053073489854967, 1.969617801099436738, 4.507369966539876316 ) ) ;
#53436 = EDGE_CURVE ( 'NONE', #42825, #120364, #10075, .T. ) ;
#53437 = DIRECTION ( 'NONE',  ( -0.000000000000000000, 1.000000000000000000, -0.000000000000000000 ) ) ;
#53438 = CIRCLE ( 'NONE', #70160, 0.1000000000000002554 ) ;
#53439 = EDGE_CURVE ( 'NONE', #17385, #47052, #61309, .T. ) ;
#53440 = ORIENTED_EDGE ( 'NONE', *, *, #97279, .F. ) ;
#53441 = CIRCLE ( 'NONE', #74355, 0.09999999999999982514 ) ;
#53442 = EDGE_LOOP ( 'NONE', ( #99366, #32130, #17332, #117815 ) ) ;
#53443 = VECTOR ( 'NONE', #95736, 1000.000000000000000 ) ;
#53444 = ORIENTED_EDGE ( 'NONE', *, *, #119902, .T. ) ;
#53445 = VERTEX_POINT ( 'NONE', #238 ) ;
#53446 = FACE_OUTER_BOUND ( 'NONE', #126495, .T. ) ;
#53447 = CARTESIAN_POINT ( 'NONE',  ( 12.09999999999990195, 2.500000000000000000, 0.6928203230275494784 ) ) ;
#53448 = DIRECTION ( 'NONE',  ( -0.000000000000000000, 1.000000000000000000, -0.000000000000000000 ) ) ;
#53449 = FACE_BOUND ( 'NONE', #27628, .T. ) ;
#53450 = EDGE_LOOP ( 'NONE', ( #3697, #96545, #54493, #115342 ) ) ;
#53451 = CARTESIAN_POINT ( 'NONE',  ( 185.4479166673494603, -6.668395609140176816, -3.850000000000003642 ) ) ;
#53452 = CARTESIAN_POINT ( 'NONE',  ( -6.650000000000018119, 2.500000000000000000, -2.165063509461101710 ) ) ;
#53453 = DIRECTION ( 'NONE',  ( 0.000000000000000000, 1.000000000000000000, 0.000000000000000000 ) ) ;
#53454 = CIRCLE ( 'NONE', #88951, 0.06509327318403745899 ) ;
#53455 = CARTESIAN_POINT ( 'NONE',  ( 1.899999999999951283, 12.50000000000000000, -4.741630453620015118 ) ) ;
#53456 = DIRECTION ( 'NONE',  ( 0.000000000000000000, 0.000000000000000000, 1.000000000000000000 ) ) ;
#53457 = LINE ( 'NONE', #93373, #65901 ) ;
#53458 = VECTOR ( 'NONE', #11363, 1000.000000000000000 ) ;
#53459 = AXIS2_PLACEMENT_3D ( 'NONE', #97099, #87264, #37547 ) ;
#53460 = DIRECTION ( 'NONE',  ( 0.000000000000000000, 0.000000000000000000, 1.000000000000000000 ) ) ;
#53461 = VECTOR ( 'NONE', #80066, 1000.000000000000000 ) ;
#53462 = ORIENTED_EDGE ( 'NONE', *, *, #61669, .T. ) ;
#53463 = EDGE_LOOP ( 'NONE', ( #43492, #95357, #110868, #100899 ) ) ;
#53464 = ORIENTED_EDGE ( 'NONE', *, *, #117787, .F. ) ;
#53465 = EDGE_LOOP ( 'NONE', ( #71405, #67303 ) ) ;
#53466 = AXIS2_PLACEMENT_3D ( 'NONE', #113268, #34078, #94268 ) ;
#53467 = VERTEX_POINT ( 'NONE', #48076 ) ;
#53468 = DIRECTION ( 'NONE',  ( 0.000000000000000000, 1.000000000000000000, 0.000000000000000000 ) ) ;
#53469 = DIRECTION ( 'NONE',  ( 0.000000000000000000, 0.000000000000000000, 1.000000000000000000 ) ) ;
#53470 = VERTEX_POINT ( 'NONE', #118733 ) ;
#53471 = FACE_BOUND ( 'NONE', #107439, .T. ) ;
#53472 = DIRECTION ( 'NONE',  ( -0.000000000000000000, -1.000000000000000000, -0.000000000000000000 ) ) ;
#53473 = EDGE_CURVE ( 'NONE', #9353, #127509, #67691, .T. ) ;
#53474 = ADVANCED_FACE ( 'NONE', ( #97802 ), #57089, .T. ) ;
#53475 = ORIENTED_EDGE ( 'NONE', *, *, #85880, .T. ) ;
#53476 = LINE ( 'NONE', #25269, #124764 ) ;
#53477 = DIRECTION ( 'NONE',  ( 0.000000000000000000, 0.000000000000000000, -1.000000000000000000 ) ) ;
#53478 = DIRECTION ( 'NONE',  ( 0.000000000000000000, -0.9999939076577903929, 0.003490651415223739937 ) ) ;
#53480 = ORIENTED_EDGE ( 'NONE', *, *, #127488, .F. ) ;
#53479 = VECTOR ( 'NONE', #71325, 1000.000000000000000 ) ;
#53481 = FACE_OUTER_BOUND ( 'NONE', #48879, .T. ) ;
#53482 = ORIENTED_EDGE ( 'NONE', *, *, #103551, .T. ) ;
#53483 = EDGE_LOOP ( 'NONE', ( #5529, #82362, #65578, #124827 ) ) ;
#53484 = ORIENTED_EDGE ( 'NONE', *, *, #60044, .F. ) ;
#53485 = DIRECTION ( 'NONE',  ( 0.000000000000000000, 0.000000000000000000, 1.000000000000000000 ) ) ;
#53486 = DIRECTION ( 'NONE',  ( 0.000000000000000000, 1.000000000000000000, 0.000000000000000000 ) ) ;
#53487 = CIRCLE ( 'NONE', #34724, 0.06509327318403741736 ) ;
#53488 = CARTESIAN_POINT ( 'NONE',  ( -15.59999999999998010, 2.500000000000000000, 0.3464101615137759604 ) ) ;
#53489 = ORIENTED_EDGE ( 'NONE', *, *, #5778, .F. ) ;
#53490 = DIRECTION ( 'NONE',  ( -4.274815082592931898E-19, -0.9999939076577903929, -0.003490651415223739937 ) ) ;
#53491 = AXIS2_PLACEMENT_3D ( 'NONE', #105620, #76159, #25113 ) ;
#53492 = LINE ( 'NONE', #15475, #76246 ) ;
#53493 = VECTOR ( 'NONE', #42220, 1000.000000000000000 ) ;
#53494 = DIRECTION ( 'NONE',  ( -0.000000000000000000, -1.000000000000000000, -0.000000000000000000 ) ) ;
#53495 = CARTESIAN_POINT ( 'NONE',  ( 187.1562500006828316, 8.891194145520236347, 5.444286225454521982E-16 ) ) ;
#53496 = ORIENTED_EDGE ( 'NONE', *, *, #32013, .T. ) ;
#53497 = LINE ( 'NONE', #122879, #101818 ) ;
#53498 = VERTEX_POINT ( 'NONE', #67032 ) ;
#53499 = CARTESIAN_POINT ( 'NONE',  ( -6.450000000000016165, 2.500000000000000000, 6.741600689897071952 ) ) ;
#53500 = VECTOR ( 'NONE', #49744, 1000.000000000000000 ) ;
#53501 = ORIENTED_EDGE ( 'NONE', *, *, #16341, .T. ) ;
#53503 = AXIS2_PLACEMENT_3D ( 'NONE', #110776, #7577, #88049 ) ;
#53502 = CONICAL_SURFACE ( 'NONE', #13767, 0.1000000000000000472, 0.003490658503988666988 ) ;
#53504 = ORIENTED_EDGE ( 'NONE', *, *, #59365, .F. ) ;
#53505 = DIRECTION ( 'NONE',  ( 0.000000000000000000, -0.000000000000000000, -1.000000000000000000 ) ) ;
#53506 = CARTESIAN_POINT ( 'NONE',  ( -10.20000000000000462, 2.500000000000000000, -4.676537180435973440 ) ) ;
#53507 = DIRECTION ( 'NONE',  ( -0.000000000000000000, -1.000000000000000000, -0.000000000000000000 ) ) ;
#53508 = DIRECTION ( 'NONE',  ( 0.000000000000000000, -0.000000000000000000, 1.000000000000000000 ) ) ;
#53509 = CARTESIAN_POINT ( 'NONE',  ( 9.399999999999915090, 2.500000000000000000, -4.083716857408426826 ) ) ;
#53510 = VERTEX_POINT ( 'NONE', #8127 ) ;
#53511 = ORIENTED_EDGE ( 'NONE', *, *, #55964, .T. ) ;
#53512 = EDGE_CURVE ( 'NONE', #64031, #91293, #86324, .T. ) ;
#53513 = DIRECTION ( 'NONE',  ( -0.000000000000000000, -1.000000000000000000, -0.000000000000000000 ) ) ;
#53514 = CIRCLE ( 'NONE', #57428, 0.5000000000000004441 ) ;
#53515 = AXIS2_PLACEMENT_3D ( 'NONE', #51248, #22431, #91150 ) ;
#53516 = FACE_OUTER_BOUND ( 'NONE', #76318, .T. ) ;
#53517 = DIRECTION ( 'NONE',  ( 0.000000000000000000, 0.000000000000000000, 1.000000000000000000 ) ) ;
#53518 = VERTEX_POINT ( 'NONE', #47430 ) ;
#53519 = ORIENTED_EDGE ( 'NONE', *, *, #52955, .T. ) ;
#53520 = DIRECTION ( 'NONE',  ( 0.000000000000000000, 1.000000000000000000, 0.000000000000000000 ) ) ;
#53521 = ORIENTED_EDGE ( 'NONE', *, *, #104362, .T. ) ;
#53522 = EDGE_CURVE ( 'NONE', #48111, #4340, #15211, .T. ) ;
#53523 = CARTESIAN_POINT ( 'NONE',  ( -4.800000000000026468, 2.500000000000000000, -4.676537180435978769 ) ) ;
#53524 = DIRECTION ( 'NONE',  ( 0.000000000000000000, 1.000000000000000000, 0.000000000000000000 ) ) ;
#53525 = ORIENTED_EDGE ( 'NONE', *, *, #28119, .T. ) ;
#53526 = CARTESIAN_POINT ( 'NONE',  ( -6.050000000000022027, 2.500000000000000000, -1.818653347947326138 ) ) ;
#53527 = CARTESIAN_POINT ( 'NONE',  ( -11.24999999999999822, 2.500000000000000000, 1.372243186433545370 ) ) ;
#53528 = CARTESIAN_POINT ( 'NONE',  ( -9.150000000000009237, 2.500000000000000000, 1.372243186433545370 ) ) ;
#53529 = CARTESIAN_POINT ( 'NONE',  ( -7.100000000000018296, 2.500000000000000000, -4.330127018922201643 ) ) ;
#53530 = EDGE_CURVE ( 'NONE', #124307, #129616, #87326, .T. ) ;
#53531 = EDGE_CURVE ( 'NONE', #58192, #105776, #48791, .T. ) ;
#53532 = CARTESIAN_POINT ( 'NONE',  ( -13.34999999999999076, 2.500000000000000000, 2.265063509461101354 ) ) ;
#53533 = ORIENTED_EDGE ( 'NONE', *, *, #77370, .F. ) ;
#53534 = DIRECTION ( 'NONE',  ( 0.000000000000000000, 0.000000000000000000, -1.000000000000000000 ) ) ;
#53535 = VECTOR ( 'NONE', #106036, 1000.000000000000000 ) ;
#53536 = CARTESIAN_POINT ( 'NONE',  ( 76.45227062015452191, -3.905198618276467304, 5.870121734768856570 ) ) ;
#53537 = ORIENTED_EDGE ( 'NONE', *, *, #61888, .F. ) ;
#53538 = ORIENTED_EDGE ( 'NONE', *, *, #41781, .T. ) ;
#53539 = EDGE_CURVE ( 'NONE', #180, #45027, #105213, .T. ) ;
#53540 = CARTESIAN_POINT ( 'NONE',  ( 186.4635416670080872, -4.367472073101519747, 7.564683531249999149 ) ) ;
#53541 = CARTESIAN_POINT ( 'NONE',  ( 195.0435778713738557, 0.000000000000000000, -8.040022453829767102 ) ) ;
#53542 = DIRECTION ( 'NONE',  ( -0.000000000000000000, -1.000000000000000000, -0.000000000000000000 ) ) ;
#53543 = CARTESIAN_POINT ( 'NONE',  ( -2.900000000000029221, 2.500000000000000000, -4.430127018922202176 ) ) ;
#53544 = CARTESIAN_POINT ( 'NONE',  ( -3.950000000000026379, 12.50000000000000000, -1.818653347947326138 ) ) ;
#53545 = CARTESIAN_POINT ( 'NONE',  ( -9.400000000000007461, 2.500000000000000000, 4.576537180435972019 ) ) ;
#53546 = LINE ( 'NONE', #4400, #128303 ) ;
#53547 = CARTESIAN_POINT ( 'NONE',  ( -7.950000000000009059, 2.500000000000000000, 6.495190528383297135 ) ) ;
#53548 = LINE ( 'NONE', #93466, #72891 ) ;
#53549 = CARTESIAN_POINT ( 'NONE',  ( -12.49999999999995914, 2.500000000000000000, -0.09999999999999815981 ) ) ;
#53550 = CARTESIAN_POINT ( 'NONE',  ( 1.649999999999951950, 12.50000000000000000, -5.867463478539787225 ) ) ;
#53551 = CONICAL_SURFACE ( 'NONE', #78694, 0.1000000000000002554, 0.003490658503988666988 ) ;
#53552 = EDGE_LOOP ( 'NONE', ( #94915, #112954 ) ) ;
#53553 = VERTEX_POINT ( 'NONE', #77517 ) ;
#53554 = ORIENTED_EDGE ( 'NONE', *, *, #97906, .T. ) ;
#53555 = ORIENTED_EDGE ( 'NONE', *, *, #58245, .T. ) ;
#53556 = DIRECTION ( 'NONE',  ( 0.000000000000000000, 0.000000000000000000, 1.000000000000000000 ) ) ;
#53557 = FACE_OUTER_BOUND ( 'NONE', #68988, .T. ) ;
#53558 = EDGE_LOOP ( 'NONE', ( #39508, #78223 ) ) ;
#53559 = DIRECTION ( 'NONE',  ( -0.000000000000000000, 1.000000000000000000, -0.000000000000000000 ) ) ;
#53560 = EDGE_CURVE ( 'NONE', #103587, #127196, #128306, .T. ) ;
#53561 = DIRECTION ( 'NONE',  ( 0.000000000000000000, 0.000000000000000000, 1.000000000000000000 ) ) ;
#53563 = ORIENTED_EDGE ( 'NONE', *, *, #18573, .F. ) ;
#53562 = CARTESIAN_POINT ( 'NONE',  ( 13.29999999999989946, 2.500000000000000000, -2.385244779468109755E-15 ) ) ;
#53564 = EDGE_CURVE ( 'NONE', #64904, #98829, #23754, .T. ) ;
#53565 = FACE_OUTER_BOUND ( 'NONE', #57340, .T. ) ;
#53566 = ADVANCED_FACE ( 'NONE', ( #128587 ), #113622, .T. ) ;
#53567 = CARTESIAN_POINT ( 'NONE',  ( -2.700000000000030376, 2.500000000000000000, 3.883716857408421319 ) ) ;
#53568 = ORIENTED_EDGE ( 'NONE', *, *, #32863, .T. ) ;
#53569 = AXIS2_PLACEMENT_3D ( 'NONE', #47420, #86685, #35661 ) ;
#53570 = VERTEX_POINT ( 'NONE', #118083 ) ;
#53571 = ORIENTED_EDGE ( 'NONE', *, *, #112271, .F. ) ;
#53572 = ORIENTED_EDGE ( 'NONE', *, *, #30550, .T. ) ;
#53573 = PLANE ( 'NONE',  #46831 ) ;
#53574 = ADVANCED_FACE ( 'NONE', ( #19228 ), #68344, .T. ) ;
#53575 = EDGE_CURVE ( 'NONE', #71342, #45854, #111564, .T. ) ;
#53576 = CONICAL_SURFACE ( 'NONE', #87014, 0.1000000000000002554, 0.003490658503988666988 ) ;
#53577 = EDGE_CURVE ( 'NONE', #125197, #41184, #69635, .T. ) ;
#53578 = VECTOR ( 'NONE', #115237, 1000.000000000000000 ) ;
#53579 = EDGE_CURVE ( 'NONE', #31468, #94085, #53231, .T. ) ;
#53580 = FACE_OUTER_BOUND ( 'NONE', #24090, .T. ) ;
#53581 = DIRECTION ( 'NONE',  ( 0.000000000000000000, 0.000000000000000000, 1.000000000000000000 ) ) ;
#53582 = VECTOR ( 'NONE', #32874, 1000.000000000000000 ) ;
#53583 = CARTESIAN_POINT ( 'NONE',  ( 13.74999999999989519, 2.500000000000000000, -2.757883832488654097 ) ) ;
#53584 = VERTEX_POINT ( 'NONE', #72863 ) ;
#53585 = AXIS2_PLACEMENT_3D ( 'NONE', #92912, #53617, #52325 ) ;
#53586 = EDGE_CURVE ( 'NONE', #21808, #37517, #120033, .T. ) ;
#53587 = FACE_OUTER_BOUND ( 'NONE', #128623, .T. ) ;
#53588 = ORIENTED_EDGE ( 'NONE', *, *, #61524, .T. ) ;
#53589 = CARTESIAN_POINT ( 'NONE',  ( 4.799999999999934097, 2.500000000000000000, 4.576537180435972019 ) ) ;
#53590 = DIRECTION ( 'NONE',  ( 0.000000000000000000, 0.000000000000000000, -1.000000000000000000 ) ) ;
#53591 = LINE ( 'NONE', #113139, #21220 ) ;
#53592 = CARTESIAN_POINT ( 'NONE',  ( -8.350000000000008527, 12.50000000000000000, 7.188010851410848723 ) ) ;
#53593 = ADVANCED_FACE ( 'NONE', ( #70289 ), #86418, .T. ) ;
#53594 = CIRCLE ( 'NONE', #49401, 0.1000000000000002554 ) ;
#53595 = EDGE_LOOP ( 'NONE', ( #100160, #80928 ) ) ;
#53597 = CIRCLE ( 'NONE', #70318, 0.06509327318403741736 ) ;
#53596 = AXIS2_PLACEMENT_3D ( 'NONE', #118371, #39841, #120318 ) ;
#53598 = VERTEX_POINT ( 'NONE', #110212 ) ;
#53599 = VERTEX_POINT ( 'NONE', #40849 ) ;
#53600 = DIRECTION ( 'NONE',  ( 0.000000000000000000, 0.000000000000000000, -1.000000000000000000 ) ) ;
#53601 = CARTESIAN_POINT ( 'NONE',  ( 6.249999999999968914, 2.500000000000000000, -6.395190528383301931 ) ) ;
#53602 = CARTESIAN_POINT ( 'NONE',  ( -11.25000000000000000, 2.500000000000000000, -7.288010851410851032 ) ) ;
#53603 = FACE_BOUND ( 'NONE', #87073, .T. ) ;
#53604 = CARTESIAN_POINT ( 'NONE',  ( -7.700000000000014388, 2.500000000000000000, -0.4464101615137782142 ) ) ;
#53605 = CARTESIAN_POINT ( 'NONE',  ( -14.99999999999998224, 2.500000000000000000, -0.5928203230275518321 ) ) ;
#53606 = FACE_OUTER_BOUND ( 'NONE', #60508, .T. ) ;
#53607 = CARTESIAN_POINT ( 'NONE',  ( 187.5000000000000000, 0.000000000000000000, 0.000000000000000000 ) ) ;
#53608 = FACE_OUTER_BOUND ( 'NONE', #81380, .T. ) ;
#53609 = CARTESIAN_POINT ( 'NONE',  ( -4.119968255444916849E-14, 2.500000000000000000, 3.637306695894644726 ) ) ;
#53610 = ORIENTED_EDGE ( 'NONE', *, *, #75697, .T. ) ;
#53611 = CARTESIAN_POINT ( 'NONE',  ( 10.84999999999991260, 12.50000000000000000, -2.165063509461101710 ) ) ;
#53612 = VERTEX_POINT ( 'NONE', #101681 ) ;
#53613 = VERTEX_POINT ( 'NONE', #52569 ) ;
#53614 = EDGE_LOOP ( 'NONE', ( #97702, #5933, #85277, #53538 ) ) ;
#53615 = FACE_OUTER_BOUND ( 'NONE', #65758, .T. ) ;
#53616 = FACE_BOUND ( 'NONE', #58344, .T. ) ;
#53617 = DIRECTION ( 'NONE',  ( -0.000000000000000000, -1.000000000000000000, -0.000000000000000000 ) ) ;
#53618 = AXIS2_PLACEMENT_3D ( 'NONE', #113201, #63476, #113866 ) ;
#53619 = EDGE_CURVE ( 'NONE', #6735, #37234, #115669, .T. ) ;
#53620 = ORIENTED_EDGE ( 'NONE', *, *, #121353, .T. ) ;
#53621 = CARTESIAN_POINT ( 'NONE',  ( -4.400000000000025224, 12.50000000000000000, 4.676537180435972552 ) ) ;
#53622 = DIRECTION ( 'NONE',  ( 0.000000000000000000, 0.000000000000000000, -1.000000000000000000 ) ) ;
#53623 = VERTEX_POINT ( 'NONE', #61104 ) ;
#53624 = PLANE ( 'NONE',  #122234 ) ;
#53625 = FACE_OUTER_BOUND ( 'NONE', #124961, .T. ) ;
#53626 = AXIS2_PLACEMENT_3D ( 'NONE', #122199, #32545, #16075 ) ;
#53627 = EDGE_CURVE ( 'NONE', #52693, #12173, #91213, .T. ) ;
#53628 = VERTEX_POINT ( 'NONE', #80107 ) ;
#53629 = PLANE ( 'NONE',  #15086 ) ;
#53630 = CARTESIAN_POINT ( 'NONE',  ( 12.09999999999990195, 2.500000000000000000, -2.276824562219559311E-15 ) ) ;
#53632 = CIRCLE ( 'NONE', #120535, 0.1000000000000002554 ) ;
#53631 = AXIS2_PLACEMENT_3D ( 'NONE', #121796, #92335, #2655 ) ;
#53633 = ORIENTED_EDGE ( 'NONE', *, *, #51274, .T. ) ;
#53634 = AXIS2_PLACEMENT_3D ( 'NONE', #95535, #5836, #85055 ) ;
#53635 = DIRECTION ( 'NONE',  ( 0.000000000000000000, 0.000000000000000000, 1.000000000000000000 ) ) ;
#53636 = FACE_OUTER_BOUND ( 'NONE', #57500, .T. ) ;
#53637 = CARTESIAN_POINT ( 'NONE',  ( -10.20000000000000284, 2.500000000000000000, -0.2464101615137782308 ) ) ;
#53638 = ORIENTED_EDGE ( 'NONE', *, *, #48818, .T. ) ;
#53639 = ORIENTED_EDGE ( 'NONE', *, *, #102197, .T. ) ;
#53640 = LINE ( 'NONE', #4500, #78633 ) ;
#53641 = ORIENTED_EDGE ( 'NONE', *, *, #8188, .T. ) ;
#53642 = DIRECTION ( 'NONE',  ( 0.000000000000000000, 1.000000000000000000, 0.000000000000000000 ) ) ;
#53643 = CARTESIAN_POINT ( 'NONE',  ( -9.600000000000006750, 2.500000000000000000, -0.5928203230275542746 ) ) ;
#53644 = ORIENTED_EDGE ( 'NONE', *, *, #107250, .F. ) ;
#53645 = DIRECTION ( 'NONE',  ( 0.000000000000000000, 0.000000000000000000, -1.000000000000000000 ) ) ;
#53646 = CARTESIAN_POINT ( 'NONE',  ( 9.799999999999915445, 2.500000000000000000, 3.983716857408420964 ) ) ;
#53647 = CARTESIAN_POINT ( 'NONE',  ( 4.399999999999940847, 12.50000000000000000, -4.048810130592463530 ) ) ;
#53648 = CARTESIAN_POINT ( 'NONE',  ( 4.149999999999941735, 2.500000000000000000, -1.572243186433550211 ) ) ;
#53649 = AXIS2_PLACEMENT_3D ( 'NONE', #343, #97271, #109007 ) ;
#53650 = CARTESIAN_POINT ( 'NONE',  ( 9.549999999999918998, 2.500000000000000000, -6.495190528383302464 ) ) ;
#53651 = VECTOR ( 'NONE', #59125, 1000.000000000000000 ) ;
#53652 = ORIENTED_EDGE ( 'NONE', *, *, #13826, .T. ) ;
#53654 = VERTEX_POINT ( 'NONE', #82025 ) ;
#53653 = EDGE_CURVE ( 'NONE', #105928, #124471, #51942, .T. ) ;
#53655 = CARTESIAN_POINT ( 'NONE',  ( -1.250000000000037526, 2.500000000000000000, -1.472243186433550122 ) ) ;
#53656 = AXIS2_PLACEMENT_3D ( 'NONE', #128636, #78881, #118781 ) ;
#53657 = CARTESIAN_POINT ( 'NONE',  ( 108.0000000000000142, 5.855766388782936538, -5.000000000000004441 ) ) ;
#53659 = EDGE_LOOP ( 'NONE', ( #113319, #29613, #4079, #87712 ) ) ;
#53658 = VERTEX_POINT ( 'NONE', #2174 ) ;
#53660 = ORIENTED_EDGE ( 'NONE', *, *, #96276, .F. ) ;
#53661 = CARTESIAN_POINT ( 'NONE',  ( 13.14999999999990088, 2.500000000000000000, 1.918653347947321564 ) ) ;
#53662 = AXIS2_PLACEMENT_3D ( 'NONE', #43031, #82936, #33201 ) ;
#53663 = AXIS2_PLACEMENT_3D ( 'NONE', #1141, #69890, #48310 ) ;
#53665 = ADVANCED_FACE ( 'NONE', ( #12636 ), #30377, .T. ) ;
#53664 = FACE_OUTER_BOUND ( 'NONE', #64438, .T. ) ;
#53666 = DIRECTION ( 'NONE',  ( 0.000000000000000000, 0.000000000000000000, -1.000000000000000000 ) ) ;
#53667 = AXIS2_PLACEMENT_3D ( 'NONE', #89142, #30891, #2041 ) ;
#53668 = DIRECTION ( 'NONE',  ( 0.000000000000000000, -0.9999939076577903929, 0.003490651415223739937 ) ) ;
#53669 = DIRECTION ( 'NONE',  ( 0.000000000000000000, 0.000000000000000000, 1.000000000000000000 ) ) ;
#53670 = DIRECTION ( 'NONE',  ( -0.000000000000000000, 1.000000000000000000, -0.000000000000000000 ) ) ;
#53671 = DIRECTION ( 'NONE',  ( 0.000000000000000000, 0.000000000000000000, -1.000000000000000000 ) ) ;
#53672 = CARTESIAN_POINT ( 'NONE',  ( 2.499999999999983569, 12.50000000000000000, -4.330127018922201643 ) ) ;
#53673 = EDGE_CURVE ( 'NONE', #104031, #126341, #1530, .T. ) ;
#53674 = EDGE_CURVE ( 'NONE', #106262, #115994, #100389, .T. ) ;
#53675 = CARTESIAN_POINT ( 'NONE',  ( 9.199999999999919353, 12.50000000000000000, -2.276824562219559311E-15 ) ) ;
#53676 = VECTOR ( 'NONE', #7379, 1000.000000000000000 ) ;
#53677 = VERTEX_POINT ( 'NONE', #72233 ) ;
#53679 = AXIS2_PLACEMENT_3D ( 'NONE', #102102, #32737, #3258 ) ;
#53678 = AXIS2_PLACEMENT_3D ( 'NONE', #90035, #120162, #40323 ) ;
#53680 = EDGE_CURVE ( 'NONE', #129536, #125867, #2812, .T. ) ;
#53681 = PLANE ( 'NONE',  #50708 ) ;
#53682 = ORIENTED_EDGE ( 'NONE', *, *, #123572, .F. ) ;
#53683 = VERTEX_POINT ( 'NONE', #23111 ) ;
#53684 = ADVANCED_FACE ( 'NONE', ( #71562 ), #30014, .T. ) ;
#53685 = DIRECTION ( 'NONE',  ( 0.000000000000000000, 0.000000000000000000, -1.000000000000000000 ) ) ;
#53686 = DIRECTION ( 'NONE',  ( 0.000000000000000000, 0.000000000000000000, 1.000000000000000000 ) ) ;
#53687 = FACE_OUTER_BOUND ( 'NONE', #17253, .T. ) ;
#53688 = DIRECTION ( 'NONE',  ( 0.000000000000000000, 0.000000000000000000, -1.000000000000000000 ) ) ;
#53689 = DIRECTION ( 'NONE',  ( 0.000000000000000000, 0.000000000000000000, 1.000000000000000000 ) ) ;
#53690 = FACE_OUTER_BOUND ( 'NONE', #106579, .T. ) ;
#53691 = DIRECTION ( 'NONE',  ( -0.000000000000000000, 1.000000000000000000, -0.000000000000000000 ) ) ;
#53692 = VERTEX_POINT ( 'NONE', #122611 ) ;
#53693 = DIRECTION ( 'NONE',  ( 0.000000000000000000, 0.000000000000000000, -1.000000000000000000 ) ) ;
#53694 = TOROIDAL_SURFACE ( 'NONE', #49600, 9.000000000000001776, 1.000000000000000000 ) ;
#53695 = CARTESIAN_POINT ( 'NONE',  ( 11.64999999999990798, 2.500000000000000000, -1.572243186433550211 ) ) ;
#53696 = VERTEX_POINT ( 'NONE', #32960 ) ;
#53697 = ORIENTED_EDGE ( 'NONE', *, *, #39254, .F. ) ;
#53698 = ORIENTED_EDGE ( 'NONE', *, *, #26339, .F. ) ;
#53699 = ORIENTED_EDGE ( 'NONE', *, *, #71457, .T. ) ;
#53700 = DIRECTION ( 'NONE',  ( 0.000000000000000000, -0.9999939076577903929, 0.003490651415223739937 ) ) ;
#53701 = CARTESIAN_POINT ( 'NONE',  ( -4.800000000000024691, 12.50000000000000000, 0.3464101615137735735 ) ) ;
#53702 = CARTESIAN_POINT ( 'NONE',  ( 1.449999999999952216, 2.500000000000000000, -2.511473670974877948 ) ) ;
#53704 = CARTESIAN_POINT ( 'NONE',  ( -1.050000000000038236, 2.500000000000000000, -1.718653347947326049 ) ) ;
#53703 = AXIS2_PLACEMENT_3D ( 'NONE', #50051, #39590, #89299 ) ;
#53705 = FACE_OUTER_BOUND ( 'NONE', #82470, .T. ) ;
#53706 = ORIENTED_EDGE ( 'NONE', *, *, #34811, .T. ) ;
#53707 = FACE_OUTER_BOUND ( 'NONE', #27751, .T. ) ;
#53708 = CARTESIAN_POINT ( 'NONE',  ( 9.999999999999948486, 12.50000000000000000, -4.265033745738164406 ) ) ;
#53709 = LINE ( 'NONE', #33448, #13793 ) ;
#53711 = AXIS2_PLACEMENT_3D ( 'NONE', #43123, #122313, #31357 ) ;
#53710 = CIRCLE ( 'NONE', #1474, 0.06509327318403745899 ) ;
#53712 = CARTESIAN_POINT ( 'NONE',  ( -11.64999999999999680, 2.500000000000000000, 2.857883832488649301 ) ) ;
#53713 = ORIENTED_EDGE ( 'NONE', *, *, #68521, .F. ) ;
#53714 = ORIENTED_EDGE ( 'NONE', *, *, #46480, .T. ) ;
#53715 = ORIENTED_EDGE ( 'NONE', *, *, #3332, .F. ) ;
#53716 = ADVANCED_FACE ( 'NONE', ( #112792 ), #69708, .T. ) ;
#53717 = DIRECTION ( 'NONE',  ( 0.000000000000000000, 0.000000000000000000, 1.000000000000000000 ) ) ;
#53718 = ADVANCED_FACE ( 'NONE', ( #70928 ), #41496, .T. ) ;
#53719 = EDGE_CURVE ( 'NONE', #18217, #112183, #9064, .T. ) ;
#53722 = ADVANCED_FACE ( 'NONE', ( #26347 ), #117802, .T. ) ;
#53721 = CIRCLE ( 'NONE', #28601, 0.1000000000000000472 ) ;
#53720 = AXIS2_PLACEMENT_3D ( 'NONE', #59377, #48239, #117591 ) ;
#53723 = FACE_OUTER_BOUND ( 'NONE', #53483, .T. ) ;
#53724 = DIRECTION ( 'NONE',  ( 0.000000000000000000, 0.000000000000000000, 1.000000000000000000 ) ) ;
#53725 = AXIS2_PLACEMENT_3D ( 'NONE', #71651, #72309, #11439 ) ;
#53726 = ADVANCED_FACE ( 'NONE', ( #4735 ), #55796, .T. ) ;
#53727 = ORIENTED_EDGE ( 'NONE', *, *, #70434, .F. ) ;
#53728 = DIRECTION ( 'NONE',  ( 0.000000000000000000, 0.000000000000000000, -1.000000000000000000 ) ) ;
#53729 = DIRECTION ( 'NONE',  ( 0.000000000000000000, 0.000000000000000000, 1.000000000000000000 ) ) ;
#53730 = CARTESIAN_POINT ( 'NONE',  ( 9.149999999999920419, 12.50000000000000000, -7.253104124594891289 ) ) ;
#53731 = CARTESIAN_POINT ( 'NONE',  ( 2.699999999999947331, 2.500000000000000000, -0.2464101615137783419 ) ) ;
#53732 = EDGE_CURVE ( 'NONE', #32164, #72823, #25794, .T. ) ;
#53733 = EDGE_CURVE ( 'NONE', #29014, #47875, #75957, .T. ) ;
#53734 = FACE_OUTER_BOUND ( 'NONE', #48670, .T. ) ;
#53735 = EDGE_LOOP ( 'NONE', ( #83863, #119643, #91405, #7430 ) ) ;
#53736 = ORIENTED_EDGE ( 'NONE', *, *, #44447, .T. ) ;
#53737 = DIRECTION ( 'NONE',  ( -4.274815082592931898E-19, -0.9999939076577903929, -0.003490651415223739937 ) ) ;
#53738 = FACE_OUTER_BOUND ( 'NONE', #35057, .T. ) ;
#53739 = VECTOR ( 'NONE', #90325, 1000.000000000000000 ) ;
#53740 = DIRECTION ( 'NONE',  ( 0.000000000000000000, -0.9999939076577903929, 0.003490651415223739937 ) ) ;
#53741 = FACE_OUTER_BOUND ( 'NONE', #93260, .T. ) ;
#53742 = AXIS2_PLACEMENT_3D ( 'NONE', #50576, #21115, #61042 ) ;
#53743 = CARTESIAN_POINT ( 'NONE',  ( 8.549999999999924327, 2.500000000000000000, 1.818653347947321475 ) ) ;
#53744 = EDGE_LOOP ( 'NONE', ( #78101, #29470 ) ) ;
#53745 = CIRCLE ( 'NONE', #97661, 0.06509327318403741736 ) ;
#53746 = ORIENTED_EDGE ( 'NONE', *, *, #29745, .F. ) ;
#53747 = DIRECTION ( 'NONE',  ( 0.000000000000000000, -0.000000000000000000, 1.000000000000000000 ) ) ;
#53748 = CARTESIAN_POINT ( 'NONE',  ( -3.100000000000028955, 2.500000000000000000, 3.983716857408420964 ) ) ;
#53750 = CARTESIAN_POINT ( 'NONE',  ( -10.84999999999999964, 2.500000000000000000, 1.472243186433545459 ) ) ;
#53749 = AXIS2_PLACEMENT_3D ( 'NONE', #80848, #31116, #9524 ) ;
#53752 = DIRECTION ( 'NONE',  ( 0.000000000000000000, 0.000000000000000000, 1.000000000000000000 ) ) ;
#53751 = AXIS2_PLACEMENT_3D ( 'NONE', #6274, #114947, #4992 ) ;
#53753 = ORIENTED_EDGE ( 'NONE', *, *, #59657, .T. ) ;
#53754 = CARTESIAN_POINT ( 'NONE',  ( 10.44999999999991402, 2.500000000000000000, 6.495190528383297135 ) ) ;
#53755 = CIRCLE ( 'NONE', #126928, 0.1000000000000002554 ) ;
#53756 = DIRECTION ( 'NONE',  ( 0.000000000000000000, 0.000000000000000000, 1.000000000000000000 ) ) ;
#53757 = ORIENTED_EDGE ( 'NONE', *, *, #127280, .T. ) ;
#53758 = DIRECTION ( 'NONE',  ( 0.000000000000000000, 0.000000000000000000, 1.000000000000000000 ) ) ;
#53759 = ORIENTED_EDGE ( 'NONE', *, *, #55932, .F. ) ;
#53760 = DIRECTION ( 'NONE',  ( 0.000000000000000000, 1.000000000000000000, 0.000000000000000000 ) ) ;
#53762 = AXIS2_PLACEMENT_3D ( 'NONE', #96926, #110460, #98216 ) ;
#53761 = AXIS2_PLACEMENT_3D ( 'NONE', #105678, #25825, #76863 ) ;
#53763 = ORIENTED_EDGE ( 'NONE', *, *, #46005, .T. ) ;
#53764 = CARTESIAN_POINT ( 'NONE',  ( 14.34999999999989306, 2.500000000000000000, -2.411473670974877859 ) ) ;
#53765 = DIRECTION ( 'NONE',  ( 0.000000000000000000, 0.000000000000000000, -1.000000000000000000 ) ) ;
#53766 = EDGE_LOOP ( 'NONE', ( #19112, #61300 ) ) ;
#53767 = VERTEX_POINT ( 'NONE', #74152 ) ;
#53768 = CARTESIAN_POINT ( 'NONE',  ( 185.6302083336747444, -4.367472073101514418, -7.564683531250002702 ) ) ;
#53769 = LINE ( 'NONE', #112055, #85337 ) ;
#53770 = CARTESIAN_POINT ( 'NONE',  ( 186.2135416670080588, 4.367472073101518859, -7.564683531249999149 ) ) ;
#53771 = CARTESIAN_POINT ( 'NONE',  ( 184.4427083336747160, -6.551208109652278289, 3.782341765624995134 ) ) ;
#53772 = ADVANCED_FACE ( 'NONE', ( #45989 ), #124081, .T. ) ;
#53773 = CARTESIAN_POINT ( 'NONE',  ( 108.0000000000000142, 7.119691004531021328, -5.000000000000004441 ) ) ;
#53774 = CARTESIAN_POINT ( 'NONE',  ( 5.799999999999931433, 12.50000000000000000, 4.330127018922196314 ) ) ;
#53775 = DIRECTION ( 'NONE',  ( 0.000000000000000000, 0.000000000000000000, 1.000000000000000000 ) ) ;
#53776 = DIRECTION ( 'NONE',  ( -0.000000000000000000, 1.000000000000000000, -0.000000000000000000 ) ) ;
#53777 = AXIS2_PLACEMENT_3D ( 'NONE', #116046, #87857, #66927 ) ;
#53778 = ORIENTED_EDGE ( 'NONE', *, *, #60831, .F. ) ;
#53779 = ORIENTED_EDGE ( 'NONE', *, *, #110090, .T. ) ;
#53780 = CARTESIAN_POINT ( 'NONE',  ( -8.350000000000010303, 2.500000000000000000, 6.495190528383297135 ) ) ;
#53781 = VERTEX_POINT ( 'NONE', #55158 ) ;
#53782 = DIRECTION ( 'NONE',  ( -0.000000000000000000, 1.000000000000000000, -0.000000000000000000 ) ) ;
#53783 = DIRECTION ( 'NONE',  ( 0.000000000000000000, -0.000000000000000000, 1.000000000000000000 ) ) ;
#53784 = CARTESIAN_POINT ( 'NONE',  ( 87.50000000000001421, 0.000000000000000000, 7.700000000000000178 ) ) ;
#53786 = ORIENTED_EDGE ( 'NONE', *, *, #22712, .T. ) ;
#53785 = EDGE_LOOP ( 'NONE', ( #120248, #84247 ) ) ;
#53787 = CARTESIAN_POINT ( 'NONE',  ( -3.350000000000028511, 12.50000000000000000, 1.472243186433545459 ) ) ;
#53788 = ORIENTED_EDGE ( 'NONE', *, *, #70358, .F. ) ;
#53789 = DIRECTION ( 'NONE',  ( 0.000000000000000000, 1.000000000000000000, 0.000000000000000000 ) ) ;
#53790 = CARTESIAN_POINT ( 'NONE',  ( 187.4609375001707008, 0.000000000000000000, 7.632341765625000107 ) ) ;
#53791 = ORIENTED_EDGE ( 'NONE', *, *, #70120, .F. ) ;
#53792 = LINE ( 'NONE', #24344, #7372 ) ;
#53793 = CARTESIAN_POINT ( 'NONE',  ( 7.899999999999921307, 12.50000000000000000, -2.385244779468109755E-15 ) ) ;
#53794 = AXIS2_PLACEMENT_3D ( 'NONE', #67659, #59820, #78801 ) ;
#53795 = DIRECTION ( 'NONE',  ( 0.000000000000000000, 1.000000000000000000, 0.000000000000000000 ) ) ;
#53796 = CONICAL_SURFACE ( 'NONE', #49708, 0.1000000000000002554, 0.003490658503988666988 ) ;
#53797 = CARTESIAN_POINT ( 'NONE',  ( 9.999999999999914735, 12.50000000000000000, 0.6928203230275494784 ) ) ;
#53798 = DIRECTION ( 'NONE',  ( 0.000000000000000000, 0.000000000000000000, 1.000000000000000000 ) ) ;
#53799 = CARTESIAN_POINT ( 'NONE',  ( 15.39999999999989022, 2.500000000000000000, -2.385244779468109755E-15 ) ) ;
#53800 = CARTESIAN_POINT ( 'NONE',  ( 186.9843750003414016, -8.734944146203032389, -1.604583208406767949E-15 ) ) ;
#53801 = DIRECTION ( 'NONE',  ( -0.000000000000000000, 1.000000000000000000, -0.000000000000000000 ) ) ;
#53802 = CARTESIAN_POINT ( 'NONE',  ( -7.100000000000017408, 12.50000000000000000, -5.088040615133791356 ) ) ;
#53804 = VECTOR ( 'NONE', #576, 1000.000000000000000 ) ;
#53803 = AXIS2_PLACEMENT_3D ( 'NONE', #86895, #37802, #96073 ) ;
#53805 = VERTEX_POINT ( 'NONE', #104876 ) ;
#53806 = VERTEX_POINT ( 'NONE', #85879 ) ;
#53807 = CIRCLE ( 'NONE', #126975, 0.06509327318403745899 ) ;
#53808 = ORIENTED_EDGE ( 'NONE', *, *, #16067, .F. ) ;
#53809 = DIRECTION ( 'NONE',  ( -0.000000000000000000, -1.000000000000000000, -0.000000000000000000 ) ) ;
#53810 = VERTEX_POINT ( 'NONE', #36168 ) ;
#53812 = ORIENTED_EDGE ( 'NONE', *, *, #121679, .F. ) ;
#53811 = ORIENTED_EDGE ( 'NONE', *, *, #42527, .T. ) ;
#53813 = ORIENTED_EDGE ( 'NONE', *, *, #86763, .T. ) ;
#53814 = EDGE_CURVE ( 'NONE', #29011, #7017, #55139, .T. ) ;
#53815 = CARTESIAN_POINT ( 'NONE',  ( 13.09999999999990195, 12.50000000000000000, 3.983716857408420076 ) ) ;
#53817 = CONICAL_SURFACE ( 'NONE', #26356, 0.1000000000000002554, 0.003490658503988666988 ) ;
#53816 = CIRCLE ( 'NONE', #87248, 0.1000000000000002554 ) ;
#53819 = EDGE_CURVE ( 'NONE', #21551, #116826, #94840, .T. ) ;
#53818 = AXIS2_PLACEMENT_3D ( 'NONE', #114005, #43981, #83880 ) ;
#53820 = DIRECTION ( 'NONE',  ( 0.000000000000000000, 0.000000000000000000, -1.000000000000000000 ) ) ;
#53821 = CARTESIAN_POINT ( 'NONE',  ( -5.850000000000021849, 12.50000000000000000, -2.922977105672691422 ) ) ;
#53822 = CARTESIAN_POINT ( 'NONE',  ( 13.74999999999993072, 2.500000000000000000, -2.065063509461102065 ) ) ;
#53823 = DIRECTION ( 'NONE',  ( 0.000000000000000000, 0.000000000000000000, 1.000000000000000000 ) ) ;
#53824 = EDGE_CURVE ( 'NONE', #123556, #92862, #13261, .T. ) ;
#53825 = ORIENTED_EDGE ( 'NONE', *, *, #35579, .T. ) ;
#53826 = ADVANCED_FACE ( 'NONE', ( #35524 ), #84374, .T. ) ;
#53827 = DIRECTION ( 'NONE',  ( -0.000000000000000000, -1.000000000000000000, -0.000000000000000000 ) ) ;
#53828 = VERTEX_POINT ( 'NONE', #106194 ) ;
#53829 = VECTOR ( 'NONE', #103047, 1000.000000000000000 ) ;
#53830 = ORIENTED_EDGE ( 'NONE', *, *, #49233, .F. ) ;
#53831 = EDGE_LOOP ( 'NONE', ( #37405, #101110, #108412, #72286 ) ) ;
#53832 = CONICAL_SURFACE ( 'NONE', #7844, 0.1000000000000000472, 0.003490658503988666988 ) ;
#53833 = ADVANCED_FACE ( 'NONE', ( #16494 ), #61410, .T. ) ;
#53835 = EDGE_CURVE ( 'NONE', #18676, #50283, #78130, .T. ) ;
#53834 = DIRECTION ( 'NONE',  ( 0.000000000000000000, 1.000000000000000000, 0.000000000000000000 ) ) ;
#53837 = ORIENTED_EDGE ( 'NONE', *, *, #90994, .T. ) ;
#53836 = EDGE_CURVE ( 'NONE', #75250, #100878, #64958, .T. ) ;
#53838 = ORIENTED_EDGE ( 'NONE', *, *, #34157, .F. ) ;
#53839 = ADVANCED_FACE ( 'NONE', ( #74800 ), #93797, .T. ) ;
#53841 = ORIENTED_EDGE ( 'NONE', *, *, #3141, .F. ) ;
#53840 = EDGE_CURVE ( 'NONE', #72027, #99397, #90418, .T. ) ;
#53842 = VECTOR ( 'NONE', #41761, 1000.000000000000000 ) ;
#53844 = CARTESIAN_POINT ( 'NONE',  ( -11.84999999999999609, 2.500000000000000000, 2.511473670974873507 ) ) ;
#53843 = CIRCLE ( 'NONE', #66349, 0.1000000000000002554 ) ;
#53845 = CARTESIAN_POINT ( 'NONE',  ( -9.550000000000002487, 12.50000000000000000, 6.495190528383297135 ) ) ;
#53847 = AXIS2_PLACEMENT_3D ( 'NONE', #97194, #10103, #109600 ) ;
#53846 = DIRECTION ( 'NONE',  ( 0.000000000000000000, 0.000000000000000000, 1.000000000000000000 ) ) ;
#53848 = CARTESIAN_POINT ( 'NONE',  ( -6.850000000000017408, 12.50000000000000000, -2.511473670974877948 ) ) ;
#53849 = FACE_OUTER_BOUND ( 'NONE', #115873, .T. ) ;
#53850 = DIRECTION ( 'NONE',  ( 0.000000000000000000, 0.000000000000000000, -1.000000000000000000 ) ) ;
#53851 = ADVANCED_FACE ( 'NONE', ( #25682 ), #99055, .T. ) ;
#53852 = CONICAL_SURFACE ( 'NONE', #118683, 0.09999999999999982514, 0.003490658503988666988 ) ;
#53854 = AXIS2_PLACEMENT_3D ( 'NONE', #18690, #99204, #88047 ) ;
#53853 = DIRECTION ( 'NONE',  ( -0.000000000000000000, 1.000000000000000000, -0.000000000000000000 ) ) ;
#53855 = ORIENTED_EDGE ( 'NONE', *, *, #33783, .T. ) ;
#53856 = AXIS2_PLACEMENT_3D ( 'NONE', #126306, #36653, #85082 ) ;
#53857 = AXIS2_PLACEMENT_3D ( 'NONE', #113284, #93020, #3342 ) ;
#53858 = LINE ( 'NONE', #4094, #94493 ) ;
#53859 = EDGE_LOOP ( 'NONE', ( #68836, #45688, #6804, #32591 ) ) ;
#53860 = CARTESIAN_POINT ( 'NONE',  ( 3.749999999999975131, 2.500000000000000000, 6.495190528383297135 ) ) ;
#53861 = EDGE_LOOP ( 'NONE', ( #78233, #17693, #72248, #65229 ) ) ;
#53862 = CIRCLE ( 'NONE', #97772, 0.1000000000000000472 ) ;
#53863 = ORIENTED_EDGE ( 'NONE', *, *, #127186, .F. ) ;
#53864 = CARTESIAN_POINT ( 'NONE',  ( 9.999999999999916511, 2.500000000000000000, -0.6928203230275541413 ) ) ;
#53865 = CARTESIAN_POINT ( 'NONE',  ( -8.550000000000013145, 2.500000000000000000, -1.918653347947326004 ) ) ;
#53867 = CIRCLE ( 'NONE', #127034, 0.09999999999999982514 ) ;
#53866 = CIRCLE ( 'NONE', #106192, 0.09999999999999982514 ) ;
#53868 = DIRECTION ( 'NONE',  ( -4.274815082592931898E-19, -0.9999939076577903929, -0.003490651415223739937 ) ) ;
#53869 = VERTEX_POINT ( 'NONE', #54496 ) ;
#53870 = ORIENTED_EDGE ( 'NONE', *, *, #81842, .T. ) ;
#53871 = DIRECTION ( 'NONE',  ( 0.000000000000000000, -0.9999939076577903929, 0.003490651415223739937 ) ) ;
#53872 = DIRECTION ( 'NONE',  ( 0.000000000000000000, 1.000000000000000000, 0.000000000000000000 ) ) ;
#53873 = APPLICATION_CONTEXT ( 'automotive_design' ) ;
#53874 = CARTESIAN_POINT ( 'NONE',  ( 12.09999999999990195, 2.500000000000000000, -0.1000000000000022815 ) ) ;
#53875 = PLANE ( 'NONE',  #68089 ) ;
#53876 = CARTESIAN_POINT ( 'NONE',  ( 6.649999999999931966, 12.50000000000000000, -7.188010851410854052 ) ) ;
#53877 = ORIENTED_EDGE ( 'NONE', *, *, #80486, .T. ) ;
#53878 = EDGE_CURVE ( 'NONE', #112383, #43675, #113432, .T. ) ;
#53879 = AXIS2_PLACEMENT_3D ( 'NONE', #8382, #117675, #89532 ) ;
#53880 = EDGE_CURVE ( 'NONE', #51819, #11852, #59691, .T. ) ;
#53881 = ORIENTED_EDGE ( 'NONE', *, *, #103649, .F. ) ;
#53882 = DIRECTION ( 'NONE',  ( -0.000000000000000000, 1.000000000000000000, -0.000000000000000000 ) ) ;
#53883 = DIRECTION ( 'NONE',  ( 0.000000000000000000, 0.000000000000000000, -1.000000000000000000 ) ) ;
#53884 = EDGE_CURVE ( 'NONE', #120135, #107678, #75763, .T. ) ;
#53885 = CARTESIAN_POINT ( 'NONE',  ( 184.7968750003414016, 8.734944146203032389, 5.348610694689227483E-16 ) ) ;
#53886 = CARTESIAN_POINT ( 'NONE',  ( 9.799999999999915445, 12.50000000000000000, -4.741630453620015118 ) ) ;
#53887 = CARTESIAN_POINT ( 'NONE',  ( -6.700000000000019718, 12.50000000000000000, -4.330127018922201643 ) ) ;
#53888 = EDGE_CURVE ( 'NONE', #99960, #74427, #97650, .T. ) ;
#53889 = DIRECTION ( 'NONE',  ( 0.000000000000000000, 1.000000000000000000, 0.000000000000000000 ) ) ;
#53890 = CARTESIAN_POINT ( 'NONE',  ( 3.949999999999941558, 2.500000000000000000, -6.248780366869526759 ) ) ;
#53891 = ORIENTED_EDGE ( 'NONE', *, *, #122610, .T. ) ;
#53892 = EDGE_CURVE ( 'NONE', #32647, #46243, #58392, .T. ) ;
#53894 = ADVANCED_FACE ( 'NONE', ( #48561 ), #107473, .T. ) ;
#53893 = AXIS2_PLACEMENT_3D ( 'NONE', #125151, #75387, #35491 ) ;
#53895 = DIRECTION ( 'NONE',  ( -0.000000000000000000, 1.000000000000000000, -0.000000000000000000 ) ) ;
#53896 = CIRCLE ( 'NONE', #10074, 0.06509327318403745899 ) ;
#53897 = ADVANCED_FACE ( 'NONE', ( #46613 ), #2909, .T. ) ;
#53898 = DIRECTION ( 'NONE',  ( 0.000000000000000000, 1.000000000000000000, 0.000000000000000000 ) ) ;
#53899 = CARTESIAN_POINT ( 'NONE',  ( -8.950000000000008171, 12.50000000000000000, 1.818653347947321475 ) ) ;
#53900 = ORIENTED_EDGE ( 'NONE', *, *, #75461, .T. ) ;
#53901 = EDGE_CURVE ( 'NONE', #82923, #81743, #109517, .T. ) ;
#53902 = FACE_OUTER_BOUND ( 'NONE', #3358, .T. ) ;
#53903 = VECTOR ( 'NONE', #32118, 1000.000000000000000 ) ;
#53904 = AXIS2_PLACEMENT_3D ( 'NONE', #110793, #21123, #11306 ) ;
#53905 = ORIENTED_EDGE ( 'NONE', *, *, #110974, .F. ) ;
#53906 = DIRECTION ( 'NONE',  ( 0.000000000000000000, 0.000000000000000000, 1.000000000000000000 ) ) ;
#53907 = ORIENTED_EDGE ( 'NONE', *, *, #79715, .F. ) ;
#53908 = CARTESIAN_POINT ( 'NONE',  ( -2.950000000000029932, 12.50000000000000000, -2.165063509461101710 ) ) ;
#53909 = CARTESIAN_POINT ( 'NONE',  ( -11.84999999999999609, 2.500000000000000000, 6.248780366869521430 ) ) ;
#53910 = DIRECTION ( 'NONE',  ( -0.000000000000000000, 1.000000000000000000, -0.000000000000000000 ) ) ;
#53911 = ORIENTED_EDGE ( 'NONE', *, *, #66107, .T. ) ;
#53912 = VECTOR ( 'NONE', #111912, 1000.000000000000000 ) ;
#53913 = DIRECTION ( 'NONE',  ( 0.000000000000000000, 0.000000000000000000, 1.000000000000000000 ) ) ;
#53914 = CARTESIAN_POINT ( 'NONE',  ( -4.600000000000028066, 2.500000000000000000, -3.637306695894650055 ) ) ;
#53915 = CIRCLE ( 'NONE', #68574, 0.06509327318403745899 ) ;
#53916 = ADVANCED_FACE ( 'NONE', ( #57070 ), #88461, .T. ) ;
#53917 = ORIENTED_EDGE ( 'NONE', *, *, #7943, .F. ) ;
#53918 = CARTESIAN_POINT ( 'NONE',  ( 9.349999999999919709, 2.500000000000000000, 2.411473670974873862 ) ) ;
#53919 = CIRCLE ( 'NONE', #127094, 0.06509327318403745899 ) ;
#53920 = EDGE_LOOP ( 'NONE', ( #78800, #125918 ) ) ;
#53921 = ORIENTED_EDGE ( 'NONE', *, *, #15385, .F. ) ;
#53922 = AXIS2_PLACEMENT_3D ( 'NONE', #117372, #110174, #20507 ) ;
#53923 = CARTESIAN_POINT ( 'NONE',  ( 1.899999999999949507, 2.500000000000000000, 4.776537180435972196 ) ) ;
#53924 = CARTESIAN_POINT ( 'NONE',  ( -8.750000000000012434, 12.50000000000000000, -5.737276932171707422 ) ) ;
#53925 = DIRECTION ( 'NONE',  ( 0.000000000000000000, 1.224646799147352468E-16, 1.000000000000000000 ) ) ;
#53926 = ORIENTED_EDGE ( 'NONE', *, *, #76141, .T. ) ;
#53927 = AXIS2_PLACEMENT_3D ( 'NONE', #123219, #44018, #74120 ) ;
#53928 = DIRECTION ( 'NONE',  ( 0.000000000000000000, 0.000000000000000000, 1.000000000000000000 ) ) ;
#53929 = CARTESIAN_POINT ( 'NONE',  ( -1.650000000000035660, 12.50000000000000000, 2.792790559304612064 ) ) ;
#53930 = VECTOR ( 'NONE', #95532, 1000.000000000000000 ) ;
#53931 = EDGE_LOOP ( 'NONE', ( #82924, #99578 ) ) ;
#53932 = CARTESIAN_POINT ( 'NONE',  ( -4.150000000000027889, 2.500000000000000000, -6.495190528383302464 ) ) ;
#53933 = DIRECTION ( 'NONE',  ( 0.000000000000000000, 0.000000000000000000, 1.000000000000000000 ) ) ;
#53934 = AXIS2_PLACEMENT_3D ( 'NONE', #31058, #121997, #100420 ) ;
#53935 = ADVANCED_FACE ( 'NONE', ( #47277 ), #17251, .T. ) ;
#53936 = CARTESIAN_POINT ( 'NONE',  ( -13.74999999999998934, 12.50000000000000000, 2.792790559304615616 ) ) ;
#53937 = FACE_OUTER_BOUND ( 'NONE', #96244, .T. ) ;
#53938 = PLANE ( 'NONE',  #101045 ) ;
#53939 = DIRECTION ( 'NONE',  ( 0.000000000000000000, 1.000000000000000000, 0.000000000000000000 ) ) ;
#53940 = AXIS2_PLACEMENT_3D ( 'NONE', #105486, #6593, #36104 ) ;
#53941 = DIRECTION ( 'NONE',  ( 0.000000000000000000, 1.000000000000000000, 0.000000000000000000 ) ) ;
#53942 = AXIS2_PLACEMENT_3D ( 'NONE', #70231, #57177, #48020 ) ;
#53943 = AXIS2_PLACEMENT_3D ( 'NONE', #82418, #122970, #53590 ) ;
#53944 = ORIENTED_EDGE ( 'NONE', *, *, #7632, .T. ) ;
#53945 = ORIENTED_EDGE ( 'NONE', *, *, #117507, .F. ) ;
#53946 = ORIENTED_EDGE ( 'NONE', *, *, #31132, .F. ) ;
#53947 = ORIENTED_EDGE ( 'NONE', *, *, #65784, .T. ) ;
#53948 = FACE_OUTER_BOUND ( 'NONE', #32877, .T. ) ;
#53949 = CARTESIAN_POINT ( 'NONE',  ( -3.350000000000031619, 2.500000000000000000, -7.188010851410854052 ) ) ;
#53950 = CARTESIAN_POINT ( 'NONE',  ( -1.250000000000036193, 2.500000000000000000, 5.702370205355745014 ) ) ;
#53951 = VERTEX_POINT ( 'NONE', #27602 ) ;
#53952 = ADVANCED_FACE ( 'NONE', ( #67521 ), #7973, .T. ) ;
#53953 = FACE_BOUND ( 'NONE', #14957, .T. ) ;
#53954 = FACE_OUTER_BOUND ( 'NONE', #10938, .T. ) ;
#53955 = DIRECTION ( 'NONE',  ( 0.000000000000000000, 1.000000000000000000, 0.000000000000000000 ) ) ;
#53956 = DIRECTION ( 'NONE',  ( -0.000000000000000000, 1.000000000000000000, -0.000000000000000000 ) ) ;
#53958 = AXIS2_PLACEMENT_3D ( 'NONE', #12516, #103492, #13798 ) ;
#53957 = AXIS2_PLACEMENT_3D ( 'NONE', #72535, #34555, #64628 ) ;
#53959 = CARTESIAN_POINT ( 'NONE',  ( 12.04999999999990834, 2.500000000000000000, -2.165063509461101710 ) ) ;
#53960 = LINE ( 'NONE', #53327, #122485 ) ;
#53961 = CARTESIAN_POINT ( 'NONE',  ( -3.950000000000024603, 12.50000000000000000, 1.818653347947321475 ) ) ;
#53962 = CARTESIAN_POINT ( 'NONE',  ( -6.050000000000018474, 12.50000000000000000, 6.906693963081109722 ) ) ;
#53963 = FACE_OUTER_BOUND ( 'NONE', #38201, .T. ) ;
#53964 = DIRECTION ( 'NONE',  ( 1.000000000000000000, -0.000000000000000000, -0.000000000000000000 ) ) ;
#53965 = DIRECTION ( 'NONE',  ( 0.000000000000000000, -0.000000000000000000, 1.000000000000000000 ) ) ;
#53966 = ORIENTED_EDGE ( 'NONE', *, *, #58146, .F. ) ;
#53967 = ORIENTED_EDGE ( 'NONE', *, *, #106937, .T. ) ;
#53968 = ORIENTED_EDGE ( 'NONE', *, *, #89947, .T. ) ;
#53969 = ORIENTED_EDGE ( 'NONE', *, *, #109065, .F. ) ;
#53970 = EDGE_LOOP ( 'NONE', ( #97881, #80517 ) ) ;
#53971 = ORIENTED_EDGE ( 'NONE', *, *, #101129, .T. ) ;
#53972 = CARTESIAN_POINT ( 'NONE',  ( -10.65000000000000213, 2.500000000000000000, 1.818653347947321475 ) ) ;
#53973 = VERTEX_POINT ( 'NONE', #86539 ) ;
#53974 = ORIENTED_EDGE ( 'NONE', *, *, #42544, .F. ) ;
#53975 = ADVANCED_FACE ( 'NONE', ( #116641 ), #48895, .T. ) ;
#53977 = AXIS2_PLACEMENT_3D ( 'NONE', #53646, #124323, #74576 ) ;
#53976 = CARTESIAN_POINT ( 'NONE',  ( 12.31005523291632464, -2.500000000000000444, 7.488833080795306962 ) ) ;
#53979 = DIRECTION ( 'NONE',  ( 0.000000000000000000, 0.000000000000000000, 1.000000000000000000 ) ) ;
#53978 = CIRCLE ( 'NONE', #24733, 0.1000000000000002554 ) ;
#53980 = CARTESIAN_POINT ( 'NONE',  ( -3.350000000000028511, 2.500000000000000000, -2.857883832488653741 ) ) ;
#53981 = CIRCLE ( 'NONE', #93685, 0.1000000000000000056 ) ;
#53982 = EDGE_LOOP ( 'NONE', ( #118243, #10087 ) ) ;
#53983 = CARTESIAN_POINT ( 'NONE',  ( 10.39999999999991154, 2.500000000000000000, -5.122947341949753763 ) ) ;
#53984 = ADVANCED_FACE ( 'NONE', ( #47923 ), #82336, .T. ) ;
#53985 = CONICAL_SURFACE ( 'NONE', #87418, 0.1000000000000002554, 0.003490658503988666988 ) ;
#53986 = ORIENTED_EDGE ( 'NONE', *, *, #109915, .T. ) ;
#53987 = CONICAL_SURFACE ( 'NONE', #127156, 0.09999999999999982514, 0.003490658503988666988 ) ;
#53988 = ORIENTED_EDGE ( 'NONE', *, *, #74978, .F. ) ;
#53990 = VERTEX_POINT ( 'NONE', #89122 ) ;
#53989 = CARTESIAN_POINT ( 'NONE',  ( -1.650000000000034328, 2.500000000000000000, -6.595190528383302109 ) ) ;
#53991 = EDGE_CURVE ( 'NONE', #62914, #2669, #7325, .T. ) ;
#53993 = EDGE_CURVE ( 'NONE', #119558, #47762, #108111, .T. ) ;
#53992 = CARTESIAN_POINT ( 'NONE',  ( -9.200000000000006395, 12.50000000000000000, 4.395220292106234439 ) ) ;
#53994 = ADVANCED_FACE ( 'NONE', ( #117927 ), #76067, .T. ) ;
#53995 = EDGE_CURVE ( 'NONE', #85395, #74962, #107154, .T. ) ;
#53996 = VERTEX_POINT ( 'NONE', #129073 ) ;
#53997 = AXIS2_PLACEMENT_3D ( 'NONE', #75792, #5750, #106546 ) ;
#53998 = DIRECTION ( 'NONE',  ( 0.000000000000000000, 1.000000000000000000, 0.000000000000000000 ) ) ;
#53999 = AXIS2_PLACEMENT_3D ( 'NONE', #81126, #23480, #121674 ) ;
#54000 = DIRECTION ( 'NONE',  ( 0.000000000000000000, -0.9999939076577903929, 0.003490651415223739937 ) ) ;
#54001 = LINE ( 'NONE', #73620, #1873 ) ;
#54002 = DIRECTION ( 'NONE',  ( -0.000000000000000000, 1.000000000000000000, -0.000000000000000000 ) ) ;
#54003 = DIRECTION ( 'NONE',  ( 0.000000000000000000, -0.9999939076577903929, 0.003490651415223739937 ) ) ;
#54004 = ADVANCED_FACE ( 'NONE', ( #39407 ), #42638, .T. ) ;
#54005 = ORIENTED_EDGE ( 'NONE', *, *, #128959, .F. ) ;
#54006 = CARTESIAN_POINT ( 'NONE',  ( 0.3999999999999563904, 2.500000000000000000, 3.537306695894645081 ) ) ;
#54007 = EDGE_CURVE ( 'NONE', #1863, #81765, #120520, .T. ) ;
#54008 = CIRCLE ( 'NONE', #112501, 0.1000000000000000056 ) ;
#54009 = ADVANCED_FACE ( 'NONE', ( #22332 ), #50736, .T. ) ;
#54010 = VERTEX_POINT ( 'NONE', #20386 ) ;
#54011 = CARTESIAN_POINT ( 'NONE',  ( 87.50000000000004263, 7.402262750143062675, 1.385127402881716874 ) ) ;
#54012 = EDGE_LOOP ( 'NONE', ( #45820, #51087, #105751, #34090 ) ) ;
#54013 = CARTESIAN_POINT ( 'NONE',  ( -0.8500000000000386136, 2.500000000000000000, 1.572243186433545548 ) ) ;
#54014 = DIRECTION ( 'NONE',  ( 0.000000000000000000, 1.000000000000000000, 0.000000000000000000 ) ) ;
#54015 = AXIS2_PLACEMENT_3D ( 'NONE', #33594, #45993, #23773 ) ;
#54016 = DIRECTION ( 'NONE',  ( 0.000000000000000000, 1.000000000000000000, 0.000000000000000000 ) ) ;
#54017 = DIRECTION ( 'NONE',  ( 0.000000000000000000, -0.9999939076577903929, 0.003490651415223739937 ) ) ;
#54018 = ORIENTED_EDGE ( 'NONE', *, *, #39384, .T. ) ;
#54019 = AXIS2_PLACEMENT_3D ( 'NONE', #34567, #23423, #5071 ) ;
#54020 = MECHANICAL_DESIGN_GEOMETRIC_PRESENTATION_REPRESENTATION (  '', ( #102140 ), #97925 ) ;
#54021 = CARTESIAN_POINT ( 'NONE',  ( -5.650000000000023448, 2.500000000000000000, -2.411473670974877859 ) ) ;
#54022 = ORIENTED_EDGE ( 'NONE', *, *, #115399, .F. ) ;
#54023 = ORIENTED_EDGE ( 'NONE', *, *, #35094, .F. ) ;
#54024 = ORIENTED_EDGE ( 'NONE', *, *, #14547, .F. ) ;
#54025 = DIRECTION ( 'NONE',  ( -0.000000000000000000, 1.000000000000000000, -0.000000000000000000 ) ) ;
#54026 = DIRECTION ( 'NONE',  ( -0.000000000000000000, 1.000000000000000000, -0.000000000000000000 ) ) ;
#54027 = CARTESIAN_POINT ( 'NONE',  ( 185.8177083336747444, 4.367472073101515306, 7.564683531250000925 ) ) ;
#54029 = AXIS2_PLACEMENT_3D ( 'NONE', #26782, #106624, #96797 ) ;
#54028 = DIRECTION ( 'NONE',  ( 0.000000000000000000, 1.000000000000000000, 0.000000000000000000 ) ) ;
#54030 = AXIS2_PLACEMENT_3D ( 'NONE', #41989, #70164, #2045 ) ;
#54031 = DIRECTION ( 'NONE',  ( 0.000000000000000000, 0.000000000000000000, -1.000000000000000000 ) ) ;
#54032 = CARTESIAN_POINT ( 'NONE',  ( -3.550000000000028244, 2.500000000000000000, -1.918653347947326004 ) ) ;
#54033 = VECTOR ( 'NONE', #54429, 1000.000000000000000 ) ;
#54034 = ORIENTED_EDGE ( 'NONE', *, *, #19830, .F. ) ;
#54035 = FACE_OUTER_BOUND ( 'NONE', #59237, .T. ) ;
#54036 = ORIENTED_EDGE ( 'NONE', *, *, #30343, .F. ) ;
#54037 = DIRECTION ( 'NONE',  ( -0.000000000000000000, 1.000000000000000000, -0.000000000000000000 ) ) ;
#54038 = VECTOR ( 'NONE', #90139, 1000.000000000000000 ) ;
#54039 = DIRECTION ( 'NONE',  ( 0.000000000000000000, 1.000000000000000000, 0.000000000000000000 ) ) ;
#54040 = DIRECTION ( 'NONE',  ( -0.000000000000000000, -0.000000000000000000, -1.000000000000000000 ) ) ;
#54041 = ADVANCED_FACE ( 'NONE', ( #11191 ), #46514, .T. ) ;
#54042 = CARTESIAN_POINT ( 'NONE',  ( -9.200000000000006395, 2.500000000000000000, -0.1000000000000023925 ) ) ;
#54043 = ORIENTED_EDGE ( 'NONE', *, *, #56811, .F. ) ;
#54044 = EDGE_CURVE ( 'NONE', #79461, #100575, #41332, .T. ) ;
#54046 = AXIS2_PLACEMENT_3D ( 'NONE', #7674, #55510, #66604 ) ;
#54045 = VECTOR ( 'NONE', #112228, 1000.000000000000000 ) ;
#54047 = ADVANCED_FACE ( 'NONE', ( #112636 ), #122040, .T. ) ;
#54048 = FACE_OUTER_BOUND ( 'NONE', #27122, .T. ) ;
#54050 = EDGE_LOOP ( 'NONE', ( #125796, #107489, #60999, #73207 ) ) ;
#54049 = DIRECTION ( 'NONE',  ( -0.000000000000000000, 1.000000000000000000, -0.000000000000000000 ) ) ;
#54051 = ORIENTED_EDGE ( 'NONE', *, *, #29085, .F. ) ;
#54052 = EDGE_CURVE ( 'NONE', #112102, #7001, #12487, .T. ) ;
#54053 = DIRECTION ( 'NONE',  ( 0.000000000000000000, 1.000000000000000000, 0.000000000000000000 ) ) ;
#54054 = VERTEX_POINT ( 'NONE', #71393 ) ;
#54055 = EDGE_LOOP ( 'NONE', ( #45617, #10031 ) ) ;
#54056 = CARTESIAN_POINT ( 'NONE',  ( -0.2000000000000404232, 12.50000000000000000, 4.048810130592458201 ) ) ;
#54057 = CIRCLE ( 'NONE', #14324, 0.06509327318403745899 ) ;
#54058 = ORIENTED_EDGE ( 'NONE', *, *, #115917, .F. ) ;
#54059 = LINE ( 'NONE', #44894, #94876 ) ;
#54060 = CARTESIAN_POINT ( 'NONE',  ( -13.14999999999999147, 2.500000000000000000, 1.718653347947325383 ) ) ;
#54061 = DIRECTION ( 'NONE',  ( 0.000000000000000000, 0.000000000000000000, 1.000000000000000000 ) ) ;
#54062 = ORIENTED_EDGE ( 'NONE', *, *, #116007, .T. ) ;
#54063 = VECTOR ( 'NONE', #90556, 1000.000000000000000 ) ;
#54064 = AXIS2_PLACEMENT_3D ( 'NONE', #128880, #107915, #39209 ) ;
#54065 = CARTESIAN_POINT ( 'NONE',  ( 13.29999999999990301, 12.50000000000000000, 4.330127018922196314 ) ) ;
#54067 = ORIENTED_EDGE ( 'NONE', *, *, #110729, .T. ) ;
#54066 = DIRECTION ( 'NONE',  ( -4.274815082592931898E-19, -0.9999939076577903929, -0.003490651415223739937 ) ) ;
#54068 = FACE_OUTER_BOUND ( 'NONE', #34827, .T. ) ;
#54069 = FACE_OUTER_BOUND ( 'NONE', #119399, .T. ) ;
#54070 = EDGE_CURVE ( 'NONE', #105674, #50587, #63550, .T. ) ;
#54071 = AXIS2_PLACEMENT_3D ( 'NONE', #124498, #84565, #34844 ) ;
#54072 = ORIENTED_EDGE ( 'NONE', *, *, #44362, .T. ) ;
#54073 = AXIS2_PLACEMENT_3D ( 'NONE', #109371, #39374, #27570 ) ;
#54074 = CIRCLE ( 'NONE', #47829, 0.1000000000000000472 ) ;
#54075 = EDGE_LOOP ( 'NONE', ( #39576, #41320 ) ) ;
#54076 = CONICAL_SURFACE ( 'NONE', #26889, 0.1000000000000000472, 0.003490658503988666988 ) ;
#54077 = VERTEX_POINT ( 'NONE', #100236 ) ;
#54078 = DIRECTION ( 'NONE',  ( 0.000000000000000000, 0.000000000000000000, -1.000000000000000000 ) ) ;
#54079 = DIRECTION ( 'NONE',  ( 0.000000000000000000, 0.000000000000000000, 1.000000000000000000 ) ) ;
#54080 = CARTESIAN_POINT ( 'NONE',  ( 9.399999999999915090, 2.500000000000000000, -4.776537180435977525 ) ) ;
#54081 = FACE_BOUND ( 'NONE', #10049, .T. ) ;
#54082 = ORIENTED_EDGE ( 'NONE', *, *, #35980, .T. ) ;
#54083 = CARTESIAN_POINT ( 'NONE',  ( 186.7760416670080588, 6.551208109652274736, 3.782341765625001351 ) ) ;
#54084 = CONICAL_SURFACE ( 'NONE', #18580, 0.09999999999999982514, 0.003490658503988666988 ) ;
#54085 = DIRECTION ( 'NONE',  ( 0.000000000000000000, 0.000000000000000000, -1.000000000000000000 ) ) ;
#54086 = DIRECTION ( 'NONE',  ( -0.000000000000000000, 1.000000000000000000, -0.000000000000000000 ) ) ;
#54087 = CONICAL_SURFACE ( 'NONE', #20649, 0.1000000000000002554, 0.003490658503988666988 ) ;
#54088 = EDGE_CURVE ( 'NONE', #41131, #53209, #115456, .T. ) ;
#54089 = DIRECTION ( 'NONE',  ( 0.000000000000000000, 0.000000000000000000, 1.000000000000000000 ) ) ;
#54090 = FACE_OUTER_BOUND ( 'NONE', #42225, .T. ) ;
#54091 = DIRECTION ( 'NONE',  ( 0.000000000000000000, 1.000000000000000000, 0.000000000000000000 ) ) ;
#54092 = AXIS2_PLACEMENT_3D ( 'NONE', #12252, #56532, #111761 ) ;
#54093 = DIRECTION ( 'NONE',  ( 0.000000000000000000, -0.9999939076577903929, 0.003490651415223739937 ) ) ;
#54094 = ORIENTED_EDGE ( 'NONE', *, *, #44980, .T. ) ;
#54095 = VERTEX_POINT ( 'NONE', #111312 ) ;
#54096 = ORIENTED_EDGE ( 'NONE', *, *, #69373, .F. ) ;
#54097 = EDGE_LOOP ( 'NONE', ( #20733, #70885 ) ) ;
#54098 = ORIENTED_EDGE ( 'NONE', *, *, #14945, .F. ) ;
#54099 = CONICAL_SURFACE ( 'NONE', #106333, 0.09999999999999982514, 0.003490658503988666988 ) ;
#54100 = DIRECTION ( 'NONE',  ( 0.000000000000000000, 0.000000000000000000, 1.000000000000000000 ) ) ;
#54101 = LINE ( 'NONE', #91443, #80060 ) ;
#54102 = VERTEX_POINT ( 'NONE', #91702 ) ;
#54103 = ADVANCED_FACE ( 'NONE', ( #60329 ), #23839, .T. ) ;
#54104 = FACE_BOUND ( 'NONE', #87903, .T. ) ;
#54105 = DIRECTION ( 'NONE',  ( -0.000000000000000000, 1.000000000000000000, -0.000000000000000000 ) ) ;
#54106 = VECTOR ( 'NONE', #47584, 1000.000000000000000 ) ;
#54107 = ORIENTED_EDGE ( 'NONE', *, *, #105898, .T. ) ;
#54108 = CARTESIAN_POINT ( 'NONE',  ( -14.59999999999998366, 2.500000000000000000, -0.7928203230275520097 ) ) ;
#54109 = EDGE_CURVE ( 'NONE', #42733, #40379, #13052, .T. ) ;
#54110 = PLANE ( 'NONE',  #113847 ) ;
#54111 = CARTESIAN_POINT ( 'NONE',  ( 165.4999999999999716, 0.000000000000000000, -2.000000000000000000 ) ) ;
#54112 = ORIENTED_EDGE ( 'NONE', *, *, #48385, .F. ) ;
#54113 = AXIS2_PLACEMENT_3D ( 'NONE', #9413, #70267, #40166 ) ;
#54114 = CARTESIAN_POINT ( 'NONE',  ( -1.900000000000034994, 12.50000000000000000, -4.676537180435978769 ) ) ;
#54116 = ORIENTED_EDGE ( 'NONE', *, *, #93777, .F. ) ;
#54115 = CIRCLE ( 'NONE', #24874, 0.09999999999999982514 ) ;
#54117 = EDGE_LOOP ( 'NONE', ( #101544, #57883, #20359, #87730 ) ) ;
#54118 = EDGE_LOOP ( 'NONE', ( #20815, #94082, #70984, #116525 ) ) ;
#54119 = DIRECTION ( 'NONE',  ( 0.000000000000000000, 0.000000000000000000, -1.000000000000000000 ) ) ;
#54120 = DIRECTION ( 'NONE',  ( 0.000000000000000000, 0.000000000000000000, 1.000000000000000000 ) ) ;
#54121 = DIRECTION ( 'NONE',  ( -0.000000000000000000, 1.000000000000000000, -0.000000000000000000 ) ) ;
#54122 = AXIS2_PLACEMENT_3D ( 'NONE', #121418, #21962, #59963 ) ;
#54123 = EDGE_LOOP ( 'NONE', ( #54005, #91420, #84234, #63073 ) ) ;
#54124 = LINE ( 'NONE', #94048, #5723 ) ;
#54125 = FACE_OUTER_BOUND ( 'NONE', #60939, .T. ) ;
#54126 = EDGE_CURVE ( 'NONE', #13704, #60192, #23537, .T. ) ;
#54129 = CIRCLE ( 'NONE', #106355, 0.06509327318403745899 ) ;
#54128 = DIRECTION ( 'NONE',  ( 0.000000000000000000, 0.000000000000000000, 1.000000000000000000 ) ) ;
#54127 = VECTOR ( 'NONE', #65937, 1000.000000000000000 ) ;
#54130 = CARTESIAN_POINT ( 'NONE',  ( 186.0312500006828031, 9.429780353434619030E-16, -7.700000000000000178 ) ) ;
#54131 = ORIENTED_EDGE ( 'NONE', *, *, #3021, .F. ) ;
#54132 = CIRCLE ( 'NONE', #97948, 0.1000000000000002554 ) ;
#54133 = PLANE ( 'NONE',  #47440 ) ;
#54134 = ORIENTED_EDGE ( 'NONE', *, *, #18822, .T. ) ;
#54135 = LINE ( 'NONE', #75065, #54658 ) ;
#54136 = ADVANCED_FACE ( 'NONE', ( #110056 ), #10542, .T. ) ;
#54138 = AXIS2_PLACEMENT_3D ( 'NONE', #83532, #13476, #82240 ) ;
#54137 = AXIS2_PLACEMENT_3D ( 'NONE', #84273, #5702, #113091 ) ;
#54139 = ORIENTED_EDGE ( 'NONE', *, *, #18414, .F. ) ;
#54140 = VERTEX_POINT ( 'NONE', #82538 ) ;
#54141 = DIRECTION ( 'NONE',  ( 0.000000000000000000, -1.000000000000000000, 0.000000000000000000 ) ) ;
#54142 = CYLINDRICAL_SURFACE ( 'NONE', #109418, 2.000000000000000000 ) ;
#54143 = EDGE_CURVE ( 'NONE', #118512, #116743, #27739, .T. ) ;
#54144 = PLANE ( 'NONE',  #11177 ) ;
#54146 = ADVANCED_FACE ( 'NONE', ( #30223 ), #50483, .T. ) ;
#54145 = CARTESIAN_POINT ( 'NONE',  ( 6.049999999999932321, 2.500000000000000000, -1.918653347947326004 ) ) ;
#54147 = EDGE_CURVE ( 'NONE', #66596, #120245, #638, .T. ) ;
#54148 = CARTESIAN_POINT ( 'NONE',  ( 8.549999999999924327, 12.50000000000000000, 1.818653347947321475 ) ) ;
#54149 = EDGE_CURVE ( 'NONE', #6351, #5094, #67421, .T. ) ;
#54150 = VERTEX_POINT ( 'NONE', #125650 ) ;
#54151 = VERTEX_POINT ( 'NONE', #124390 ) ;
#54152 = DIRECTION ( 'NONE',  ( 0.000000000000000000, 0.000000000000000000, 1.000000000000000000 ) ) ;
#54153 = CARTESIAN_POINT ( 'NONE',  ( 4.349999999999937472, 12.50000000000000000, 6.841600689897072485 ) ) ;
#54154 = ADVANCED_FACE ( 'NONE', ( #34737 ), #92998, .T. ) ;
#54155 = DIRECTION ( 'NONE',  ( -0.000000000000000000, -1.000000000000000000, -0.000000000000000000 ) ) ;
#54157 = ORIENTED_EDGE ( 'NONE', *, *, #79852, .T. ) ;
#54156 = AXIS2_PLACEMENT_3D ( 'NONE', #68586, #56184, #55558 ) ;
#54158 = ORIENTED_EDGE ( 'NONE', *, *, #119319, .T. ) ;
#54159 = ADVANCED_FACE ( 'NONE', ( #115842 ), #48688, .T. ) ;
#54160 = CARTESIAN_POINT ( 'NONE',  ( -12.04999999999999538, 12.50000000000000000, 6.495190528383297135 ) ) ;
#54161 = ORIENTED_EDGE ( 'NONE', *, *, #40841, .F. ) ;
#54162 = CARTESIAN_POINT ( 'NONE',  ( -6.050000000000017586, 12.50000000000000000, 6.148780366869520009 ) ) ;
#54163 = ADVANCED_FACE ( 'NONE', ( #104721 ), #121825, .T. ) ;
#54164 = CONICAL_SURFACE ( 'NONE', #87588, 0.1000000000000002554, 0.003490658503988666988 ) ;
#54165 = ADVANCED_FACE ( 'NONE', ( #85733 ), #42433, .T. ) ;
#54167 = CARTESIAN_POINT ( 'NONE',  ( -1.450000000000035927, 12.50000000000000000, -1.818653347947326138 ) ) ;
#54166 = CIRCLE ( 'NONE', #129493, 0.1000000000000000472 ) ;
#54168 = EDGE_LOOP ( 'NONE', ( #75329, #16009, #84306, #60937 ) ) ;
#54169 = CARTESIAN_POINT ( 'NONE',  ( 2.099999999999947686, 2.500000000000000000, 5.122947341949749323 ) ) ;
#54170 = DIRECTION ( 'NONE',  ( 0.000000000000000000, 1.000000000000000000, 0.000000000000000000 ) ) ;
#54171 = DIRECTION ( 'NONE',  ( 0.000000000000000000, 0.000000000000000000, -1.000000000000000000 ) ) ;
#54173 = EDGE_CURVE ( 'NONE', #114385, #80836, #21489, .T. ) ;
#54172 = FACE_OUTER_BOUND ( 'NONE', #109540, .T. ) ;
#54174 = AXIS2_PLACEMENT_3D ( 'NONE', #125974, #36345, #6825 ) ;
#54175 = ORIENTED_EDGE ( 'NONE', *, *, #54861, .T. ) ;
#54176 = AXIS2_PLACEMENT_3D ( 'NONE', #50303, #21482, #71887 ) ;
#54178 = DIRECTION ( 'NONE',  ( 0.000000000000000000, -0.9999939076577903929, 0.003490651415223739937 ) ) ;
#54177 = CONICAL_SURFACE ( 'NONE', #31201, 0.09999999999999982514, 0.003490658503988666988 ) ;
#54179 = CARTESIAN_POINT ( 'NONE',  ( 76.40063402951030014, -3.742348971408897107, 5.987205606699626870 ) ) ;
#54180 = VERTEX_POINT ( 'NONE', #125022 ) ;
#54181 = ORIENTED_EDGE ( 'NONE', *, *, #116646, .T. ) ;
#54182 = CARTESIAN_POINT ( 'NONE',  ( 184.4635416670080588, -4.367472073101519747, 7.564683531249999149 ) ) ;
#54183 = CARTESIAN_POINT ( 'NONE',  ( -10.40000000000000213, 12.50000000000000000, -5.088040615133786915 ) ) ;
#54184 = DIRECTION ( 'NONE',  ( -0.000000000000000000, -1.000000000000000000, -0.000000000000000000 ) ) ;
#54185 = AXIS2_PLACEMENT_3D ( 'NONE', #80816, #2224, #42171 ) ;
#54186 = CARTESIAN_POINT ( 'NONE',  ( -12.89999999999999147, 2.500000000000000000, 4.330127018922196314 ) ) ;
#54187 = CARTESIAN_POINT ( 'NONE',  ( -3.750000000000027978, 2.500000000000000000, 7.188010851410848723 ) ) ;
#54188 = CIRCLE ( 'NONE', #125195, 0.06509327318403745899 ) ;
#54189 = CARTESIAN_POINT ( 'NONE',  ( 1.899999999999951283, 12.50000000000000000, -0.3464101615137782364 ) ) ;
#54190 = CARTESIAN_POINT ( 'NONE',  ( 6.649999999999930189, 12.50000000000000000, -1.537336459617587581 ) ) ;
#54191 = DIRECTION ( 'NONE',  ( 0.000000000000000000, 0.000000000000000000, 1.000000000000000000 ) ) ;
#54192 = CARTESIAN_POINT ( 'NONE',  ( -9.150000000000009237, 12.50000000000000000, -6.430097255199259010 ) ) ;
#54193 = PLANE ( 'NONE',  #119401 ) ;
#54194 = CARTESIAN_POINT ( 'NONE',  ( -6.050000000000017586, 2.500000000000000000, 6.148780366869520009 ) ) ;
#54195 = ORIENTED_EDGE ( 'NONE', *, *, #77174, .T. ) ;
#54196 = VERTEX_POINT ( 'NONE', #103458 ) ;
#54197 = VERTEX_POINT ( 'NONE', #75272 ) ;
#54198 = VECTOR ( 'NONE', #107587, 1000.000000000000000 ) ;
#54199 = ORIENTED_EDGE ( 'NONE', *, *, #128803, .F. ) ;
#54200 = FACE_OUTER_BOUND ( 'NONE', #101947, .T. ) ;
#54201 = PLANE ( 'NONE',  #44229 ) ;
#54202 = DIRECTION ( 'NONE',  ( -4.274815082592931898E-19, -0.9999939076577903929, -0.003490651415223739937 ) ) ;
#54203 = ORIENTED_EDGE ( 'NONE', *, *, #71344, .T. ) ;
#54204 = CARTESIAN_POINT ( 'NONE',  ( 3.149999999999944400, 2.500000000000000000, 1.818653347947321475 ) ) ;
#54205 = ADVANCED_FACE ( 'NONE', ( #113267 ), #35366, .T. ) ;
#54206 = EDGE_CURVE ( 'NONE', #79729, #22266, #13146, .T. ) ;
#54207 = CARTESIAN_POINT ( 'NONE',  ( -8.750000000000007105, 12.50000000000000000, 7.188010851410848723 ) ) ;
#54209 = ORIENTED_EDGE ( 'NONE', *, *, #76730, .F. ) ;
#54208 = DIRECTION ( 'NONE',  ( 0.000000000000000000, -0.9999939076577903929, 0.003490651415223739937 ) ) ;
#54210 = DIRECTION ( 'NONE',  ( 0.000000000000000000, -0.000000000000000000, 1.000000000000000000 ) ) ;
#54211 = AXIS2_PLACEMENT_3D ( 'NONE', #120651, #59166, #79449 ) ;
#54212 = CARTESIAN_POINT ( 'NONE',  ( -10.60000000000000320, 2.500000000000000000, -4.676537180435973440 ) ) ;
#54213 = ORIENTED_EDGE ( 'NONE', *, *, #75302, .T. ) ;
#54214 = ADVANCED_FACE ( 'NONE', ( #54990 ), #75854, .T. ) ;
#54215 = ORIENTED_EDGE ( 'NONE', *, *, #53104, .F. ) ;
#54216 = EDGE_LOOP ( 'NONE', ( #83582, #54749, #78802, #103317 ) ) ;
#54217 = ORIENTED_EDGE ( 'NONE', *, *, #28056, .T. ) ;
#54218 = DIRECTION ( 'NONE',  ( -4.274815082592931898E-19, -0.9999939076577903929, -0.003490651415223739937 ) ) ;
#54219 = AXIS2_PLACEMENT_3D ( 'NONE', #50592, #59813, #21135 ) ;
#54220 = LINE ( 'NONE', #113787, #32109 ) ;
#54221 = PLANE ( 'NONE',  #50427 ) ;
#54222 = CARTESIAN_POINT ( 'NONE',  ( 0.6499999999999561684, 2.500000000000000000, -2.411473670974877859 ) ) ;
#54223 = EDGE_LOOP ( 'NONE', ( #24542, #37410, #55007, #108343 ) ) ;
#54225 = AXIS2_PLACEMENT_3D ( 'NONE', #84175, #94006, #14767 ) ;
#54224 = AXIS2_PLACEMENT_3D ( 'NONE', #29261, #108439, #116962 ) ;
#54226 = DIRECTION ( 'NONE',  ( 0.000000000000000000, 0.000000000000000000, 1.000000000000000000 ) ) ;
#54227 = VERTEX_POINT ( 'NONE', #123098 ) ;
#54228 = DIRECTION ( 'NONE',  ( -0.000000000000000000, -1.000000000000000000, -0.000000000000000000 ) ) ;
#54229 = DIRECTION ( 'NONE',  ( -4.274815082592931898E-19, -0.9999939076577903929, -0.003490651415223739937 ) ) ;
#54230 = CARTESIAN_POINT ( 'NONE',  ( -6.650000000000018119, 2.500000000000000000, -2.165063509461101710 ) ) ;
#54231 = CARTESIAN_POINT ( 'NONE',  ( -7.300000000000018474, 2.500000000000000000, 0.4464101615137735513 ) ) ;
#54232 = ORIENTED_EDGE ( 'NONE', *, *, #67387, .F. ) ;
#54234 = CIRCLE ( 'NONE', #12451, 0.1000000000000000472 ) ;
#54233 = AXIS2_PLACEMENT_3D ( 'NONE', #26655, #116942, #48223 ) ;
#54235 = ORIENTED_EDGE ( 'NONE', *, *, #18333, .F. ) ;
#54236 = VERTEX_POINT ( 'NONE', #93636 ) ;
#54237 = DIRECTION ( 'NONE',  ( -0.000000000000000000, 1.000000000000000000, -0.000000000000000000 ) ) ;
#54238 = CARTESIAN_POINT ( 'NONE',  ( -4.400000000000025224, 12.50000000000000000, 4.048810130592458201 ) ) ;
#54239 = CARTESIAN_POINT ( 'NONE',  ( -11.64999999999999680, 2.500000000000000000, 2.265063509461097357 ) ) ;
#54240 = FACE_BOUND ( 'NONE', #128339, .T. ) ;
#54241 = DIRECTION ( 'NONE',  ( 0.000000000000000000, 1.000000000000000000, 0.000000000000000000 ) ) ;
#54242 = FACE_OUTER_BOUND ( 'NONE', #107379, .T. ) ;
#54243 = DIRECTION ( 'NONE',  ( -0.000000000000000000, 1.000000000000000000, -0.000000000000000000 ) ) ;
#54244 = EDGE_CURVE ( 'NONE', #66584, #79607, #5874, .T. ) ;
#54245 = CIRCLE ( 'NONE', #64698, 0.1000000000000002554 ) ;
#54246 = CARTESIAN_POINT ( 'NONE',  ( 187.0468750003414300, -8.734944146203032389, -1.604583208406767949E-15 ) ) ;
#54247 = CARTESIAN_POINT ( 'NONE',  ( 2.949999999999946887, 2.500000000000000000, -6.495190528383302464 ) ) ;
#54248 = DIRECTION ( 'NONE',  ( 0.000000000000000000, 0.000000000000000000, 1.000000000000000000 ) ) ;
#54249 = ORIENTED_EDGE ( 'NONE', *, *, #98185, .T. ) ;
#54250 = AXIS2_PLACEMENT_3D ( 'NONE', #112473, #22813, #70605 ) ;
#54251 = CARTESIAN_POINT ( 'NONE',  ( -8.350000000000013856, 2.500000000000000000, -6.495190528383297135 ) ) ;
#54252 = ORIENTED_EDGE ( 'NONE', *, *, #4601, .F. ) ;
#54253 = ORIENTED_EDGE ( 'NONE', *, *, #76470, .F. ) ;
#54254 = VERTEX_POINT ( 'NONE', #55641 ) ;
#54255 = VERTEX_POINT ( 'NONE', #14412 ) ;
#54256 = EDGE_CURVE ( 'NONE', #65457, #34347, #29901, .T. ) ;
#54257 = DIRECTION ( 'NONE',  ( 0.000000000000000000, 1.000000000000000000, 0.000000000000000000 ) ) ;
#54258 = FACE_BOUND ( 'NONE', #55343, .T. ) ;
#54259 = CARTESIAN_POINT ( 'NONE',  ( 2.049999999999950084, 12.50000000000000000, 2.165063509461097713 ) ) ;
#54260 = CIRCLE ( 'NONE', #58482, 0.06509327318403745899 ) ;
#54261 = VECTOR ( 'NONE', #27271, 1000.000000000000000 ) ;
#54262 = CIRCLE ( 'NONE', #110397, 0.09999999999999982514 ) ;
#54263 = VERTEX_POINT ( 'NONE', #85094 ) ;
#54264 = DIRECTION ( 'NONE',  ( -4.274815082592931898E-19, -0.9999939076577903929, -0.003490651415223739937 ) ) ;
#54265 = EDGE_CURVE ( 'NONE', #7939, #107780, #38229, .T. ) ;
#54266 = CARTESIAN_POINT ( 'NONE',  ( -5.600000000000020073, 12.50000000000000000, 4.741630453620009789 ) ) ;
#54267 = CIRCLE ( 'NONE', #52218, 0.1000000000000002554 ) ;
#54268 = ORIENTED_EDGE ( 'NONE', *, *, #68158, .F. ) ;
#54269 = CARTESIAN_POINT ( 'NONE',  ( -12.09999999999999609, 12.50000000000000000, 4.330127018922196314 ) ) ;
#54270 = CARTESIAN_POINT ( 'NONE',  ( -14.59999999999998366, 2.500000000000000000, -1.084202172485504434E-16 ) ) ;
#54271 = AXIS2_PLACEMENT_3D ( 'NONE', #2844, #4115, #102971 ) ;
#54272 = AXIS2_PLACEMENT_3D ( 'NONE', #44083, #44743, #34287 ) ;
#54273 = ORIENTED_EDGE ( 'NONE', *, *, #96260, .T. ) ;
#54274 = DIRECTION ( 'NONE',  ( -0.000000000000000000, -1.000000000000000000, -0.000000000000000000 ) ) ;
#54275 = CARTESIAN_POINT ( 'NONE',  ( 4.999999999999936939, 12.50000000000000000, -0.6277270498435166823 ) ) ;
#54276 = VERTEX_POINT ( 'NONE', #95571 ) ;
#54277 = DIRECTION ( 'NONE',  ( -0.000000000000000000, 1.000000000000000000, -0.000000000000000000 ) ) ;
#54278 = CARTESIAN_POINT ( 'NONE',  ( 186.8229166673494603, -4.445597072760107515, 7.700000000000023270 ) ) ;
#54279 = FACE_OUTER_BOUND ( 'NONE', #307, .T. ) ;
#54280 = AXIS2_PLACEMENT_3D ( 'NONE', #91169, #98392, #69588 ) ;
#54281 = ORIENTED_EDGE ( 'NONE', *, *, #17806, .F. ) ;
#54282 = EDGE_LOOP ( 'NONE', ( #42073, #98884, #58366, #65785 ) ) ;
#54283 = CARTESIAN_POINT ( 'NONE',  ( 9.399999999999915090, 2.500000000000000000, -4.576537180435977348 ) ) ;
#54284 = ORIENTED_EDGE ( 'NONE', *, *, #79864, .T. ) ;
#54285 = CARTESIAN_POINT ( 'NONE',  ( -8.350000000000012079, 12.50000000000000000, -2.857883832488653741 ) ) ;
#54286 = DIRECTION ( 'NONE',  ( 0.000000000000000000, 0.000000000000000000, -1.000000000000000000 ) ) ;
#54287 = EDGE_CURVE ( 'NONE', #16543, #125159, #13766, .T. ) ;
#54288 = ORIENTED_EDGE ( 'NONE', *, *, #84105, .F. ) ;
#54289 = DIRECTION ( 'NONE',  ( 0.000000000000000000, 0.000000000000000000, 1.000000000000000000 ) ) ;
#54290 = CARTESIAN_POINT ( 'NONE',  ( -7.100000000000018296, 12.50000000000000000, -4.395220292106239768 ) ) ;
#54291 = DIRECTION ( 'NONE',  ( 0.000000000000000000, 0.000000000000000000, 1.000000000000000000 ) ) ;
#54292 = PLANE ( 'NONE',  #88340 ) ;
#54293 = EDGE_CURVE ( 'NONE', #67411, #26300, #17350, .T. ) ;
#54294 = CARTESIAN_POINT ( 'NONE',  ( 9.999999999999948486, 2.500000000000000000, 4.330127018922196314 ) ) ;
#54295 = EDGE_CURVE ( 'NONE', #101138, #69331, #24249, .T. ) ;
#54296 = ORIENTED_EDGE ( 'NONE', *, *, #58968, .F. ) ;
#54297 = ORIENTED_EDGE ( 'NONE', *, *, #75560, .T. ) ;
#54298 = DIRECTION ( 'NONE',  ( 0.000000000000000000, 0.000000000000000000, 1.000000000000000000 ) ) ;
#54299 = LINE ( 'NONE', #11795, #1263 ) ;
#54300 = EDGE_CURVE ( 'NONE', #8031, #63281, #11007, .T. ) ;
#54301 = DIRECTION ( 'NONE',  ( 0.000000000000000000, -0.9999939076577903929, 0.003490651415223739937 ) ) ;
#54303 = VERTEX_POINT ( 'NONE', #26186 ) ;
#54302 = VERTEX_POINT ( 'NONE', #68033 ) ;
#54304 = EDGE_CURVE ( 'NONE', #83081, #39693, #37936, .T. ) ;
#54305 = ORIENTED_EDGE ( 'NONE', *, *, #19381, .T. ) ;
#54306 = CIRCLE ( 'NONE', #39753, 0.06509327318403745899 ) ;
#54307 = EDGE_CURVE ( 'NONE', #50596, #5370, #128102, .T. ) ;
#54308 = DIRECTION ( 'NONE',  ( 0.000000000000000000, 0.000000000000000000, 1.000000000000000000 ) ) ;
#54309 = DIRECTION ( 'NONE',  ( 0.000000000000000000, 0.000000000000000000, 1.000000000000000000 ) ) ;
#54310 = LINE ( 'NONE', #4531, #53930 ) ;
#54311 = DIRECTION ( 'NONE',  ( 1.000000000000000000, 0.000000000000000000, 0.000000000000000000 ) ) ;
#54314 = EDGE_CURVE ( 'NONE', #103678, #91712, #79169, .T. ) ;
#54313 = AXIS2_PLACEMENT_3D ( 'NONE', #96562, #77571, #18012 ) ;
#54312 = CIRCLE ( 'NONE', #27126, 0.06509327318403745899 ) ;
#54315 = DIRECTION ( 'NONE',  ( -4.274815082592931898E-19, -0.9999939076577903929, -0.003490651415223739937 ) ) ;
#54316 = DIRECTION ( 'NONE',  ( 0.000000000000000000, 0.000000000000000000, 1.000000000000000000 ) ) ;
#54317 = CARTESIAN_POINT ( 'NONE',  ( 11.84999999999990727, 12.50000000000000000, -1.753560074763288679 ) ) ;
#54318 = DIRECTION ( 'NONE',  ( 0.000000000000000000, 0.000000000000000000, 1.000000000000000000 ) ) ;
#54319 = DIRECTION ( 'NONE',  ( 0.000000000000000000, 1.000000000000000000, 0.000000000000000000 ) ) ;
#54320 = AXIS2_PLACEMENT_3D ( 'NONE', #56519, #6745, #59115 ) ;
#54322 = ADVANCED_FACE ( 'NONE', ( #18922 ), #96777, .T. ) ;
#54321 = LINE ( 'NONE', #35334, #102103 ) ;
#54323 = AXIS2_PLACEMENT_3D ( 'NONE', #43938, #83836, #84500 ) ;
#54324 = VERTEX_POINT ( 'NONE', #96843 ) ;
#54325 = DIRECTION ( 'NONE',  ( -0.000000000000000000, 1.000000000000000000, -0.000000000000000000 ) ) ;
#54326 = VERTEX_POINT ( 'NONE', #128923 ) ;
#54327 = ORIENTED_EDGE ( 'NONE', *, *, #55703, .T. ) ;
#54328 = CARTESIAN_POINT ( 'NONE',  ( -7.050000000000013145, 2.500000000000000000, 2.165063509461097713 ) ) ;
#54329 = CARTESIAN_POINT ( 'NONE',  ( 10.84999999999991260, 12.50000000000000000, -1.537336459617587581 ) ) ;
#54330 = FACE_OUTER_BOUND ( 'NONE', #121816, .T. ) ;
#54331 = DIRECTION ( 'NONE',  ( 0.000000000000000000, 0.000000000000000000, 1.000000000000000000 ) ) ;
#54332 = DIRECTION ( 'NONE',  ( 0.000000000000000000, 0.000000000000000000, 1.000000000000000000 ) ) ;
#54333 = CARTESIAN_POINT ( 'NONE',  ( -1.250000000000037526, 2.500000000000000000, -1.572243186433550211 ) ) ;
#54334 = FACE_OUTER_BOUND ( 'NONE', #120924, .T. ) ;
#54335 = ORIENTED_EDGE ( 'NONE', *, *, #81891, .T. ) ;
#54336 = CARTESIAN_POINT ( 'NONE',  ( 194.5000000000000000, 0.000000000000000000, 0.000000000000000000 ) ) ;
#54337 = FACE_OUTER_BOUND ( 'NONE', #18077, .T. ) ;
#54338 = ORIENTED_EDGE ( 'NONE', *, *, #24370, .F. ) ;
#54340 = ORIENTED_EDGE ( 'NONE', *, *, #52984, .F. ) ;
#54339 = CIRCLE ( 'NONE', #81534, 0.06509327318403745899 ) ;
#54341 = EDGE_LOOP ( 'NONE', ( #89546, #110453, #36001, #85504 ) ) ;
#54342 = ORIENTED_EDGE ( 'NONE', *, *, #17973, .F. ) ;
#54343 = DIRECTION ( 'NONE',  ( 0.000000000000000000, 0.000000000000000000, 1.000000000000000000 ) ) ;
#54344 = CARTESIAN_POINT ( 'NONE',  ( 12.29999999999990479, 2.500000000000000000, -3.983716857408426293 ) ) ;
#54345 = CIRCLE ( 'NONE', #14610, 0.06509327318403745899 ) ;
#54346 = DIRECTION ( 'NONE',  ( 0.000000000000000000, 1.000000000000000000, 0.000000000000000000 ) ) ;
#54347 = EDGE_CURVE ( 'NONE', #43713, #48486, #31970, .T. ) ;
#54348 = DIRECTION ( 'NONE',  ( -0.000000000000000000, 1.000000000000000000, -0.000000000000000000 ) ) ;
#54349 = CARTESIAN_POINT ( 'NONE',  ( 5.649999999999936406, 2.500000000000000000, -6.841600689897077814 ) ) ;
#54350 = ORIENTED_EDGE ( 'NONE', *, *, #106721, .F. ) ;
#54351 = FACE_OUTER_BOUND ( 'NONE', #5140, .T. ) ;
#54352 = LINE ( 'NONE', #124395, #107986 ) ;
#54353 = AXIS2_PLACEMENT_3D ( 'NONE', #75981, #56330, #118325 ) ;
#54355 = ADVANCED_FACE ( 'NONE', ( #8453 ), #1623, .T. ) ;
#54354 = CARTESIAN_POINT ( 'NONE',  ( 7.899999999999924860, 2.500000000000000000, -3.737306695894649700 ) ) ;
#54356 = CIRCLE ( 'NONE', #129606, 0.09999999999999982514 ) ;
#54357 = EDGE_LOOP ( 'NONE', ( #11792, #24050 ) ) ;
#54358 = CIRCLE ( 'NONE', #58579, 0.1000000000000002554 ) ;
#54359 = ORIENTED_EDGE ( 'NONE', *, *, #35991, .F. ) ;
#54360 = VERTEX_POINT ( 'NONE', #18287 ) ;
#54361 = FACE_OUTER_BOUND ( 'NONE', #62895, .T. ) ;
#54362 = CONICAL_SURFACE ( 'NONE', #94079, 0.1000000000000002554, 0.003490658503988666988 ) ;
#54363 = CIRCLE ( 'NONE', #127529, 0.06509327318403745899 ) ;
#54364 = CARTESIAN_POINT ( 'NONE',  ( -1.900000000000035438, 2.500000000000000000, 3.983716857408420076 ) ) ;
#54365 = CARTESIAN_POINT ( 'NONE',  ( -0.8000000000000315747, 12.50000000000000000, 0.000000000000000000 ) ) ;
#54366 = CIRCLE ( 'NONE', #127535, 0.1000000000000000472 ) ;
#54367 = ORIENTED_EDGE ( 'NONE', *, *, #43403, .T. ) ;
#54368 = DIRECTION ( 'NONE',  ( -0.000000000000000000, -1.000000000000000000, -0.000000000000000000 ) ) ;
#54369 = CARTESIAN_POINT ( 'NONE',  ( -4.600000000000024514, 2.500000000000000000, -0.5928203230275542746 ) ) ;
#54370 = CARTESIAN_POINT ( 'NONE',  ( 9.549999999999915445, 2.500000000000000000, -2.065063509461102065 ) ) ;
#54371 = DIRECTION ( 'NONE',  ( -0.000000000000000000, 1.000000000000000000, -0.000000000000000000 ) ) ;
#54372 = DIRECTION ( 'NONE',  ( 0.000000000000000000, 0.000000000000000000, 1.000000000000000000 ) ) ;
#54373 = ORIENTED_EDGE ( 'NONE', *, *, #65374, .T. ) ;
#54374 = ORIENTED_EDGE ( 'NONE', *, *, #35258, .T. ) ;
#54375 = CARTESIAN_POINT ( 'NONE',  ( 1.049999999999954081, 2.500000000000000000, -6.148780366869526226 ) ) ;
#54376 = CARTESIAN_POINT ( 'NONE',  ( 8.149999999999923972, 2.500000000000000000, -6.741600689897077281 ) ) ;
#54377 = CARTESIAN_POINT ( 'NONE',  ( 12.09999999999990550, 2.500000000000000000, 3.637306695894644726 ) ) ;
#54378 = LINE ( 'NONE', #74672, #125905 ) ;
#54379 = DIRECTION ( 'NONE',  ( -0.000000000000000000, 1.000000000000000000, -0.000000000000000000 ) ) ;
#54380 = ADVANCED_FACE ( 'NONE', ( #78529 ), #82132, .T. ) ;
#54381 = EDGE_LOOP ( 'NONE', ( #57418, #5647, #79248, #113951 ) ) ;
#54382 = CIRCLE ( 'NONE', #117067, 0.06509327318403745899 ) ;
#54383 = VERTEX_POINT ( 'NONE', #17636 ) ;
#54385 = AXIS2_PLACEMENT_3D ( 'NONE', #95369, #14835, #44987 ) ;
#54384 = DIRECTION ( 'NONE',  ( 0.000000000000000000, 0.000000000000000000, -1.000000000000000000 ) ) ;
#54386 = CARTESIAN_POINT ( 'NONE',  ( 6.249999999999967137, 2.500000000000000000, -2.165063509461101710 ) ) ;
#54387 = DIRECTION ( 'NONE',  ( 0.000000000000000000, 0.000000000000000000, 1.000000000000000000 ) ) ;
#54388 = CARTESIAN_POINT ( 'NONE',  ( 6.049999999999934097, 12.50000000000000000, -2.511473670974877948 ) ) ;
#54389 = ORIENTED_EDGE ( 'NONE', *, *, #73261, .T. ) ;
#54390 = EDGE_CURVE ( 'NONE', #24991, #85122, #76575, .T. ) ;
#54391 = DIRECTION ( 'NONE',  ( 0.000000000000000000, -0.9999939076577903929, 0.003490651415223739937 ) ) ;
#54393 = AXIS2_PLACEMENT_3D ( 'NONE', #63755, #52005, #91920 ) ;
#54392 = AXIS2_PLACEMENT_3D ( 'NONE', #3500, #62435, #72887 ) ;
#54394 = CARTESIAN_POINT ( 'NONE',  ( -12.69999999999999218, 2.500000000000000000, -0.3464101615137741286 ) ) ;
#54395 = VERTEX_POINT ( 'NONE', #58238 ) ;
#54396 = EDGE_CURVE ( 'NONE', #113036, #5090, #87028, .T. ) ;
#54397 = DIRECTION ( 'NONE',  ( 0.000000000000000000, 0.000000000000000000, 1.000000000000000000 ) ) ;
#54398 = EDGE_CURVE ( 'NONE', #40560, #72456, #98841, .T. ) ;
#54399 = ORIENTED_EDGE ( 'NONE', *, *, #52279, .T. ) ;
#54400 = DIRECTION ( 'NONE',  ( 0.000000000000000000, -0.000000000000000000, 1.000000000000000000 ) ) ;
#54401 = AXIS2_PLACEMENT_3D ( 'NONE', #62892, #103462, #46295 ) ;
#54402 = EDGE_LOOP ( 'NONE', ( #5421, #5056, #40346, #41214 ) ) ;
#54403 = DIRECTION ( 'NONE',  ( 0.000000000000000000, -0.9999939076577903929, 0.003490651415223739937 ) ) ;
#54404 = DIRECTION ( 'NONE',  ( -0.000000000000000000, 1.000000000000000000, -0.000000000000000000 ) ) ;
#54405 = ADVANCED_FACE ( 'NONE', ( #118422 ), #63351, .T. ) ;
#54406 = ORIENTED_EDGE ( 'NONE', *, *, #59997, .F. ) ;
#54407 = VERTEX_POINT ( 'NONE', #107316 ) ;
#54408 = EDGE_CURVE ( 'NONE', #64010, #43167, #19197, .T. ) ;
#54409 = CARTESIAN_POINT ( 'NONE',  ( 186.8802083336747444, 4.367472073101515306, 7.564683531250000925 ) ) ;
#54410 = DIRECTION ( 'NONE',  ( 0.000000000000000000, 1.000000000000000000, 0.000000000000000000 ) ) ;
#54411 = DIRECTION ( 'NONE',  ( -0.000000000000000000, 1.000000000000000000, -0.000000000000000000 ) ) ;
#54412 = CARTESIAN_POINT ( 'NONE',  ( 2.099999999999950351, 12.50000000000000000, -4.957854068765716882 ) ) ;
#54413 = DIRECTION ( 'NONE',  ( -0.000000000000000000, 1.000000000000000000, -0.000000000000000000 ) ) ;
#54414 = DIRECTION ( 'NONE',  ( 1.000000000000000000, -0.000000000000000000, -0.000000000000000000 ) ) ;
#54415 = DIRECTION ( 'NONE',  ( 0.000000000000000000, 1.000000000000000000, 0.000000000000000000 ) ) ;
#54416 = AXIS2_PLACEMENT_3D ( 'NONE', #102129, #29526, #60297 ) ;
#54417 = VECTOR ( 'NONE', #122910, 1000.000000000000000 ) ;
#54418 = ORIENTED_EDGE ( 'NONE', *, *, #1085, .T. ) ;
#54419 = ORIENTED_EDGE ( 'NONE', *, *, #5688, .T. ) ;
#54420 = CARTESIAN_POINT ( 'NONE',  ( 4.799999999999937650, 2.500000000000000000, -3.883716857408426648 ) ) ;
#54421 = CARTESIAN_POINT ( 'NONE',  ( -5.000000000000023093, 12.50000000000000000, 5.088040615133786027 ) ) ;
#54422 = DIRECTION ( 'NONE',  ( 0.000000000000000000, 0.000000000000000000, 1.000000000000000000 ) ) ;
#54423 = FACE_OUTER_BOUND ( 'NONE', #89426, .T. ) ;
#54425 = VERTEX_POINT ( 'NONE', #51634 ) ;
#54424 = ORIENTED_EDGE ( 'NONE', *, *, #46913, .T. ) ;
#54426 = DIRECTION ( 'NONE',  ( 0.000000000000000000, -0.9999939076577903929, 0.003490651415223739937 ) ) ;
#54427 = ORIENTED_EDGE ( 'NONE', *, *, #50184, .F. ) ;
#54428 = CARTESIAN_POINT ( 'NONE',  ( 11.24999999999990763, 2.500000000000000000, 1.472243186433545459 ) ) ;
#54429 = DIRECTION ( 'NONE',  ( -4.274815082592931898E-19, -0.9999939076577903929, -0.003490651415223739937 ) ) ;
#54430 = AXIS2_PLACEMENT_3D ( 'NONE', #113135, #35239, #4439 ) ;
#54431 = EDGE_LOOP ( 'NONE', ( #57818, #34952, #39153, #121763 ) ) ;
#54432 = DIRECTION ( 'NONE',  ( 0.000000000000000000, 1.000000000000000000, 0.000000000000000000 ) ) ;
#54433 = CARTESIAN_POINT ( 'NONE',  ( 10.84999999999991260, 2.500000000000000000, 7.088010851410848190 ) ) ;
#54434 = EDGE_CURVE ( 'NONE', #124886, #90021, #119778, .T. ) ;
#54435 = DIRECTION ( 'NONE',  ( 0.000000000000000000, 0.000000000000000000, 1.000000000000000000 ) ) ;
#54436 = FACE_OUTER_BOUND ( 'NONE', #82174, .T. ) ;
#54437 = DIRECTION ( 'NONE',  ( 0.000000000000000000, 0.000000000000000000, -1.000000000000000000 ) ) ;
#54438 = CARTESIAN_POINT ( 'NONE',  ( 10.19999999999991225, 2.500000000000000000, 3.983716857408420076 ) ) ;
#54439 = CARTESIAN_POINT ( 'NONE',  ( -11.25000000000000000, 2.500000000000000000, 7.288010851410849256 ) ) ;
#54440 = CARTESIAN_POINT ( 'NONE',  ( -4.999999999999990230, 12.50000000000000000, -4.395220292106239768 ) ) ;
#54441 = DIRECTION ( 'NONE',  ( 0.000000000000000000, 1.000000000000000000, 0.000000000000000000 ) ) ;
#54442 = EDGE_CURVE ( 'NONE', #114390, #87221, #91549, .T. ) ;
#54443 = AXIS2_PLACEMENT_3D ( 'NONE', #56919, #115187, #116501 ) ;
#54444 = ORIENTED_EDGE ( 'NONE', *, *, #109126, .T. ) ;
#54445 = ORIENTED_EDGE ( 'NONE', *, *, #12303, .T. ) ;
#54446 = CIRCLE ( 'NONE', #58666, 0.06509327318403745899 ) ;
#54447 = VERTEX_POINT ( 'NONE', #21521 ) ;
#54448 = DIRECTION ( 'NONE',  ( 0.000000000000000000, 0.000000000000000000, -1.000000000000000000 ) ) ;
#54449 = ORIENTED_EDGE ( 'NONE', *, *, #77914, .F. ) ;
#54450 = DIRECTION ( 'NONE',  ( -4.274815082592931898E-19, -0.9999939076577903929, -0.003490651415223739937 ) ) ;
#54451 = ADVANCED_FACE ( 'NONE', ( #11036 ), #34107, .T. ) ;
#54453 = VERTEX_POINT ( 'NONE', #109908 ) ;
#54452 = ORIENTED_EDGE ( 'NONE', *, *, #34732, .F. ) ;
#54454 = ORIENTED_EDGE ( 'NONE', *, *, #63725, .F. ) ;
#54455 = ADVANCED_FACE ( 'NONE', ( #89615 ), #50830, .T. ) ;
#54456 = FACE_OUTER_BOUND ( 'NONE', #61540, .T. ) ;
#54458 = ADVANCED_FACE ( 'NONE', ( #1866 ), #40476, .T. ) ;
#54457 = CIRCLE ( 'NONE', #96306, 0.1000000000000002554 ) ;
#54459 = CARTESIAN_POINT ( 'NONE',  ( -11.05000000000000071, 2.500000000000000000, -6.841600689897075149 ) ) ;
#54460 = SURFACE_STYLE_FILL_AREA ( #93751 ) ;
#54461 = EDGE_CURVE ( 'NONE', #26094, #127992, #41824, .T. ) ;
#54462 = CARTESIAN_POINT ( 'NONE',  ( 186.8750000000000000, 8.891194145520236347, 5.444286225454521982E-16 ) ) ;
#54463 = LINE ( 'NONE', #2142, #87694 ) ;
#54464 = FACE_OUTER_BOUND ( 'NONE', #47873, .T. ) ;
#54465 = EDGE_LOOP ( 'NONE', ( #49926, #26009, #38463, #6139 ) ) ;
#54467 = ADVANCED_FACE ( 'NONE', ( #100082 ), #124071, .T. ) ;
#54466 = CARTESIAN_POINT ( 'NONE',  ( 11.04999999999990834, 2.500000000000000000, -6.741600689897077281 ) ) ;
#54468 = ORIENTED_EDGE ( 'NONE', *, *, #77354, .T. ) ;
#54469 = EDGE_CURVE ( 'NONE', #18441, #9509, #86407, .T. ) ;
#54470 = ORIENTED_EDGE ( 'NONE', *, *, #74885, .T. ) ;
#54471 = ORIENTED_EDGE ( 'NONE', *, *, #78837, .F. ) ;
#54472 = DIRECTION ( 'NONE',  ( 0.000000000000000000, 0.000000000000000000, 1.000000000000000000 ) ) ;
#54473 = ORIENTED_EDGE ( 'NONE', *, *, #117889, .F. ) ;
#54474 = VERTEX_POINT ( 'NONE', #110537 ) ;
#54475 = EDGE_LOOP ( 'NONE', ( #88576, #50329 ) ) ;
#54476 = CARTESIAN_POINT ( 'NONE',  ( 179.5000000000000000, 1.375000000000002665, -7.634788798650556707 ) ) ;
#54477 = DIRECTION ( 'NONE',  ( 0.000000000000000000, 0.000000000000000000, -1.000000000000000000 ) ) ;
#54478 = DIRECTION ( 'NONE',  ( 0.000000000000000000, 0.000000000000000000, 1.000000000000000000 ) ) ;
#54479 = FACE_OUTER_BOUND ( 'NONE', #36659, .T. ) ;
#54480 = DIRECTION ( 'NONE',  ( 0.000000000000000000, 0.000000000000000000, 1.000000000000000000 ) ) ;
#54481 = AXIS2_PLACEMENT_3D ( 'NONE', #61590, #22315, #22944 ) ;
#54482 = CARTESIAN_POINT ( 'NONE',  ( -3.950000000000026379, 12.50000000000000000, 2.576566944158910744 ) ) ;
#54483 = ORIENTED_EDGE ( 'NONE', *, *, #95922, .T. ) ;
#54484 = AXIS2_PLACEMENT_3D ( 'NONE', #44041, #4096, #93784 ) ;
#54485 = VECTOR ( 'NONE', #19361, 1000.000000000000000 ) ;
#54486 = DIRECTION ( 'NONE',  ( -0.000000000000000000, -1.000000000000000000, -0.000000000000000000 ) ) ;
#54487 = ORIENTED_EDGE ( 'NONE', *, *, #81459, .T. ) ;
#54488 = FACE_OUTER_BOUND ( 'NONE', #21627, .T. ) ;
#54489 = ORIENTED_EDGE ( 'NONE', *, *, #125271, .T. ) ;
#54490 = DIRECTION ( 'NONE',  ( 0.000000000000000000, 0.000000000000000000, 1.000000000000000000 ) ) ;
#54491 = VERTEX_POINT ( 'NONE', #79790 ) ;
#54492 = CIRCLE ( 'NONE', #31513, 0.06509327318403745899 ) ;
#54493 = ORIENTED_EDGE ( 'NONE', *, *, #4630, .T. ) ;
#54494 = DIRECTION ( 'NONE',  ( -0.000000000000000000, -1.000000000000000000, -0.000000000000000000 ) ) ;
#54495 = CARTESIAN_POINT ( 'NONE',  ( 3.349999999999945466, 12.50000000000000000, -2.857883832488653741 ) ) ;
#54496 = CARTESIAN_POINT ( 'NONE',  ( -1.650000000000034772, 2.500000000000000000, 1.572243186433545548 ) ) ;
#54497 = ORIENTED_EDGE ( 'NONE', *, *, #26729, .F. ) ;
#54498 = DIRECTION ( 'NONE',  ( 0.000000000000000000, 0.000000000000000000, 1.000000000000000000 ) ) ;
#54499 = VERTEX_POINT ( 'NONE', #574 ) ;
#54500 = DIRECTION ( 'NONE',  ( -0.000000000000000000, -1.000000000000000000, -0.000000000000000000 ) ) ;
#54501 = LINE ( 'NONE', #94422, #49450 ) ;
#54502 = CARTESIAN_POINT ( 'NONE',  ( -0.8500000000000386136, 12.50000000000000000, 7.188010851410848723 ) ) ;
#54503 = CARTESIAN_POINT ( 'NONE',  ( -9.999999999999969802, 12.50000000000000000, -2.276824562219559311E-15 ) ) ;
#54505 = EDGE_CURVE ( 'NONE', #75521, #23353, #100998, .T. ) ;
#54504 = CARTESIAN_POINT ( 'NONE',  ( -9.800000000000004263, 2.500000000000000000, 3.883716857408420431 ) ) ;
#54506 = VERTEX_POINT ( 'NONE', #30064 ) ;
#54507 = ORIENTED_EDGE ( 'NONE', *, *, #8294, .T. ) ;
#54508 = LINE ( 'NONE', #122626, #105059 ) ;
#54509 = AXIS2_PLACEMENT_3D ( 'NONE', #36808, #57067, #37453 ) ;
#54510 = FACE_OUTER_BOUND ( 'NONE', #48775, .T. ) ;
#54511 = AXIS2_PLACEMENT_3D ( 'NONE', #88778, #29228, #50787 ) ;
#54512 = CARTESIAN_POINT ( 'NONE',  ( 185.7968750003414300, 8.734944146203032389, 5.348610694689227483E-16 ) ) ;
#54513 = CARTESIAN_POINT ( 'NONE',  ( -0.6000000000000383915, 12.50000000000000000, -4.676537180435977881 ) ) ;
#54514 = LINE ( 'NONE', #23134, #75904 ) ;
#54515 = PLANE ( 'NONE',  #98302 ) ;
#54516 = CARTESIAN_POINT ( 'NONE',  ( 2.049999999999950084, 12.50000000000000000, -2.099970236277064473 ) ) ;
#54517 = ORIENTED_EDGE ( 'NONE', *, *, #75888, .F. ) ;
#54518 = AXIS2_PLACEMENT_3D ( 'NONE', #22044, #61961, #110398 ) ;
#54519 = AXIS2_PLACEMENT_3D ( 'NONE', #74777, #25030, #105526 ) ;
#54520 = CARTESIAN_POINT ( 'NONE',  ( -0.4500000000000402012, 12.50000000000000000, 2.165063509461097713 ) ) ;
#54521 = CARTESIAN_POINT ( 'NONE',  ( 11.24999999999994316, 2.500000000000000000, -6.495190528383302464 ) ) ;
#54522 = DIRECTION ( 'NONE',  ( -0.000000000000000000, -1.000000000000000000, -0.000000000000000000 ) ) ;
#54523 = VERTEX_POINT ( 'NONE', #69980 ) ;
#54524 = DIRECTION ( 'NONE',  ( 0.000000000000000000, 0.000000000000000000, 1.000000000000000000 ) ) ;
#54525 = CONICAL_SURFACE ( 'NONE', #10602, 0.1000000000000002554, 0.003490658503988666988 ) ;
#54526 = VERTEX_POINT ( 'NONE', #60173 ) ;
#54527 = CARTESIAN_POINT ( 'NONE',  ( 5.199999999999935341, 2.500000000000000000, -3.983716857408426293 ) ) ;
#54528 = ORIENTED_EDGE ( 'NONE', *, *, #84427, .T. ) ;
#54529 = CARTESIAN_POINT ( 'NONE',  ( -0.6500000000000394351, 2.500000000000000000, 6.841600689897072485 ) ) ;
#54530 = DIRECTION ( 'NONE',  ( 0.000000000000000000, -0.9999939076577903929, 0.003490651415223739937 ) ) ;
#54531 = DIRECTION ( 'NONE',  ( -0.000000000000000000, 1.000000000000000000, -0.000000000000000000 ) ) ;
#54532 = ORIENTED_EDGE ( 'NONE', *, *, #64224, .F. ) ;
#54533 = EDGE_CURVE ( 'NONE', #19040, #39809, #21580, .T. ) ;
#54534 = CARTESIAN_POINT ( 'NONE',  ( 185.7395833340161175, 4.445597072760159030, 7.699999999999928235 ) ) ;
#54535 = CARTESIAN_POINT ( 'NONE',  ( 186.5000000000000000, 0.000000000000000000, 7.700000000000000178 ) ) ;
#54536 = CONICAL_SURFACE ( 'NONE', #60822, 0.09999999999999982514, 0.003490658503988666988 ) ;
#54537 = EDGE_CURVE ( 'NONE', #4682, #44082, #84267, .T. ) ;
#54538 = EDGE_CURVE ( 'NONE', #51372, #2839, #34210, .T. ) ;
#54539 = ORIENTED_EDGE ( 'NONE', *, *, #44603, .T. ) ;
#54540 = DIRECTION ( 'NONE',  ( -0.000000000000000000, 1.000000000000000000, -0.000000000000000000 ) ) ;
#54541 = VERTEX_POINT ( 'NONE', #128026 ) ;
#54542 = ORIENTED_EDGE ( 'NONE', *, *, #48116, .F. ) ;
#54543 = CARTESIAN_POINT ( 'NONE',  ( -4.150000000000024336, 12.50000000000000000, 2.230156782645134950 ) ) ;
#54544 = DIRECTION ( 'NONE',  ( 0.000000000000000000, 1.000000000000000000, 0.000000000000000000 ) ) ;
#54545 = EDGE_CURVE ( 'NONE', #33567, #63146, #50932, .T. ) ;
#54546 = EDGE_CURVE ( 'NONE', #26182, #49424, #27830, .T. ) ;
#54547 = DIRECTION ( 'NONE',  ( 0.000000000000000000, 1.000000000000000000, 0.000000000000000000 ) ) ;
#54548 = ADVANCED_FACE ( 'NONE', ( #27237 ), #57176, .T. ) ;
#54549 = ORIENTED_EDGE ( 'NONE', *, *, #114069, .T. ) ;
#54550 = EDGE_CURVE ( 'NONE', #14780, #121980, #126130, .T. ) ;
#54551 = CARTESIAN_POINT ( 'NONE',  ( -6.050000000000018474, 12.50000000000000000, 2.576566944158910744 ) ) ;
#54552 = CARTESIAN_POINT ( 'NONE',  ( 12.09999999999990550, 12.50000000000000000, 3.572213422710607489 ) ) ;
#54553 = VERTEX_POINT ( 'NONE', #49488 ) ;
#54554 = DIRECTION ( 'NONE',  ( -0.000000000000000000, -1.000000000000000000, -0.000000000000000000 ) ) ;
#54555 = DIRECTION ( 'NONE',  ( 0.000000000000000000, 0.000000000000000000, 1.000000000000000000 ) ) ;
#54557 = DIRECTION ( 'NONE',  ( 0.000000000000000000, 1.000000000000000000, 0.000000000000000000 ) ) ;
#54556 = CIRCLE ( 'NONE', #58786, 0.06509327318403745899 ) ;
#54558 = DIRECTION ( 'NONE',  ( 0.000000000000000000, 0.000000000000000000, 1.000000000000000000 ) ) ;
#54559 = CARTESIAN_POINT ( 'NONE',  ( 12.09999999999990550, 2.500000000000000000, -5.122947341949753763 ) ) ;
#54560 = AXIS2_PLACEMENT_3D ( 'NONE', #28918, #68172, #107465 ) ;
#54561 = CIRCLE ( 'NONE', #106884, 0.06509327318403745899 ) ;
#54562 = CARTESIAN_POINT ( 'NONE',  ( -11.24999999999999822, 12.50000000000000000, 1.472243186433545459 ) ) ;
#54563 = LINE ( 'NONE', #75495, #31667 ) ;
#54564 = CIRCLE ( 'NONE', #117250, 0.09999999999999982514 ) ;
#54565 = VERTEX_POINT ( 'NONE', #126745 ) ;
#54566 = ORIENTED_EDGE ( 'NONE', *, *, #62458, .F. ) ;
#54567 = ORIENTED_EDGE ( 'NONE', *, *, #30718, .T. ) ;
#54568 = EDGE_LOOP ( 'NONE', ( #40148, #107259 ) ) ;
#54569 = DIRECTION ( 'NONE',  ( 0.000000000000000000, 0.000000000000000000, -1.000000000000000000 ) ) ;
#54570 = CARTESIAN_POINT ( 'NONE',  ( 6.649999999999928413, 2.500000000000000000, 2.857883832488649301 ) ) ;
#54571 = AXIS2_PLACEMENT_3D ( 'NONE', #79587, #117542, #69109 ) ;
#54572 = FACE_OUTER_BOUND ( 'NONE', #116056, .T. ) ;
#54573 = ORIENTED_EDGE ( 'NONE', *, *, #95252, .T. ) ;
#54574 = FACE_BOUND ( 'NONE', #7502, .T. ) ;
#54575 = CARTESIAN_POINT ( 'NONE',  ( -10.00000000000000533, 2.500000000000000000, -4.922947341949749145 ) ) ;
#54576 = LINE ( 'NONE', #44789, #100203 ) ;
#54577 = DIRECTION ( 'NONE',  ( 0.000000000000000000, -0.000000000000000000, 1.000000000000000000 ) ) ;
#54578 = DIRECTION ( 'NONE',  ( -0.000000000000000000, 1.000000000000000000, -0.000000000000000000 ) ) ;
#54579 = DIRECTION ( 'NONE',  ( -0.000000000000000000, 1.000000000000000000, -0.000000000000000000 ) ) ;
#54580 = FACE_OUTER_BOUND ( 'NONE', #117823, .T. ) ;
#54581 = PLANE ( 'NONE',  #112325 ) ;
#54582 = FACE_OUTER_BOUND ( 'NONE', #13605, .T. ) ;
#54583 = EDGE_CURVE ( 'NONE', #42141, #76556, #25782, .T. ) ;
#54584 = DIRECTION ( 'NONE',  ( -0.000000000000000000, 1.000000000000000000, -0.000000000000000000 ) ) ;
#54585 = CARTESIAN_POINT ( 'NONE',  ( 10.39999999999991154, 12.50000000000000000, 3.637306695894644726 ) ) ;
#54586 = AXIS2_PLACEMENT_3D ( 'NONE', #24833, #5174, #112580 ) ;
#54587 = ORIENTED_EDGE ( 'NONE', *, *, #18496, .F. ) ;
#54588 = ORIENTED_EDGE ( 'NONE', *, *, #95412, .T. ) ;
#54589 = VERTEX_POINT ( 'NONE', #89394 ) ;
#54590 = ORIENTED_EDGE ( 'NONE', *, *, #42241, .T. ) ;
#54591 = LINE ( 'NONE', #125914, #43644 ) ;
#54592 = VERTEX_POINT ( 'NONE', #129342 ) ;
#54593 = ADVANCED_FACE ( 'NONE', ( #106448 ), #23741, .T. ) ;
#54594 = FACE_OUTER_BOUND ( 'NONE', #125065, .T. ) ;
#54595 = ADVANCED_FACE ( 'NONE', ( #29203 ), #105198, .T. ) ;
#54596 = EDGE_LOOP ( 'NONE', ( #60790, #117126, #66360, #16892 ) ) ;
#54597 = EDGE_LOOP ( 'NONE', ( #52131, #69414, #108159, #89893 ) ) ;
#54598 = EDGE_CURVE ( 'NONE', #63919, #14173, #117698, .T. ) ;
#54599 = CIRCLE ( 'NONE', #94405, 0.06509327318403745899 ) ;
#54600 = CARTESIAN_POINT ( 'NONE',  ( 10.63722763381580272, -2.499999999999999112, 8.014330155767860120 ) ) ;
#54601 = CARTESIAN_POINT ( 'NONE',  ( 13.14999999999989733, 2.500000000000000000, -2.611473670974877592 ) ) ;
#54602 = CARTESIAN_POINT ( 'NONE',  ( 9.999999999999911182, 2.500000000000000000, -3.737306695894649700 ) ) ;
#54603 = EDGE_CURVE ( 'NONE', #93230, #51306, #68448, .T. ) ;
#54604 = CARTESIAN_POINT ( 'NONE',  ( 11.24999999999994493, 2.500000000000000000, -2.065063509461102065 ) ) ;
#54605 = EDGE_CURVE ( 'NONE', #91647, #13873, #2800, .T. ) ;
#54606 =( BOUNDED_SURFACE ( )  B_SPLINE_SURFACE ( 3, 2, ( 
 ( #73603, #21286, #71681 ),
 ( #71042, #120779, #123360 ),
 ( #113537, #122719, #33693 ),
 ( #32435, #121417, #21961 ),
 ( #23887, #61880, #22606 ),
 ( #110942, #62525, #2281 ),
 ( #43531, #63804, #61222 ),
 ( #102437, #52054, #92613 ),
 ( #101149, #33069, #13394 ),
 ( #103732, #14031, #53976 ),
 ( #93908, #4211, #126591 ),
 ( #25150, #95837, #54600 ),
 ( #46739, #86654, #95193 ),
 ( #125296, #123996, #5500 ),
 ( #6775, #104363, #75532 ),
 ( #94536, #116749, #6148 ),
 ( #14674, #36926, #104990 ),
 ( #96458, #67000, #97121 ),
 ( #45464, #76847, #4858 ),
 ( #44813, #36292, #27098 ) ),
 .UNSPECIFIED., .F., .F., .F. ) 
 B_SPLINE_SURFACE_WITH_KNOTS ( ( 4, 2, 2, 2, 2, 2, 2, 2, 2, 4 ),
 ( 3, 3 ),
 ( 9.383769802862040876E-17, 0.0008832438798942619709, 0.001766487759788430050, 0.002649731639682598346, 0.003532975519576766425, 0.005299463279365103016, 0.007065951039153439174, 0.008832438798941775332, 0.01059892655873011236, 0.01413190207830678467 ),
 ( 0.000000000000000000, 1.000000000000000000 ),
 .UNSPECIFIED. ) 
 GEOMETRIC_REPRESENTATION_ITEM ( )  RATIONAL_B_SPLINE_SURFACE ( (
 ( 1.000000000000000000, 0.7071067811865477948, 1.000000000000000000),
 ( 1.000000000000000000, 0.7071067811865477948, 1.000000000000000000),
 ( 1.000000000000000000, 0.7071067811865471286, 1.000000000000000000),
 ( 1.000000000000000000, 0.7071067811865471286, 1.000000000000000000),
 ( 1.000000000000000000, 0.7071067811865477948, 1.000000000000000000),
 ( 1.000000000000000000, 0.7071067811865477948, 1.000000000000000000),
 ( 1.000000000000000000, 0.7071067811865476838, 1.000000000000000000),
 ( 1.000000000000000000, 0.7071067811865476838, 1.000000000000000000),
 ( 1.000000000000000000, 0.7071067811865472397, 1.000000000000000000),
 ( 1.000000000000000000, 0.7071067811865472397, 1.000000000000000000),
 ( 1.000000000000000000, 0.7071067811865474617, 1.000000000000000000),
 ( 1.000000000000000000, 0.7071067811865474617, 1.000000000000000000),
 ( 1.000000000000000000, 0.7071067811865474617, 1.000000000000000000),
 ( 1.000000000000000000, 0.7071067811865474617, 1.000000000000000000),
 ( 1.000000000000000000, 0.7071067811865477948, 1.000000000000000000),
 ( 1.000000000000000000, 0.7071067811865477948, 1.000000000000000000),
 ( 1.000000000000000000, 0.7071067811865473507, 1.000000000000000000),
 ( 1.000000000000000000, 0.7071067811865473507, 1.000000000000000000),
 ( 1.000000000000000000, 0.7071067811865472397, 1.000000000000000000),
 ( 1.000000000000000000, 0.7071067811865472397, 1.000000000000000000) ) ) 
 REPRESENTATION_ITEM ( '' )  SURFACE ( )  );
#54607 = ORIENTED_EDGE ( 'NONE', *, *, #83650, .F. ) ;
#54608 = CONICAL_SURFACE ( 'NONE', #71329, 0.1000000000000002554, 0.003490658503988666988 ) ;
#54609 = EDGE_CURVE ( 'NONE', #1900, #126243, #107344, .T. ) ;
#54610 = AXIS2_PLACEMENT_3D ( 'NONE', #7144, #47105, #54968 ) ;
#54611 = ADVANCED_FACE ( 'NONE', ( #29830 ), #61299, .T. ) ;
#54612 = ORIENTED_EDGE ( 'NONE', *, *, #80188, .T. ) ;
#54613 = EDGE_CURVE ( 'NONE', #103318, #126889, #39036, .T. ) ;
#54614 = VERTEX_POINT ( 'NONE', #76991 ) ;
#54616 = ORIENTED_EDGE ( 'NONE', *, *, #62602, .T. ) ;
#54615 = CARTESIAN_POINT ( 'NONE',  ( 1.849999999999949685, 12.50000000000000000, -2.511473670974877948 ) ) ;
#54617 = CARTESIAN_POINT ( 'NONE',  ( 184.5416666666666572, -4.445597072760039126, 7.700000000000142286 ) ) ;
#54618 = ORIENTED_EDGE ( 'NONE', *, *, #54613, .T. ) ;
#54619 = ORIENTED_EDGE ( 'NONE', *, *, #22245, .F. ) ;
#54620 = ADVANCED_FACE ( 'NONE', ( #57351 ), #97273, .T. ) ;
#54621 = DIRECTION ( 'NONE',  ( 0.000000000000000000, 1.000000000000000000, 0.000000000000000000 ) ) ;
#54622 = CIRCLE ( 'NONE', #50429, 0.06509327318403745899 ) ;
#54623 = LINE ( 'NONE', #74288, #16184 ) ;
#54624 = CARTESIAN_POINT ( 'NONE',  ( -3.350000000000028955, 2.500000000000000000, 2.265063509461097357 ) ) ;
#54625 = CARTESIAN_POINT ( 'NONE',  ( -10.85000000000000142, 12.50000000000000000, -7.188010851410850499 ) ) ;
#54626 = AXIS2_PLACEMENT_3D ( 'NONE', #112963, #92033, #13463 ) ;
#54627 = CARTESIAN_POINT ( 'NONE',  ( -8.950000000000008171, 2.500000000000000000, -2.411473670974877859 ) ) ;
#54628 = AXIS2_PLACEMENT_3D ( 'NONE', #92058, #2371, #73701 ) ;
#54629 = EDGE_LOOP ( 'NONE', ( #40492, #32569 ) ) ;
#54630 = CARTESIAN_POINT ( 'NONE',  ( 13.29999999999990301, 2.500000000000000000, -4.330127018922201643 ) ) ;
#54631 = VERTEX_POINT ( 'NONE', #87442 ) ;
#54632 = CARTESIAN_POINT ( 'NONE',  ( 17.50000000000000000, 2.500000000000000000, -3.999999999999996447 ) ) ;
#54633 = VERTEX_POINT ( 'NONE', #37717 ) ;
#54634 = DIRECTION ( 'NONE',  ( -0.000000000000000000, 1.000000000000000000, -0.000000000000000000 ) ) ;
#54635 = CONICAL_SURFACE ( 'NONE', #35870, 0.1000000000000002554, 0.003490658503988666988 ) ;
#54636 = CIRCLE ( 'NONE', #125644, 0.09999999999999999167 ) ;
#54637 = DIRECTION ( 'NONE',  ( 0.000000000000000000, -0.000000000000000000, 1.000000000000000000 ) ) ;
#54638 = CARTESIAN_POINT ( 'NONE',  ( 6.249999999999967137, 12.50000000000000000, -2.230156782645139391 ) ) ;
#54639 = CARTESIAN_POINT ( 'NONE',  ( 0.7999999999999548583, 2.500000000000000000, 4.330127018922196314 ) ) ;
#54640 = EDGE_LOOP ( 'NONE', ( #48446, #61783, #112505, #68612 ) ) ;
#54641 = CARTESIAN_POINT ( 'NONE',  ( 1.649999999999948841, 12.50000000000000000, 6.495190528383297135 ) ) ;
#54642 = DIRECTION ( 'NONE',  ( 0.000000000000000000, 0.000000000000000000, 1.000000000000000000 ) ) ;
#54643 = VERTEX_POINT ( 'NONE', #77622 ) ;
#54644 = ORIENTED_EDGE ( 'NONE', *, *, #29269, .F. ) ;
#54645 = ORIENTED_EDGE ( 'NONE', *, *, #109409, .T. ) ;
#54646 = DIRECTION ( 'NONE',  ( 0.000000000000000000, 1.000000000000000000, 0.000000000000000000 ) ) ;
#54647 = FACE_OUTER_BOUND ( 'NONE', #44069, .T. ) ;
#54648 = CARTESIAN_POINT ( 'NONE',  ( 186.9010416670080303, -4.367472073101519747, 7.564683531249999149 ) ) ;
#54649 = CARTESIAN_POINT ( 'NONE',  ( 13.14999999999990088, 2.500000000000000000, 2.511473670974873507 ) ) ;
#54651 = ADVANCED_FACE ( 'NONE', ( #18710 ), #55019, .T. ) ;
#54650 = CARTESIAN_POINT ( 'NONE',  ( 11.84999999999990727, 12.50000000000000000, -1.818653347947326138 ) ) ;
#54652 = DIRECTION ( 'NONE',  ( -0.000000000000000000, 1.000000000000000000, -0.000000000000000000 ) ) ;
#54653 = AXIS2_PLACEMENT_3D ( 'NONE', #75116, #85574, #36499 ) ;
#54654 = VECTOR ( 'NONE', #76064, 1000.000000000000000 ) ;
#54655 = ORIENTED_EDGE ( 'NONE', *, *, #57239, .T. ) ;
#54656 = DIRECTION ( 'NONE',  ( 0.000000000000000000, -0.000000000000000000, 1.000000000000000000 ) ) ;
#54657 = CIRCLE ( 'NONE', #96508, 0.1000000000000000472 ) ;
#54658 = VECTOR ( 'NONE', #4355, 1000.000000000000000 ) ;
#54659 = EDGE_LOOP ( 'NONE', ( #128457, #95523, #129024, #107755 ) ) ;
#54660 = AXIS2_PLACEMENT_3D ( 'NONE', #6158, #44826, #55282 ) ;
#54661 = EDGE_CURVE ( 'NONE', #9617, #5036, #60872, .T. ) ;
#54662 = LINE ( 'NONE', #23943, #18301 ) ;
#54663 = LINE ( 'NONE', #94589, #102805 ) ;
#54664 = DIRECTION ( 'NONE',  ( -4.274815082592931898E-19, -0.9999939076577903929, -0.003490651415223739937 ) ) ;
#54665 = EDGE_LOOP ( 'NONE', ( #53652, #73922 ) ) ;
#54666 = DIRECTION ( 'NONE',  ( 0.000000000000000000, -0.9999939076577903929, 0.003490651415223739937 ) ) ;
#54667 = LINE ( 'NONE', #95269, #104018 ) ;
#54668 = ORIENTED_EDGE ( 'NONE', *, *, #127741, .F. ) ;
#54669 = DIRECTION ( 'NONE',  ( -0.000000000000000000, -1.000000000000000000, -0.000000000000000000 ) ) ;
#54670 = ORIENTED_EDGE ( 'NONE', *, *, #90962, .F. ) ;
#54671 = ORIENTED_EDGE ( 'NONE', *, *, #52192, .T. ) ;
#54672 = CARTESIAN_POINT ( 'NONE',  ( -11.24999999999996270, 2.500000000000000000, 6.395190528383296602 ) ) ;
#54673 = ORIENTED_EDGE ( 'NONE', *, *, #123563, .F. ) ;
#54674 = CARTESIAN_POINT ( 'NONE',  ( 2.299999999999949640, 2.500000000000000000, -0.4464101615137782142 ) ) ;
#54675 = DIRECTION ( 'NONE',  ( 0.000000000000000000, 1.000000000000000000, 0.000000000000000000 ) ) ;
#54676 = DIRECTION ( 'NONE',  ( 0.000000000000000000, 1.000000000000000000, 0.000000000000000000 ) ) ;
#54677 = AXIS2_PLACEMENT_3D ( 'NONE', #97337, #7004, #17470 ) ;
#54678 = VERTEX_POINT ( 'NONE', #120442 ) ;
#54679 = AXIS2_PLACEMENT_3D ( 'NONE', #35513, #125793, #95717 ) ;
#54680 = EDGE_CURVE ( 'NONE', #91293, #64031, #128198, .T. ) ;
#54681 = FACE_BOUND ( 'NONE', #68437, .T. ) ;
#54682 = CARTESIAN_POINT ( 'NONE',  ( -3.550000000000028688, 2.500000000000000000, 6.841600689897072485 ) ) ;
#54684 = ORIENTED_EDGE ( 'NONE', *, *, #31293, .F. ) ;
#54683 = CARTESIAN_POINT ( 'NONE',  ( -8.749999999999975131, 2.500000000000000000, 2.065063509461097624 ) ) ;
#54685 = CARTESIAN_POINT ( 'NONE',  ( -5.200000000000022382, 12.50000000000000000, 4.676537180435972552 ) ) ;
#54686 = CARTESIAN_POINT ( 'NONE',  ( -1.322875655532295136, -2.500000000000000444, -5.000000000000004441 ) ) ;
#54687 = AXIS2_PLACEMENT_3D ( 'NONE', #88996, #69336, #9784 ) ;
#54688 = EDGE_CURVE ( 'NONE', #121723, #26124, #62182, .T. ) ;
#54689 = ORIENTED_EDGE ( 'NONE', *, *, #56393, .F. ) ;
#54690 = CIRCLE ( 'NONE', #94507, 0.06509327318403745899 ) ;
#54691 = CONICAL_SURFACE ( 'NONE', #127876, 0.1000000000000002554, 0.003490658503988666988 ) ;
#54692 = AXIS2_PLACEMENT_3D ( 'NONE', #20713, #121470, #119538 ) ;
#54693 = ORIENTED_EDGE ( 'NONE', *, *, #41777, .F. ) ;
#54694 = ORIENTED_EDGE ( 'NONE', *, *, #36594, .F. ) ;
#54695 = DIRECTION ( 'NONE',  ( -0.000000000000000000, -1.000000000000000000, -0.000000000000000000 ) ) ;
#54696 = DIRECTION ( 'NONE',  ( 0.000000000000000000, 0.000000000000000000, -1.000000000000000000 ) ) ;
#54697 = EDGE_CURVE ( 'NONE', #60586, #101827, #100161, .T. ) ;
#54698 = EDGE_CURVE ( 'NONE', #101462, #1863, #63440, .T. ) ;
#54699 = DIRECTION ( 'NONE',  ( 0.000000000000000000, -0.000000000000000000, 1.000000000000000000 ) ) ;
#54700 = EDGE_CURVE ( 'NONE', #79310, #57270, #6972, .T. ) ;
#54701 = FACE_BOUND ( 'NONE', #121611, .T. ) ;
#54703 = EDGE_CURVE ( 'NONE', #118649, #80208, #9050, .T. ) ;
#54702 = VERTEX_POINT ( 'NONE', #3249 ) ;
#54704 = CARTESIAN_POINT ( 'NONE',  ( 185.4010416670080588, -4.367472073101519747, 7.564683531249999149 ) ) ;
#54705 = EDGE_CURVE ( 'NONE', #34772, #86996, #1939, .T. ) ;
#54706 = CARTESIAN_POINT ( 'NONE',  ( 2.499999999999983569, 2.500000000000000000, -2.276824562219559311E-15 ) ) ;
#54707 = CARTESIAN_POINT ( 'NONE',  ( 14.99999999999989342, 2.500000000000000000, -0.5928203230275541635 ) ) ;
#54708 = AXIS2_PLACEMENT_3D ( 'NONE', #37655, #59239, #117449 ) ;
#54709 = DIRECTION ( 'NONE',  ( -0.000000000000000000, 1.000000000000000000, -0.000000000000000000 ) ) ;
#54710 = CONICAL_SURFACE ( 'NONE', #69477, 0.1000000000000002554, 0.003490658503988666988 ) ;
#54711 = CARTESIAN_POINT ( 'NONE',  ( 4.149999999999941735, 2.500000000000000000, -1.472243186433550122 ) ) ;
#54712 = AXIS2_PLACEMENT_3D ( 'NONE', #5366, #123847, #43390 ) ;
#54713 = CIRCLE ( 'NONE', #38301, 0.1000000000000002554 ) ;
#54714 = CARTESIAN_POINT ( 'NONE',  ( -4.600000000000028066, 2.500000000000000000, -5.022947341949754119 ) ) ;
#54715 = FACE_OUTER_BOUND ( 'NONE', #38833, .T. ) ;
#54716 = EDGE_CURVE ( 'NONE', #39745, #127685, #42532, .T. ) ;
#54717 = CARTESIAN_POINT ( 'NONE',  ( -3.750000000000029310, 12.50000000000000000, -7.188010851410854052 ) ) ;
#54718 = AXIS2_PLACEMENT_3D ( 'NONE', #100445, #71626, #42172 ) ;
#54719 = EDGE_CURVE ( 'NONE', #68377, #115059, #80163, .T. ) ;
#54720 = EDGE_CURVE ( 'NONE', #82397, #19127, #90720, .T. ) ;
#54721 = DIRECTION ( 'NONE',  ( 0.000000000000000000, -0.9999939076577903929, 0.003490651415223739937 ) ) ;
#54722 = VERTEX_POINT ( 'NONE', #50403 ) ;
#54723 = AXIS2_PLACEMENT_3D ( 'NONE', #15111, #66169, #104791 ) ;
#54724 = ORIENTED_EDGE ( 'NONE', *, *, #66419, .F. ) ;
#54725 = EDGE_LOOP ( 'NONE', ( #13880, #11275 ) ) ;
#54726 = EDGE_LOOP ( 'NONE', ( #22395, #28718 ) ) ;
#54727 = EDGE_LOOP ( 'NONE', ( #79931, #67611, #98435, #123352 ) ) ;
#54728 = DIRECTION ( 'NONE',  ( 0.000000000000000000, 1.000000000000000000, 0.000000000000000000 ) ) ;
#54729 = DIRECTION ( 'NONE',  ( 0.000000000000000000, 0.000000000000000000, 1.000000000000000000 ) ) ;
#54730 = ORIENTED_EDGE ( 'NONE', *, *, #28186, .T. ) ;
#54731 = FACE_BOUND ( 'NONE', #60898, .T. ) ;
#54732 = CARTESIAN_POINT ( 'NONE',  ( 1.649999999999951505, 2.500000000000000000, -1.372243186433550033 ) ) ;
#54733 = CARTESIAN_POINT ( 'NONE',  ( -0.2000000000000339284, 2.500000000000000000, -0.4464101615137759382 ) ) ;
#54734 = ORIENTED_EDGE ( 'NONE', *, *, #62884, .T. ) ;
#54735 = FACE_OUTER_BOUND ( 'NONE', #87894, .T. ) ;
#54736 = CARTESIAN_POINT ( 'NONE',  ( -10.45000000000000107, 2.500000000000000000, 2.265063509461097357 ) ) ;
#54737 = DIRECTION ( 'NONE',  ( 0.000000000000000000, 0.000000000000000000, 1.000000000000000000 ) ) ;
#54738 = EDGE_LOOP ( 'NONE', ( #47960, #106395 ) ) ;
#54739 = DIRECTION ( 'NONE',  ( 0.000000000000000000, 0.000000000000000000, 1.000000000000000000 ) ) ;
#54740 = ORIENTED_EDGE ( 'NONE', *, *, #39213, .T. ) ;
#54741 = ORIENTED_EDGE ( 'NONE', *, *, #113666, .F. ) ;
#54742 = VECTOR ( 'NONE', #14769, 1000.000000000000000 ) ;
#54743 = ORIENTED_EDGE ( 'NONE', *, *, #49233, .T. ) ;
#54744 = CIRCLE ( 'NONE', #23560, 0.1000000000000002554 ) ;
#54745 = LINE ( 'NONE', #64575, #6670 ) ;
#54746 = AXIS2_PLACEMENT_3D ( 'NONE', #100836, #91036, #79924 ) ;
#54747 = FACE_OUTER_BOUND ( 'NONE', #1036, .T. ) ;
#54748 = CARTESIAN_POINT ( 'NONE',  ( -3.642919299551294898E-14, 12.50000000000000000, 0.6928203230275518099 ) ) ;
#54749 = ORIENTED_EDGE ( 'NONE', *, *, #67891, .T. ) ;
#54750 = CARTESIAN_POINT ( 'NONE',  ( 2.500000000000002220, 2.499999999999998668, -9.000000000000000000 ) ) ;
#54751 = CARTESIAN_POINT ( 'NONE',  ( 1.649999999999951950, 2.500000000000000000, -7.088010851410853519 ) ) ;
#54752 = CONICAL_SURFACE ( 'NONE', #127928, 0.1000000000000000472, 0.003490658503988666988 ) ;
#54753 = AXIS2_PLACEMENT_3D ( 'NONE', #14411, #54346, #101522 ) ;
#54754 = CIRCLE ( 'NONE', #73536, 0.06509327318403745899 ) ;
#54755 = DIRECTION ( 'NONE',  ( -0.000000000000000000, 1.000000000000000000, -0.000000000000000000 ) ) ;
#54756 = CARTESIAN_POINT ( 'NONE',  ( 185.0729166673494888, 4.445597072760120838, -7.699999999999998401 ) ) ;
#54758 = VERTEX_POINT ( 'NONE', #110613 ) ;
#54757 = DIRECTION ( 'NONE',  ( 0.000000000000000000, -0.9999939076577903929, 0.003490651415223739937 ) ) ;
#54759 = AXIS2_PLACEMENT_3D ( 'NONE', #60590, #1635, #120137 ) ;
#54760 = CIRCLE ( 'NONE', #71490, 0.06509327318403743123 ) ;
#54761 = DIRECTION ( 'NONE',  ( 0.000000000000000000, 1.000000000000000000, 0.000000000000000000 ) ) ;
#54762 = ADVANCED_FACE ( 'NONE', ( #11112 ), #51029, .T. ) ;
#54763 = ORIENTED_EDGE ( 'NONE', *, *, #105893, .F. ) ;
#54764 = DIRECTION ( 'NONE',  ( 0.000000000000000000, 0.000000000000000000, 1.000000000000000000 ) ) ;
#54765 = CONICAL_SURFACE ( 'NONE', #29649, 0.09999999999999982514, 0.003490658503988666988 ) ;
#54766 = EDGE_CURVE ( 'NONE', #38253, #112855, #53072, .T. ) ;
#54767 = EDGE_LOOP ( 'NONE', ( #64574, #35749, #103685, #46292 ) ) ;
#54768 = EDGE_CURVE ( 'NONE', #73062, #66361, #73999, .T. ) ;
#54769 = ORIENTED_EDGE ( 'NONE', *, *, #54149, .F. ) ;
#54770 = CARTESIAN_POINT ( 'NONE',  ( 3.299999999999944755, 12.50000000000000000, -4.395220292106239768 ) ) ;
#54771 = DIRECTION ( 'NONE',  ( -0.000000000000000000, -1.000000000000000000, -0.000000000000000000 ) ) ;
#54772 = DIRECTION ( 'NONE',  ( 0.000000000000000000, 0.000000000000000000, 1.000000000000000000 ) ) ;
#54773 = FACE_OUTER_BOUND ( 'NONE', #65478, .T. ) ;
#54774 = LINE ( 'NONE', #94068, #34940 ) ;
#54775 = ORIENTED_EDGE ( 'NONE', *, *, #27785, .F. ) ;
#54776 = EDGE_CURVE ( 'NONE', #25337, #22838, #128296, .T. ) ;
#54777 = VERTEX_POINT ( 'NONE', #102090 ) ;
#54778 = PLANE ( 'NONE',  #85249 ) ;
#54779 = DIRECTION ( 'NONE',  ( -0.000000000000000000, -1.000000000000000000, -0.000000000000000000 ) ) ;
#54780 = FACE_OUTER_BOUND ( 'NONE', #56431, .T. ) ;
#54781 = ORIENTED_EDGE ( 'NONE', *, *, #15050, .F. ) ;
#54782 = VERTEX_POINT ( 'NONE', #12407 ) ;
#54783 = DIRECTION ( 'NONE',  ( -0.000000000000000000, -1.000000000000000000, -0.000000000000000000 ) ) ;
#54785 = ORIENTED_EDGE ( 'NONE', *, *, #36832, .T. ) ;
#54784 = AXIS2_PLACEMENT_3D ( 'NONE', #71101, #10858, #110376 ) ;
#54786 = CARTESIAN_POINT ( 'NONE',  ( 6.049999999999932321, 12.50000000000000000, -1.753560074763288679 ) ) ;
#54787 = CARTESIAN_POINT ( 'NONE',  ( -0.6500000000000394351, 2.500000000000000000, 2.411473670974873862 ) ) ;
#54788 = ORIENTED_EDGE ( 'NONE', *, *, #95656, .T. ) ;
#54789 = DIRECTION ( 'NONE',  ( 0.000000000000000000, 1.000000000000000000, 0.000000000000000000 ) ) ;
#54790 = DIRECTION ( 'NONE',  ( 0.000000000000000000, 0.000000000000000000, 1.000000000000000000 ) ) ;
#54791 = CARTESIAN_POINT ( 'NONE',  ( 5.649999999999932854, 2.500000000000000000, 2.511473670974873507 ) ) ;
#54792 = EDGE_CURVE ( 'NONE', #111183, #84285, #38420, .T. ) ;
#54794 = AXIS2_PLACEMENT_3D ( 'NONE', #84967, #7031, #54853 ) ;
#54793 = CARTESIAN_POINT ( 'NONE',  ( 9.799999999999915445, 2.500000000000000000, -4.676537180435977881 ) ) ;
#54795 = ORIENTED_EDGE ( 'NONE', *, *, #41031, .T. ) ;
#54796 = AXIS2_PLACEMENT_3D ( 'NONE', #1659, #10205, #2295 ) ;
#54797 = AXIS2_PLACEMENT_3D ( 'NONE', #8598, #48556, #79317 ) ;
#54798 = PLANE ( 'NONE',  #65446 ) ;
#54799 = AXIS2_PLACEMENT_3D ( 'NONE', #122778, #4264, #33749 ) ;
#54800 = DIRECTION ( 'NONE',  ( 0.000000000000000000, 0.000000000000000000, 1.000000000000000000 ) ) ;
#54801 = VERTEX_POINT ( 'NONE', #73268 ) ;
#54802 = ORIENTED_EDGE ( 'NONE', *, *, #107155, .T. ) ;
#54803 = CARTESIAN_POINT ( 'NONE',  ( 185.4635416670080872, -4.367472073101519747, 7.564683531249999149 ) ) ;
#54804 = DIRECTION ( 'NONE',  ( 0.000000000000000000, 1.000000000000000000, 0.000000000000000000 ) ) ;
#54805 = CARTESIAN_POINT ( 'NONE',  ( -10.20000000000000462, 2.500000000000000000, -4.676537180435973440 ) ) ;
#54806 = LINE ( 'NONE', #56098, #51118 ) ;
#54807 = DIRECTION ( 'NONE',  ( -4.274815082592931898E-19, -0.9999939076577903929, -0.003490651415223739937 ) ) ;
#54808 = CIRCLE ( 'NONE', #36043, 0.1000000000000000472 ) ;
#54810 = EDGE_CURVE ( 'NONE', #43068, #125419, #23826, .T. ) ;
#54809 = FACE_OUTER_BOUND ( 'NONE', #1360, .T. ) ;
#54811 = AXIS2_PLACEMENT_3D ( 'NONE', #47340, #85315, #55850 ) ;
#54812 = DIRECTION ( 'NONE',  ( -0.000000000000000000, -1.000000000000000000, -0.000000000000000000 ) ) ;
#54813 = CARTESIAN_POINT ( 'NONE',  ( -9.150000000000005684, 2.500000000000000000, 5.802370205355744659 ) ) ;
#54814 = CIRCLE ( 'NONE', #29782, 0.1000000000000002554 ) ;
#54815 = CARTESIAN_POINT ( 'NONE',  ( 8.949999999999919353, 2.500000000000000000, -6.148780366869526226 ) ) ;
#54816 = CIRCLE ( 'NONE', #25562, 0.5000000000000000000 ) ;
#54817 = LINE ( 'NONE', #43109, #85636 ) ;
#54818 = ORIENTED_EDGE ( 'NONE', *, *, #30090, .F. ) ;
#54819 = ORIENTED_EDGE ( 'NONE', *, *, #25639, .F. ) ;
#54820 = CONICAL_SURFACE ( 'NONE', #123868, 0.1000000000000002554, 0.003490658503988666988 ) ;
#54821 = ORIENTED_EDGE ( 'NONE', *, *, #120857, .T. ) ;
#54822 = ORIENTED_EDGE ( 'NONE', *, *, #8272, .F. ) ;
#54823 = EDGE_CURVE ( 'NONE', #46586, #43896, #122027, .T. ) ;
#54824 = CARTESIAN_POINT ( 'NONE',  ( 10.39999999999991154, 2.500000000000000000, 3.737306695894644371 ) ) ;
#54825 = DIRECTION ( 'NONE',  ( -0.000000000000000000, -1.000000000000000000, -0.000000000000000000 ) ) ;
#54826 = DIRECTION ( 'NONE',  ( 0.000000000000000000, 0.000000000000000000, -1.000000000000000000 ) ) ;
#54827 = ORIENTED_EDGE ( 'NONE', *, *, #97464, .T. ) ;
#54828 = CARTESIAN_POINT ( 'NONE',  ( -9.350000000000006750, 2.500000000000000000, -1.918653347947325782 ) ) ;
#54829 = CARTESIAN_POINT ( 'NONE',  ( -4.150000000000027889, 2.500000000000000000, -7.188010851410854052 ) ) ;
#54831 = EDGE_LOOP ( 'NONE', ( #91848, #30739 ) ) ;
#54830 = CARTESIAN_POINT ( 'NONE',  ( 9.999999999999914735, 2.500000000000000000, 0.7928203230275495672 ) ) ;
#54832 = CARTESIAN_POINT ( 'NONE',  ( 9.999999999999912959, 2.500000000000000000, 3.537306695894645081 ) ) ;
#54833 = ORIENTED_EDGE ( 'NONE', *, *, #12725, .T. ) ;
#54834 = VERTEX_POINT ( 'NONE', #2575 ) ;
#54835 = VERTEX_POINT ( 'NONE', #72639 ) ;
#54836 = CIRCLE ( 'NONE', #79893, 0.06509327318403741736 ) ;
#54837 = VERTEX_POINT ( 'NONE', #4495 ) ;
#54838 = CARTESIAN_POINT ( 'NONE',  ( -2.100000000000034284, 12.50000000000000000, -4.330127018922201643 ) ) ;
#54839 = AXIS2_PLACEMENT_3D ( 'NONE', #104705, #94901, #5219 ) ;
#54840 = FACE_OUTER_BOUND ( 'NONE', #25015, .T. ) ;
#54841 = LINE ( 'NONE', #35236, #65077 ) ;
#54842 = CARTESIAN_POINT ( 'NONE',  ( -5.650000000000023448, 2.500000000000000000, -6.148780366869526226 ) ) ;
#54843 = ORIENTED_EDGE ( 'NONE', *, *, #94665, .T. ) ;
#54844 = CIRCLE ( 'NONE', #44396, 0.1000000000000002554 ) ;
#54845 = EDGE_CURVE ( 'NONE', #67610, #50039, #96128, .T. ) ;
#54846 = LINE ( 'NONE', #55515, #14707 ) ;
#54848 = ORIENTED_EDGE ( 'NONE', *, *, #16120, .T. ) ;
#54847 = AXIS2_PLACEMENT_3D ( 'NONE', #104359, #25796, #64428 ) ;
#54849 = FACE_OUTER_BOUND ( 'NONE', #23456, .T. ) ;
#54850 = CARTESIAN_POINT ( 'NONE',  ( -0.2000000000000347888, 12.50000000000000000, 0.3464101615137758494 ) ) ;
#54851 = CONICAL_SURFACE ( 'NONE', #105027, 0.09999999999999982514, 0.003490658503988666988 ) ;
#54852 = DIRECTION ( 'NONE',  ( 0.000000000000000000, 1.000000000000000000, 0.000000000000000000 ) ) ;
#54853 = DIRECTION ( 'NONE',  ( 0.000000000000000000, 0.000000000000000000, 1.000000000000000000 ) ) ;
#54854 = CIRCLE ( 'NONE', #86148, 0.1000000000000002554 ) ;
#54855 = ADVANCED_FACE ( 'NONE', ( #3879 ), #61394, .T. ) ;
#54856 = ORIENTED_EDGE ( 'NONE', *, *, #114871, .T. ) ;
#54857 = VERTEX_POINT ( 'NONE', #74561 ) ;
#54858 = ORIENTED_EDGE ( 'NONE', *, *, #60972, .F. ) ;
#54859 = DIRECTION ( 'NONE',  ( 0.000000000000000000, 0.000000000000000000, 1.000000000000000000 ) ) ;
#54860 = CARTESIAN_POINT ( 'NONE',  ( -13.34999999999999076, 12.50000000000000000, 2.792790559304615616 ) ) ;
#54861 = EDGE_CURVE ( 'NONE', #9027, #126067, #24817, .T. ) ;
#54862 = ADVANCED_FACE ( 'NONE', ( #114479 ), #30104, .T. ) ;
#54863 = DIRECTION ( 'NONE',  ( -0.000000000000000000, -1.000000000000000000, -0.000000000000000000 ) ) ;
#54864 = EDGE_CURVE ( 'NONE', #115574, #24359, #92787, .T. ) ;
#54865 = FACE_BOUND ( 'NONE', #78429, .T. ) ;
#54866 = EDGE_CURVE ( 'NONE', #88265, #6869, #40573, .T. ) ;
#54867 = CARTESIAN_POINT ( 'NONE',  ( 1.849999999999950129, 12.50000000000000000, -6.841600689897078702 ) ) ;
#54868 = CARTESIAN_POINT ( 'NONE',  ( -9.800000000000007816, 2.500000000000000000, -3.983716857408421852 ) ) ;
#54869 = DIRECTION ( 'NONE',  ( 0.000000000000000000, 1.000000000000000000, 0.000000000000000000 ) ) ;
#54870 = AXIS2_PLACEMENT_3D ( 'NONE', #11546, #82238, #50841 ) ;
#54871 = EDGE_CURVE ( 'NONE', #51072, #98382, #19620, .T. ) ;
#54872 = CARTESIAN_POINT ( 'NONE',  ( 186.4635416670080872, -4.367472073101520635, 7.564683531249999149 ) ) ;
#54873 = EDGE_CURVE ( 'NONE', #109616, #58961, #93560, .T. ) ;
#54874 = CARTESIAN_POINT ( 'NONE',  ( 8.099999999999923261, 2.500000000000000000, 4.676537180435972552 ) ) ;
#54875 = EDGE_CURVE ( 'NONE', #67325, #114219, #15387, .T. ) ;
#54876 = CARTESIAN_POINT ( 'NONE',  ( -4.550000000000022915, 12.50000000000000000, -2.165063509461101710 ) ) ;
#54877 = EDGE_LOOP ( 'NONE', ( #106114, #98700 ) ) ;
#54878 = AXIS2_PLACEMENT_3D ( 'NONE', #99128, #98455, #8790 ) ;
#54879 = EDGE_CURVE ( 'NONE', #12234, #70177, #99042, .T. ) ;
#54880 = CIRCLE ( 'NONE', #25636, 0.06509327318403745899 ) ;
#54881 = EDGE_CURVE ( 'NONE', #73196, #61030, #88567, .T. ) ;
#54882 = DIRECTION ( 'NONE',  ( 0.000000000000000000, 0.000000000000000000, 1.000000000000000000 ) ) ;
#54883 = ORIENTED_EDGE ( 'NONE', *, *, #48116, .T. ) ;
#54884 = EDGE_LOOP ( 'NONE', ( #122187, #94170 ) ) ;
#54885 = VERTEX_POINT ( 'NONE', #45754 ) ;
#54886 = VERTEX_POINT ( 'NONE', #35922 ) ;
#54887 = DIRECTION ( 'NONE',  ( 0.000000000000000000, 1.000000000000000000, 0.000000000000000000 ) ) ;
#54888 = FACE_BOUND ( 'NONE', #102515, .T. ) ;
#54890 = EDGE_CURVE ( 'NONE', #2948, #29851, #25876, .T. ) ;
#54889 = AXIS2_PLACEMENT_3D ( 'NONE', #107011, #58591, #98484 ) ;
#54891 = DIRECTION ( 'NONE',  ( 0.000000000000000000, 0.000000000000000000, 1.000000000000000000 ) ) ;
#54892 = CIRCLE ( 'NONE', #52744, 0.06509327318403745899 ) ;
#54893 = CONICAL_SURFACE ( 'NONE', #75819, 0.1000000000000002554, 0.003490658503988666988 ) ;
#54894 = CIRCLE ( 'NONE', #38184, 0.09999999999999982514 ) ;
#54895 = ORIENTED_EDGE ( 'NONE', *, *, #89020, .T. ) ;
#54896 = CARTESIAN_POINT ( 'NONE',  ( 26.75237029038848391, 2.962322469582319151, 2.722363819593919931 ) ) ;
#54897 = DIRECTION ( 'NONE',  ( 0.000000000000000000, 1.000000000000000000, 0.000000000000000000 ) ) ;
#54898 = ORIENTED_EDGE ( 'NONE', *, *, #91472, .T. ) ;
#54900 = DIRECTION ( 'NONE',  ( 0.000000000000000000, 1.000000000000000000, 0.000000000000000000 ) ) ;
#54899 = CIRCLE ( 'NONE', #117574, 0.06509327318403745899 ) ;
#54901 = DIRECTION ( 'NONE',  ( 0.000000000000000000, 1.000000000000000000, 0.000000000000000000 ) ) ;
#54902 = VECTOR ( 'NONE', #128984, 1000.000000000000000 ) ;
#54903 = CIRCLE ( 'NONE', #94607, 0.06509327318403745899 ) ;
#54904 = AXIS2_PLACEMENT_3D ( 'NONE', #123682, #53043, #15664 ) ;
#54905 = CONICAL_SURFACE ( 'NONE', #128085, 0.09999999999999982514, 0.003490658503988666988 ) ;
#54906 = ORIENTED_EDGE ( 'NONE', *, *, #2797, .F. ) ;
#54907 = DIRECTION ( 'NONE',  ( -0.000000000000000000, -1.000000000000000000, -0.000000000000000000 ) ) ;
#54908 = DIRECTION ( 'NONE',  ( -4.274815082592931898E-19, -0.9999939076577903929, -0.003490651415223739937 ) ) ;
#54909 = EDGE_LOOP ( 'NONE', ( #62657, #49461, #36248, #73100 ) ) ;
#54910 = CARTESIAN_POINT ( 'NONE',  ( -3.550000000000028244, 2.500000000000000000, 2.411473670974873862 ) ) ;
#54911 = CIRCLE ( 'NONE', #627, 0.1000000000000000472 ) ;
#54912 = CARTESIAN_POINT ( 'NONE',  ( 6.649999999999929301, 2.500000000000000000, -2.165063509461101710 ) ) ;
#54913 = DIRECTION ( 'NONE',  ( -0.000000000000000000, -1.000000000000000000, -0.000000000000000000 ) ) ;
#54914 = ORIENTED_EDGE ( 'NONE', *, *, #15268, .T. ) ;
#54915 = ORIENTED_EDGE ( 'NONE', *, *, #124636, .F. ) ;
#54916 = DIRECTION ( 'NONE',  ( -0.000000000000000000, -1.000000000000000000, -0.000000000000000000 ) ) ;
#54917 = ORIENTED_EDGE ( 'NONE', *, *, #126105, .T. ) ;
#54918 = CARTESIAN_POINT ( 'NONE',  ( 10.59999999999990905, 12.50000000000000000, -4.048810130592463530 ) ) ;
#54919 = DIRECTION ( 'NONE',  ( 0.000000000000000000, 1.000000000000000000, 0.000000000000000000 ) ) ;
#54920 = EDGE_CURVE ( 'NONE', #16529, #95073, #11295, .T. ) ;
#54921 = VERTEX_POINT ( 'NONE', #105955 ) ;
#54923 = ADVANCED_FACE ( 'NONE', ( #14958 ), #46815, .T. ) ;
#54922 = CARTESIAN_POINT ( 'NONE',  ( 108.6749215142614275, 5.885800260617194191, -4.965357148327123937 ) ) ;
#54924 = FACE_OUTER_BOUND ( 'NONE', #66739, .T. ) ;
#54925 = PLANE ( 'NONE',  #17260 ) ;
#54926 = AXIS2_PLACEMENT_3D ( 'NONE', #91663, #111963, #92966 ) ;
#54927 = CARTESIAN_POINT ( 'NONE',  ( 12.89999999999990266, 12.50000000000000000, -3.637306695894650055 ) ) ;
#54928 = VECTOR ( 'NONE', #36667, 1000.000000000000000 ) ;
#54929 = LINE ( 'NONE', #35313, #59897 ) ;
#54930 = EDGE_CURVE ( 'NONE', #32336, #70678, #25436, .T. ) ;
#54931 = ORIENTED_EDGE ( 'NONE', *, *, #36495, .T. ) ;
#54932 = VERTEX_POINT ( 'NONE', #54910 ) ;
#54933 = CARTESIAN_POINT ( 'NONE',  ( 1.849999999999949019, 12.50000000000000000, 6.906693963081109722 ) ) ;
#54934 = EDGE_CURVE ( 'NONE', #25178, #13086, #64095, .T. ) ;
#54935 = AXIS2_PLACEMENT_3D ( 'NONE', #85477, #125405, #26565 ) ;
#54936 = LINE ( 'NONE', #64756, #114227 ) ;
#54937 = VECTOR ( 'NONE', #37247, 1000.000000000000000 ) ;
#54939 = CARTESIAN_POINT ( 'NONE',  ( -7.900000000000014566, 2.500000000000000000, 0.09999999999999772959 ) ) ;
#54938 = CIRCLE ( 'NONE', #128111, 0.1000000000000000472 ) ;
#54941 = ORIENTED_EDGE ( 'NONE', *, *, #20437, .F. ) ;
#54940 = ORIENTED_EDGE ( 'NONE', *, *, #36976, .F. ) ;
#54942 = ORIENTED_EDGE ( 'NONE', *, *, #108103, .T. ) ;
#54943 = CARTESIAN_POINT ( 'NONE',  ( -14.99999999999998401, 2.500000000000000000, 0.6928203230275518099 ) ) ;
#54944 = CARTESIAN_POINT ( 'NONE',  ( -1.450000000000035927, 2.500000000000000000, -6.148780366869526226 ) ) ;
#54945 = VECTOR ( 'NONE', #13131, 1000.000000000000000 ) ;
#54947 = DIRECTION ( 'NONE',  ( 0.000000000000000000, -0.9999939076577903929, 0.003490651415223739937 ) ) ;
#54946 = CIRCLE ( 'NONE', #57096, 0.1000000000000000472 ) ;
#54948 = AXIS2_PLACEMENT_3D ( 'NONE', #3637, #62576, #43587 ) ;
#54949 =( LENGTH_UNIT ( ) NAMED_UNIT ( * ) SI_UNIT ( .MILLI., .METRE. ) );
#54950 = CARTESIAN_POINT ( 'NONE',  ( 10.84999999999990905, 2.500000000000000000, 2.165063509461097713 ) ) ;
#54951 = DIRECTION ( 'NONE',  ( 0.000000000000000000, -0.9999939076577903929, 0.003490651415223739937 ) ) ;
#54952 = FACE_OUTER_BOUND ( 'NONE', #112440, .T. ) ;
#54953 = VECTOR ( 'NONE', #119320, 1000.000000000000000 ) ;
#54954 = LINE ( 'NONE', #43230, #1096 ) ;
#54955 = LINE ( 'NONE', #35333, #84362 ) ;
#54956 = CONICAL_SURFACE ( 'NONE', #86340, 0.09999999999999982514, 0.003490658503988666988 ) ;
#54957 = DIRECTION ( 'NONE',  ( 0.000000000000000000, 0.000000000000000000, -1.000000000000000000 ) ) ;
#54958 = AXIS2_PLACEMENT_3D ( 'NONE', #97962, #19393, #119530 ) ;
#54959 = VERTEX_POINT ( 'NONE', #94848 ) ;
#54960 = CARTESIAN_POINT ( 'NONE',  ( 13.29999999999989946, 12.50000000000000000, 0.06509327318403504425 ) ) ;
#54961 = EDGE_LOOP ( 'NONE', ( #25009, #43607 ) ) ;
#54962 = ORIENTED_EDGE ( 'NONE', *, *, #73783, .F. ) ;
#54963 = DIRECTION ( 'NONE',  ( 0.000000000000000000, 0.000000000000000000, -1.000000000000000000 ) ) ;
#54964 = CARTESIAN_POINT ( 'NONE',  ( 8.949999999999917577, 2.500000000000000000, -2.611473670974877592 ) ) ;
#54965 = FACE_OUTER_BOUND ( 'NONE', #40250, .T. ) ;
#54966 = CONICAL_SURFACE ( 'NONE', #128142, 0.1000000000000002554, 0.003490658503988666988 ) ;
#54967 = EDGE_CURVE ( 'NONE', #37345, #25872, #65583, .T. ) ;
#54968 = DIRECTION ( 'NONE',  ( 0.000000000000000000, 0.000000000000000000, 1.000000000000000000 ) ) ;
#54969 = CARTESIAN_POINT ( 'NONE',  ( 7.699999999999925571, 2.500000000000000000, -4.776537180435978414 ) ) ;
#54970 = DIRECTION ( 'NONE',  ( 0.000000000000000000, 0.000000000000000000, 1.000000000000000000 ) ) ;
#54971 = LINE ( 'NONE', #112620, #32182 ) ;
#54972 = VERTEX_POINT ( 'NONE', #44455 ) ;
#54973 = DIRECTION ( 'NONE',  ( 0.000000000000000000, 1.000000000000000000, 0.000000000000000000 ) ) ;
#54974 = CIRCLE ( 'NONE', #15243, 0.1000000000000002554 ) ;
#54975 = DIRECTION ( 'NONE',  ( 0.000000000000000000, 0.000000000000000000, 1.000000000000000000 ) ) ;
#54976 = ORIENTED_EDGE ( 'NONE', *, *, #50731, .F. ) ;
#54977 = AXIS2_PLACEMENT_3D ( 'NONE', #7240, #68753, #128350 ) ;
#54978 = ORIENTED_EDGE ( 'NONE', *, *, #37624, .F. ) ;
#54979 = EDGE_LOOP ( 'NONE', ( #64572, #88523 ) ) ;
#54980 = ADVANCED_FACE ( 'NONE', ( #124309 ), #85664, .T. ) ;
#54982 = EDGE_LOOP ( 'NONE', ( #118965, #5979 ) ) ;
#54981 = ADVANCED_FACE ( 'NONE', ( #8384 ), #4923, .T. ) ;
#54983 = AXIS2_PLACEMENT_3D ( 'NONE', #947, #4620, #43944 ) ;
#54984 = CARTESIAN_POINT ( 'NONE',  ( -5.000000000000024869, 2.500000000000000000, -5.022947341949754119 ) ) ;
#54985 = DIRECTION ( 'NONE',  ( 0.000000000000000000, 0.000000000000000000, 1.000000000000000000 ) ) ;
#54986 = AXIS2_PLACEMENT_3D ( 'NONE', #87635, #79762, #100054 ) ;
#54987 = AXIS2_PLACEMENT_3D ( 'NONE', #18378, #70066, #121093 ) ;
#54988 = CARTESIAN_POINT ( 'NONE',  ( 16.55763163376620994, 0.1615157349276458432, -6.093150851882356278 ) ) ;
#54989 = AXIS2_PLACEMENT_3D ( 'NONE', #40045, #79960, #120536 ) ;
#54990 = FACE_OUTER_BOUND ( 'NONE', #9733, .T. ) ;
#54991 = CARTESIAN_POINT ( 'NONE',  ( -3.550000000000028688, 2.500000000000000000, 6.941600689897073018 ) ) ;
#54992 = VERTEX_POINT ( 'NONE', #98692 ) ;
#54993 = DIRECTION ( 'NONE',  ( -0.000000000000000000, 1.000000000000000000, -0.000000000000000000 ) ) ;
#54994 = EDGE_CURVE ( 'NONE', #58972, #33187, #9688, .T. ) ;
#54995 = DIRECTION ( 'NONE',  ( 0.000000000000000000, 0.000000000000000000, -1.000000000000000000 ) ) ;
#54996 = AXIS2_PLACEMENT_3D ( 'NONE', #37818, #38489, #87551 ) ;
#54997 = LINE ( 'NONE', #54354, #60444 ) ;
#54998 = VERTEX_POINT ( 'NONE', #49633 ) ;
#54999 = AXIS2_PLACEMENT_3D ( 'NONE', #68653, #128239, #58838 ) ;
#55000 = AXIS2_PLACEMENT_3D ( 'NONE', #110480, #12268, #82966 ) ;
#55001 = ORIENTED_EDGE ( 'NONE', *, *, #64487, .T. ) ;
#55002 = ORIENTED_EDGE ( 'NONE', *, *, #17923, .F. ) ;
#55003 = CARTESIAN_POINT ( 'NONE',  ( -2.499999999999996003, 2.500000000000000000, -4.330127018922201643 ) ) ;
#55004 = CARTESIAN_POINT ( 'NONE',  ( 6.249999999999932498, 12.50000000000000000, -5.867463478539787225 ) ) ;
#55005 = CARTESIAN_POINT ( 'NONE',  ( -4.600000000000024514, 2.500000000000000000, -0.7928203230275543412 ) ) ;
#55006 = AXIS2_PLACEMENT_3D ( 'NONE', #27227, #76982, #30966 ) ;
#55007 = ORIENTED_EDGE ( 'NONE', *, *, #59462, .T. ) ;
#55008 = DIRECTION ( 'NONE',  ( 0.000000000000000000, 0.000000000000000000, -1.000000000000000000 ) ) ;
#55009 = DIRECTION ( 'NONE',  ( -0.000000000000000000, -1.000000000000000000, -0.000000000000000000 ) ) ;
#55010 = DIRECTION ( 'NONE',  ( 0.000000000000000000, 0.000000000000000000, 1.000000000000000000 ) ) ;
#55011 = DIRECTION ( 'NONE',  ( 0.000000000000000000, 0.000000000000000000, 1.000000000000000000 ) ) ;
#55012 = DIRECTION ( 'NONE',  ( 0.000000000000000000, 0.000000000000000000, 1.000000000000000000 ) ) ;
#55013 = ADVANCED_FACE ( 'NONE', ( #18206 ), #96977, .T. ) ;
#55014 = ORIENTED_EDGE ( 'NONE', *, *, #54307, .T. ) ;
#55015 = DIRECTION ( 'NONE',  ( 0.000000000000000000, 0.000000000000000000, 1.000000000000000000 ) ) ;
#55016 = ORIENTED_EDGE ( 'NONE', *, *, #61874, .F. ) ;
#55017 = ORIENTED_EDGE ( 'NONE', *, *, #60662, .F. ) ;
#55018 = ORIENTED_EDGE ( 'NONE', *, *, #102451, .T. ) ;
#55019 = CONICAL_SURFACE ( 'NONE', #46718, 0.09999999999999982514, 0.003490658503988666988 ) ;
#55020 = EDGE_CURVE ( 'NONE', #27555, #110342, #836, .T. ) ;
#55021 = DIRECTION ( 'NONE',  ( 0.000000000000000000, 1.000000000000000000, 0.000000000000000000 ) ) ;
#55022 = EDGE_CURVE ( 'NONE', #47693, #57040, #88214, .T. ) ;
#55023 = FACE_BOUND ( 'NONE', #69312, .T. ) ;
#55024 = ADVANCED_FACE ( 'NONE', ( #79716 ), #78118, .T. ) ;
#55025 = DIRECTION ( 'NONE',  ( -4.274815082592931898E-19, -0.9999939076577903929, -0.003490651415223739937 ) ) ;
#55026 = CARTESIAN_POINT ( 'NONE',  ( -5.600000000000020073, 2.500000000000000000, -0.2464101615137782308 ) ) ;
#55027 = FACE_OUTER_BOUND ( 'NONE', #47702, .T. ) ;
#55028 = CONICAL_SURFACE ( 'NONE', #15301, 0.1000000000000000472, 0.003490658503988666988 ) ;
#55029 = AXIS2_PLACEMENT_3D ( 'NONE', #74867, #28836, #117826 ) ;
#55030 = AXIS2_PLACEMENT_3D ( 'NONE', #62038, #41764, #113050 ) ;
#55031 = EDGE_CURVE ( 'NONE', #26852, #108534, #66657, .T. ) ;
#55032 = AXIS2_PLACEMENT_3D ( 'NONE', #95879, #6814, #114854 ) ;
#55033 = EDGE_CURVE ( 'NONE', #86633, #42165, #55221, .T. ) ;
#55034 = EDGE_LOOP ( 'NONE', ( #35873, #121960 ) ) ;
#55035 = CARTESIAN_POINT ( 'NONE',  ( -0.8500000000000390576, 12.50000000000000000, -2.230156782645139391 ) ) ;
#55036 = DIRECTION ( 'NONE',  ( -0.000000000000000000, 1.000000000000000000, -0.000000000000000000 ) ) ;
#55037 = EDGE_CURVE ( 'NONE', #122432, #115626, #128403, .T. ) ;
#55038 = CARTESIAN_POINT ( 'NONE',  ( 14.14999999999989555, 12.50000000000000000, 2.230156782645134950 ) ) ;
#55039 = CARTESIAN_POINT ( 'NONE',  ( -7.900000000000014566, 2.500000000000000000, -0.7928203230275542301 ) ) ;
#55040 = EDGE_LOOP ( 'NONE', ( #42943, #36800, #106329, #108032 ) ) ;
#55042 = CARTESIAN_POINT ( 'NONE',  ( 6.249999999999932498, 12.50000000000000000, 5.737276932171707422 ) ) ;
#55041 = AXIS2_PLACEMENT_3D ( 'NONE', #46464, #4581, #94278 ) ;
#55043 = AXIS2_PLACEMENT_3D ( 'NONE', #50590, #98394, #99712 ) ;
#55044 = CIRCLE ( 'NONE', #46639, 0.06509327318403745899 ) ;
#55045 = EDGE_CURVE ( 'NONE', #25337, #5713, #26751, .T. ) ;
#55046 = DIRECTION ( 'NONE',  ( 0.000000000000000000, 0.000000000000000000, 1.000000000000000000 ) ) ;
#55047 = AXIS2_PLACEMENT_3D ( 'NONE', #25980, #26615, #74434 ) ;
#55048 = ORIENTED_EDGE ( 'NONE', *, *, #69494, .T. ) ;
#55049 = CIRCLE ( 'NONE', #117725, 0.06509327318403745899 ) ;
#55050 = DIRECTION ( 'NONE',  ( 0.000000000000000000, 0.000000000000000000, 1.000000000000000000 ) ) ;
#55051 = ADVANCED_FACE ( 'NONE', ( #19501 ), #9029, .T. ) ;
#55052 = ORIENTED_EDGE ( 'NONE', *, *, #66318, .F. ) ;
#55053 = FACE_BOUND ( 'NONE', #63937, .T. ) ;
#55054 = EDGE_CURVE ( 'NONE', #88607, #95487, #68598, .T. ) ;
#55055 = AXIS2_PLACEMENT_3D ( 'NONE', #106193, #17789, #55795 ) ;
#55056 = CARTESIAN_POINT ( 'NONE',  ( 6.649999999999928413, 2.500000000000000000, 1.472243186433545459 ) ) ;
#55057 = VERTEX_POINT ( 'NONE', #18853 ) ;
#55058 = PLANE ( 'NONE',  #56848 ) ;
#55059 = CARTESIAN_POINT ( 'NONE',  ( 0.8499999999999527933, 12.50000000000000000, 7.253104124594885960 ) ) ;
#55060 = VERTEX_POINT ( 'NONE', #117679 ) ;
#55061 = EDGE_LOOP ( 'NONE', ( #102654, #109131 ) ) ;
#55062 = CARTESIAN_POINT ( 'NONE',  ( 186.2135416670080872, 4.367472073101518859, -7.564683531249999149 ) ) ;
#55064 = EDGE_LOOP ( 'NONE', ( #49775, #49942 ) ) ;
#55063 = AXIS2_PLACEMENT_3D ( 'NONE', #95126, #117296, #66926 ) ;
#55065 = DIRECTION ( 'NONE',  ( 0.000000000000000000, 1.000000000000000000, 0.000000000000000000 ) ) ;
#55066 = FACE_OUTER_BOUND ( 'NONE', #39946, .T. ) ;
#55067 = DIRECTION ( 'NONE',  ( -0.000000000000000000, -1.000000000000000000, -0.000000000000000000 ) ) ;
#55068 = PLANE ( 'NONE',  #21829 ) ;
#55069 = DIRECTION ( 'NONE',  ( 0.000000000000000000, 1.000000000000000000, 0.000000000000000000 ) ) ;
#55070 = CARTESIAN_POINT ( 'NONE',  ( 187.5000000000000000, 0.000000000000000000, 7.700000000000000178 ) ) ;
#55071 = CIRCLE ( 'NONE', #2841, 0.09999999999999999167 ) ;
#55072 = VECTOR ( 'NONE', #19818, 1000.000000000000000 ) ;
#55073 = VECTOR ( 'NONE', #108947, 1000.000000000000000 ) ;
#55074 = VERTEX_POINT ( 'NONE', #29344 ) ;
#55075 = ORIENTED_EDGE ( 'NONE', *, *, #86177, .F. ) ;
#55076 = DIRECTION ( 'NONE',  ( -0.000000000000000000, -1.000000000000000000, -0.000000000000000000 ) ) ;
#55077 = DIRECTION ( 'NONE',  ( 0.000000000000000000, -0.000000000000000000, 1.000000000000000000 ) ) ;
#55078 = DIRECTION ( 'NONE',  ( 0.000000000000000000, 1.000000000000000000, 0.000000000000000000 ) ) ;
#55079 = CARTESIAN_POINT ( 'NONE',  ( -10.40000000000000391, 2.500000000000000000, -3.537306695894645969 ) ) ;
#55081 = ORIENTED_EDGE ( 'NONE', *, *, #83503, .F. ) ;
#55080 = ORIENTED_EDGE ( 'NONE', *, *, #67559, .F. ) ;
#55082 = FACE_BOUND ( 'NONE', #121450, .T. ) ;
#55083 = EDGE_LOOP ( 'NONE', ( #111847, #51320 ) ) ;
#55084 = CIRCLE ( 'NONE', #46675, 0.06509327318403745899 ) ;
#55085 = LINE ( 'NONE', #46537, #47136 ) ;
#55086 = CARTESIAN_POINT ( 'NONE',  ( 129.5000000000000000, -1.375000000000002665, -7.576237522675752345 ) ) ;
#55087 = CIRCLE ( 'NONE', #75915, 0.06509327318403745899 ) ;
#55088 = ORIENTED_EDGE ( 'NONE', *, *, #51523, .F. ) ;
#55090 = DIRECTION ( 'NONE',  ( 0.000000000000000000, -0.9999939076577903929, 0.003490651415223739937 ) ) ;
#55089 = AXIS2_PLACEMENT_3D ( 'NONE', #110628, #28862, #20961 ) ;
#55091 = DIRECTION ( 'NONE',  ( 0.000000000000000000, 1.000000000000000000, 0.000000000000000000 ) ) ;
#55092 = EDGE_CURVE ( 'NONE', #64400, #31027, #13436, .T. ) ;
#55093 = DIRECTION ( 'NONE',  ( 1.000000000000000000, 0.000000000000000000, 0.000000000000000000 ) ) ;
#55094 = DIRECTION ( 'NONE',  ( 0.000000000000000000, 0.000000000000000000, 1.000000000000000000 ) ) ;
#55096 = EDGE_CURVE ( 'NONE', #104138, #9737, #32258, .T. ) ;
#55095 = FACE_OUTER_BOUND ( 'NONE', #13176, .T. ) ;
#55097 = CARTESIAN_POINT ( 'NONE',  ( -3.350000000000028511, 2.500000000000000000, -2.857883832488653741 ) ) ;
#55098 = CARTESIAN_POINT ( 'NONE',  ( 186.8177083336747160, 4.367472073101515306, 7.564683531250000925 ) ) ;
#55099 = CARTESIAN_POINT ( 'NONE',  ( -5.400000000000023448, 12.50000000000000000, -4.330127018922201643 ) ) ;
#55100 = CIRCLE ( 'NONE', #97146, 0.1000000000000002554 ) ;
#55101 = DIRECTION ( 'NONE',  ( 0.000000000000000000, -0.000000000000000000, 1.000000000000000000 ) ) ;
#55102 = ORIENTED_EDGE ( 'NONE', *, *, #90846, .F. ) ;
#55103 = ORIENTED_EDGE ( 'NONE', *, *, #114606, .T. ) ;
#55104 = CARTESIAN_POINT ( 'NONE',  ( -8.950000000000006395, 2.500000000000000000, 6.841600689897072485 ) ) ;
#55106 = ORIENTED_EDGE ( 'NONE', *, *, #108527, .T. ) ;
#55105 = CIRCLE ( 'NONE', #115630, 0.06509327318403745899 ) ;
#55107 = AXIS2_PLACEMENT_3D ( 'NONE', #36957, #115484, #124033 ) ;
#55108 = AXIS2_PLACEMENT_3D ( 'NONE', #105165, #94066, #55432 ) ;
#55109 = DIRECTION ( 'NONE',  ( 0.000000000000000000, -0.9999939076577903929, 0.003490651415223739937 ) ) ;
#55111 = ORIENTED_EDGE ( 'NONE', *, *, #10716, .F. ) ;
#55110 = VERTEX_POINT ( 'NONE', #7742 ) ;
#55112 = ORIENTED_EDGE ( 'NONE', *, *, #57091, .T. ) ;
#55113 = AXIS2_PLACEMENT_3D ( 'NONE', #118171, #88716, #18030 ) ;
#55114 = CARTESIAN_POINT ( 'NONE',  ( -15.39999999999997904, 2.500000000000000000, -0.6928203230275519209 ) ) ;
#55115 = CIRCLE ( 'NONE', #32146, 0.06509327318403745899 ) ;
#55116 = CARTESIAN_POINT ( 'NONE',  ( -12.49999999999999289, 2.500000000000000000, 3.637306695894644726 ) ) ;
#55117 = CARTESIAN_POINT ( 'NONE',  ( 186.8333333333333144, 6.668395609140177704, -3.849999999999998312 ) ) ;
#55118 = LINE ( 'NONE', #95046, #70980 ) ;
#55119 = DIRECTION ( 'NONE',  ( 0.000000000000000000, 0.000000000000000000, 1.000000000000000000 ) ) ;
#55120 = VERTEX_POINT ( 'NONE', #47689 ) ;
#55121 = CARTESIAN_POINT ( 'NONE',  ( -5.400000000000023448, 2.500000000000000000, -4.330127018922201643 ) ) ;
#55122 = ORIENTED_EDGE ( 'NONE', *, *, #88516, .T. ) ;
#55123 = VERTEX_POINT ( 'NONE', #87589 ) ;
#55124 = ORIENTED_EDGE ( 'NONE', *, *, #57985, .T. ) ;
#55125 = CARTESIAN_POINT ( 'NONE',  ( -9.600000000000006750, 2.500000000000000000, -0.5928203230275542746 ) ) ;
#55126 = AXIS2_PLACEMENT_3D ( 'NONE', #88937, #30029, #128888 ) ;
#55127 = VECTOR ( 'NONE', #43836, 1000.000000000000000 ) ;
#55128 = EDGE_LOOP ( 'NONE', ( #26975, #85874, #6380, #104310 ) ) ;
#55129 = VERTEX_POINT ( 'NONE', #28044 ) ;
#55130 = ORIENTED_EDGE ( 'NONE', *, *, #81842, .F. ) ;
#55131 = EDGE_CURVE ( 'NONE', #65795, #124333, #99369, .T. ) ;
#55133 = DIRECTION ( 'NONE',  ( -0.000000000000000000, 1.000000000000000000, -0.000000000000000000 ) ) ;
#55132 = VECTOR ( 'NONE', #21884, 1000.000000000000000 ) ;
#55134 = DIRECTION ( 'NONE',  ( -0.000000000000000000, -1.000000000000000000, -0.000000000000000000 ) ) ;
#55136 = CARTESIAN_POINT ( 'NONE',  ( -3.150000000000029221, 2.500000000000000000, 2.511473670974873507 ) ) ;
#55135 = AXIS2_PLACEMENT_3D ( 'NONE', #74545, #35909, #126877 ) ;
#55137 = DIRECTION ( 'NONE',  ( 0.000000000000000000, 0.000000000000000000, -1.000000000000000000 ) ) ;
#55138 = AXIS2_PLACEMENT_3D ( 'NONE', #56056, #63963, #35790 ) ;
#55139 = CIRCLE ( 'NONE', #109420, 0.1000000000000000472 ) ;
#55140 = FACE_OUTER_BOUND ( 'NONE', #24445, .T. ) ;
#55141 = EDGE_LOOP ( 'NONE', ( #6160, #55915 ) ) ;
#55142 = CARTESIAN_POINT ( 'NONE',  ( 5.849999999999935696, 12.50000000000000000, -6.430097255199264339 ) ) ;
#55143 = EDGE_CURVE ( 'NONE', #26619, #93332, #59444, .T. ) ;
#55144 = AXIS2_PLACEMENT_3D ( 'NONE', #7183, #18300, #27460 ) ;
#55146 = ORIENTED_EDGE ( 'NONE', *, *, #12456, .T. ) ;
#55145 = AXIS2_PLACEMENT_3D ( 'NONE', #74117, #23077, #92450 ) ;
#55147 = DIRECTION ( 'NONE',  ( 0.000000000000000000, 0.000000000000000000, 1.000000000000000000 ) ) ;
#55148 = CIRCLE ( 'NONE', #107365, 0.06509327318403745899 ) ;
#55149 = ORIENTED_EDGE ( 'NONE', *, *, #93254, .F. ) ;
#55150 = DIRECTION ( 'NONE',  ( -0.000000000000000000, 1.000000000000000000, -0.000000000000000000 ) ) ;
#55151 = ORIENTED_EDGE ( 'NONE', *, *, #60088, .F. ) ;
#55152 = EDGE_CURVE ( 'NONE', #19955, #24096, #53174, .T. ) ;
#55153 = EDGE_CURVE ( 'NONE', #59948, #124302, #69887, .T. ) ;
#55154 = VERTEX_POINT ( 'NONE', #119627 ) ;
#55155 = CARTESIAN_POINT ( 'NONE',  ( 12.29999999999990123, 2.500000000000000000, 0.4464101615137735513 ) ) ;
#55156 = CARTESIAN_POINT ( 'NONE',  ( 8.099999999999923261, 2.500000000000000000, -4.083716857408426826 ) ) ;
#55157 = ADVANCED_FACE ( 'NONE', ( #2422 ), #17641, .T. ) ;
#55158 = CARTESIAN_POINT ( 'NONE',  ( 9.999999999999916511, 12.50000000000000000, -0.7579135962115916003 ) ) ;
#55159 = CARTESIAN_POINT ( 'NONE',  ( -4.400000000000025224, 2.500000000000000000, -0.2464101615137783419 ) ) ;
#55160 = ORIENTED_EDGE ( 'NONE', *, *, #110458, .F. ) ;
#55161 =( BOUNDED_CURVE ( )  B_SPLINE_CURVE ( 2, ( #72104, #112666, #22366, #92363, #71428, #62286, #64194 ),
 .UNSPECIFIED., .F., .F. ) 
 B_SPLINE_CURVE_WITH_KNOTS ( ( 3, 2, 2, 3 ),
 ( 0.07142857142857149400, 0.09523809523809532995, 0.1190476190476191520, 0.1428571428571429880 ),
 .UNSPECIFIED. ) 
 CURVE ( )  GEOMETRIC_REPRESENTATION_ITEM ( )  RATIONAL_B_SPLINE_CURVE ( ( 0.9999999999999996669, 0.8660254037844390407, 1.000000000000000000, 0.8660254037844387076, 1.000000000000000000, 0.8660254037844379305, 1.000000000000000666 ) ) 
 REPRESENTATION_ITEM ( '' )  );
#55162 = CARTESIAN_POINT ( 'NONE',  ( 12.29999999999990123, 2.500000000000000000, 0.3464101615137735735 ) ) ;
#55163 = PLANE ( 'NONE',  #22257 ) ;
#55164 = ADVANCED_FACE ( 'NONE', ( #21436 ), #120063, .T. ) ;
#55165 = CARTESIAN_POINT ( 'NONE',  ( -3.150000000000029221, 2.500000000000000000, -1.818653347947326138 ) ) ;
#55166 = DIRECTION ( 'NONE',  ( 0.000000000000000000, -0.000000000000000000, 1.000000000000000000 ) ) ;
#55167 = VECTOR ( 'NONE', #13157, 1000.000000000000000 ) ;
#55168 = CARTESIAN_POINT ( 'NONE',  ( -10.40000000000000213, 12.50000000000000000, 4.330127018922196314 ) ) ;
#55169 = VERTEX_POINT ( 'NONE', #42380 ) ;
#55170 = ORIENTED_EDGE ( 'NONE', *, *, #102178, .F. ) ;
#55171 = CIRCLE ( 'NONE', #21426, 0.06509327318403745899 ) ;
#55172 = EDGE_LOOP ( 'NONE', ( #101242, #76948 ) ) ;
#55173 = FACE_OUTER_BOUND ( 'NONE', #62640, .T. ) ;
#55174 = CARTESIAN_POINT ( 'NONE',  ( -1.450000000000036371, 2.500000000000000000, 2.611473670974873151 ) ) ;
#55175 = AXIS2_PLACEMENT_3D ( 'NONE', #2704, #32844, #123763 ) ;
#55176 = CARTESIAN_POINT ( 'NONE',  ( 185.1718750003414016, 9.264065473108010111E-16, -7.564683531250000925 ) ) ;
#55177 = CARTESIAN_POINT ( 'NONE',  ( -9.800000000000006040, 2.500000000000000000, 0.3464101615137735735 ) ) ;
#55178 = DIRECTION ( 'NONE',  ( -0.000000000000000000, 1.000000000000000000, -0.000000000000000000 ) ) ;
#55179 = CARTESIAN_POINT ( 'NONE',  ( -3.100000000000028955, 2.500000000000000000, 4.676537180435972552 ) ) ;
#55180 = AXIS2_PLACEMENT_3D ( 'NONE', #58123, #108490, #28008 ) ;
#55181 = LINE ( 'NONE', #57105, #80991 ) ;
#55182 = ORIENTED_EDGE ( 'NONE', *, *, #68646, .F. ) ;
#55183 = CONICAL_SURFACE ( 'NONE', #2956, 0.1000000000000000472, 0.003490658503988666988 ) ;
#55184 = CONICAL_SURFACE ( 'NONE', #103205, 0.1000000000000002554, 0.003490658503988666988 ) ;
#55185 = EDGE_CURVE ( 'NONE', #128715, #88410, #126325, .T. ) ;
#55186 = DIRECTION ( 'NONE',  ( 0.000000000000000000, 0.000000000000000000, 1.000000000000000000 ) ) ;
#55187 = CARTESIAN_POINT ( 'NONE',  ( -4.150000000000025224, 12.50000000000000000, 7.188010851410848723 ) ) ;
#55188 = ORIENTED_EDGE ( 'NONE', *, *, #29183, .F. ) ;
#55189 = EDGE_CURVE ( 'NONE', #65093, #115124, #76145, .T. ) ;
#55190 = CARTESIAN_POINT ( 'NONE',  ( -2.050000000000032685, 2.500000000000000000, -6.595190528383302109 ) ) ;
#55191 = DIRECTION ( 'NONE',  ( 0.000000000000000000, 0.000000000000000000, -1.000000000000000000 ) ) ;
#55192 = EDGE_CURVE ( 'NONE', #90854, #108142, #122126, .T. ) ;
#55193 = CARTESIAN_POINT ( 'NONE',  ( 87.50000000000001421, 1.034826545279513461E-15, 8.199999999999999289 ) ) ;
#55194 = VERTEX_POINT ( 'NONE', #51561 ) ;
#55195 = VECTOR ( 'NONE', #44088, 1000.000000000000000 ) ;
#55196 = CIRCLE ( 'NONE', #32229, 0.06509327318403745899 ) ;
#55197 = AXIS2_PLACEMENT_3D ( 'NONE', #110951, #59976, #80883 ) ;
#55198 = DIRECTION ( 'NONE',  ( 0.000000000000000000, 0.000000000000000000, 1.000000000000000000 ) ) ;
#55199 = ADVANCED_FACE ( 'NONE', ( #120926 ), #51122, .T. ) ;
#55200 = ADVANCED_FACE ( 'NONE', ( #1155 ), #21781, .T. ) ;
#55202 = ORIENTED_EDGE ( 'NONE', *, *, #126707, .T. ) ;
#55201 = VECTOR ( 'NONE', #74233, 1000.000000000000000 ) ;
#55203 = CARTESIAN_POINT ( 'NONE',  ( -6.650000000000015454, 2.500000000000000000, 7.288010851410849256 ) ) ;
#55204 = DIRECTION ( 'NONE',  ( 0.000000000000000000, 0.000000000000000000, 1.000000000000000000 ) ) ;
#55205 = EDGE_CURVE ( 'NONE', #114757, #4060, #9249, .T. ) ;
#55206 = CARTESIAN_POINT ( 'NONE',  ( -10.85000000000000142, 2.500000000000000000, -2.857883832488649745 ) ) ;
#55207 = ADVANCED_FACE ( 'NONE', ( #100009 ), #44857, .T. ) ;
#55208 = CIRCLE ( 'NONE', #57347, 0.06509327318403745899 ) ;
#55209 = ORIENTED_EDGE ( 'NONE', *, *, #8376, .F. ) ;
#55210 = DIRECTION ( 'NONE',  ( 0.000000000000000000, 0.000000000000000000, 1.000000000000000000 ) ) ;
#55211 = EDGE_CURVE ( 'NONE', #2148, #115931, #62670, .T. ) ;
#55212 = DIRECTION ( 'NONE',  ( 0.000000000000000000, 0.000000000000000000, 1.000000000000000000 ) ) ;
#55213 = VERTEX_POINT ( 'NONE', #91467 ) ;
#55214 = ADVANCED_FACE ( 'NONE', ( #101941 ), #61493, .T. ) ;
#55215 = CARTESIAN_POINT ( 'NONE',  ( 4.149999999999941735, 2.500000000000000000, -2.757883832488654097 ) ) ;
#55216 = EDGE_LOOP ( 'NONE', ( #35134, #103063, #12324, #107233 ) ) ;
#55217 = ORIENTED_EDGE ( 'NONE', *, *, #22094, .T. ) ;
#55218 = DIRECTION ( 'NONE',  ( 0.000000000000000000, -0.000000000000000000, 1.000000000000000000 ) ) ;
#55219 = DIRECTION ( 'NONE',  ( 0.000000000000000000, 0.000000000000000000, 1.000000000000000000 ) ) ;
#55220 = VECTOR ( 'NONE', #33272, 1000.000000000000000 ) ;
#55221 = CIRCLE ( 'NONE', #44759, 0.06509327318403745899 ) ;
#55222 = ORIENTED_EDGE ( 'NONE', *, *, #127023, .F. ) ;
#55223 = CARTESIAN_POINT ( 'NONE',  ( 8.149999999999920419, 12.50000000000000000, 6.906693963081109722 ) ) ;
#55224 = DIRECTION ( 'NONE',  ( 0.000000000000000000, -0.000000000000000000, 1.000000000000000000 ) ) ;
#55225 = ORIENTED_EDGE ( 'NONE', *, *, #7825, .T. ) ;
#55226 = DIRECTION ( 'NONE',  ( 0.000000000000000000, 0.000000000000000000, -1.000000000000000000 ) ) ;
#55228 = FACE_OUTER_BOUND ( 'NONE', #33075, .T. ) ;
#55227 = CIRCLE ( 'NONE', #128408, 0.06509327318403745899 ) ;
#55229 = AXIS2_PLACEMENT_3D ( 'NONE', #12652, #21199, #92514 ) ;
#55230 = AXIS2_PLACEMENT_3D ( 'NONE', #129354, #97926, #69759 ) ;
#55231 = CARTESIAN_POINT ( 'NONE',  ( 6.699999999999930012, 12.50000000000000000, -4.330127018922201643 ) ) ;
#55232 = CARTESIAN_POINT ( 'NONE',  ( -6.050000000000022027, 12.50000000000000000, -1.753560074763288679 ) ) ;
#55233 = DIRECTION ( 'NONE',  ( 0.000000000000000000, -0.9999939076577903929, 0.003490651415223739937 ) ) ;
#55234 = DIRECTION ( 'NONE',  ( 0.000000000000000000, 1.000000000000000000, 0.000000000000000000 ) ) ;
#55235 = AXIS2_PLACEMENT_3D ( 'NONE', #51493, #69831, #11545 ) ;
#55236 = CIRCLE ( 'NONE', #111758, 0.1000000000000002554 ) ;
#55237 = CONICAL_SURFACE ( 'NONE', #117917, 0.1000000000000002554, 0.003490658503988666988 ) ;
#55238 = ORIENTED_EDGE ( 'NONE', *, *, #106417, .T. ) ;
#55239 = EDGE_LOOP ( 'NONE', ( #105250, #18392, #70336, #75907 ) ) ;
#55240 = VERTEX_POINT ( 'NONE', #1784 ) ;
#55241 = EDGE_LOOP ( 'NONE', ( #28530, #50011, #71948, #22106 ) ) ;
#55242 = PLANE ( 'NONE',  #95488 ) ;
#55243 = CARTESIAN_POINT ( 'NONE',  ( -8.950000000000011724, 2.500000000000000000, -6.248780366869521430 ) ) ;
#55244 = LINE ( 'NONE', #115406, #34285 ) ;
#55245 = ORIENTED_EDGE ( 'NONE', *, *, #64808, .F. ) ;
#55246 = FACE_BOUND ( 'NONE', #91449, .T. ) ;
#55247 = FACE_OUTER_BOUND ( 'NONE', #46321, .T. ) ;
#55248 = DIRECTION ( 'NONE',  ( 0.000000000000000000, 0.000000000000000000, 1.000000000000000000 ) ) ;
#55249 = CARTESIAN_POINT ( 'NONE',  ( -1.250000000000037526, 2.500000000000000000, -5.802370205355749988 ) ) ;
#55250 = EDGE_CURVE ( 'NONE', #32033, #120581, #81645, .T. ) ;
#55251 = DIRECTION ( 'NONE',  ( -0.000000000000000000, -1.000000000000000000, -0.000000000000000000 ) ) ;
#55252 = DIRECTION ( 'NONE',  ( 0.05223670945016245515, 0.9986347311133432214, 0.000000000000000000 ) ) ;
#55253 = CARTESIAN_POINT ( 'NONE',  ( 9.149999999999916866, 12.50000000000000000, -1.472243186433550122 ) ) ;
#55254 = DIRECTION ( 'NONE',  ( 0.000000000000000000, 0.000000000000000000, 1.000000000000000000 ) ) ;
#55255 = DIRECTION ( 'NONE',  ( -0.000000000000000000, -1.000000000000000000, -0.000000000000000000 ) ) ;
#55256 = DIRECTION ( 'NONE',  ( 0.000000000000000000, 0.000000000000000000, -1.000000000000000000 ) ) ;
#55257 = CIRCLE ( 'NONE', #21818, 0.06509327318403745899 ) ;
#55258 = CARTESIAN_POINT ( 'NONE',  ( 7.299999999999927880, 2.500000000000000000, 3.983716857408420964 ) ) ;
#55259 = EDGE_CURVE ( 'NONE', #93988, #84759, #30194, .T. ) ;
#55260 = ORIENTED_EDGE ( 'NONE', *, *, #37784, .T. ) ;
#55261 = ORIENTED_EDGE ( 'NONE', *, *, #59530, .F. ) ;
#55262 = ORIENTED_EDGE ( 'NONE', *, *, #4356, .F. ) ;
#55263 = VERTEX_POINT ( 'NONE', #80377 ) ;
#55264 = DIRECTION ( 'NONE',  ( 0.000000000000000000, 0.000000000000000000, 1.000000000000000000 ) ) ;
#55265 = ORIENTED_EDGE ( 'NONE', *, *, #116326, .F. ) ;
#55266 = DIRECTION ( 'NONE',  ( 0.000000000000000000, 0.000000000000000000, -1.000000000000000000 ) ) ;
#55267 = ORIENTED_EDGE ( 'NONE', *, *, #14852, .F. ) ;
#55268 = VERTEX_POINT ( 'NONE', #71180 ) ;
#55269 = DIRECTION ( 'NONE',  ( 0.000000000000000000, 0.000000000000000000, 1.000000000000000000 ) ) ;
#55270 = AXIS2_PLACEMENT_3D ( 'NONE', #3087, #92088, #93394 ) ;
#55271 = AXIS2_PLACEMENT_3D ( 'NONE', #21566, #101417, #22227 ) ;
#55272 = LINE ( 'NONE', #115447, #112425 ) ;
#55273 = CARTESIAN_POINT ( 'NONE',  ( -2.950000000000029932, 12.50000000000000000, 2.165063509461097713 ) ) ;
#55274 = DIRECTION ( 'NONE',  ( -0.000000000000000000, -1.000000000000000000, -0.000000000000000000 ) ) ;
#55275 = CARTESIAN_POINT ( 'NONE',  ( 11.64999999999990443, 2.500000000000000000, -5.802370205355749988 ) ) ;
#55276 = ORIENTED_EDGE ( 'NONE', *, *, #58072, .F. ) ;
#55277 = ORIENTED_EDGE ( 'NONE', *, *, #64270, .T. ) ;
#55278 = AXIS2_PLACEMENT_3D ( 'NONE', #101721, #39600, #40217 ) ;
#55279 = EDGE_LOOP ( 'NONE', ( #8800, #41833 ) ) ;
#55281 = ORIENTED_EDGE ( 'NONE', *, *, #26495, .F. ) ;
#55280 = CARTESIAN_POINT ( 'NONE',  ( 11.84999999999990372, 2.500000000000000000, 2.411473670974873862 ) ) ;
#55282 = DIRECTION ( 'NONE',  ( 0.000000000000000000, 0.000000000000000000, 1.000000000000000000 ) ) ;
#55283 = ORIENTED_EDGE ( 'NONE', *, *, #24547, .T. ) ;
#55284 = VERTEX_POINT ( 'NONE', #120294 ) ;
#55285 = FACE_OUTER_BOUND ( 'NONE', #104149, .T. ) ;
#55287 = CIRCLE ( 'NONE', #128462, 0.06509327318403745899 ) ;
#55286 = DIRECTION ( 'NONE',  ( 0.000000000000000000, 1.000000000000000000, 0.000000000000000000 ) ) ;
#55288 = DIRECTION ( 'NONE',  ( 0.000000000000000000, 0.000000000000000000, 1.000000000000000000 ) ) ;
#55289 = AXIS2_PLACEMENT_3D ( 'NONE', #25944, #65851, #64562 ) ;
#55290 = CARTESIAN_POINT ( 'NONE',  ( -0.4000000000000392131, 12.50000000000000000, -4.957854068765716882 ) ) ;
#55291 = CARTESIAN_POINT ( 'NONE',  ( 1.849999999999948130, 12.50000000000000000, 6.148780366869520009 ) ) ;
#55292 = CIRCLE ( 'NONE', #107514, 0.1000000000000002554 ) ;
#55293 = ORIENTED_EDGE ( 'NONE', *, *, #53248, .F. ) ;
#55294 = CIRCLE ( 'NONE', #28194, 0.06509327318403745899 ) ;
#55295 = CARTESIAN_POINT ( 'NONE',  ( 6.849999999999930367, 2.500000000000000000, -6.941600689897078347 ) ) ;
#55296 = ADVANCED_FACE ( 'NONE', ( #70537 ), #113806, .T. ) ;
#55297 = ORIENTED_EDGE ( 'NONE', *, *, #34209, .T. ) ;
#55298 = DIRECTION ( 'NONE',  ( 0.000000000000000000, -0.9999939076577903929, 0.003490651415223739937 ) ) ;
#55299 = ORIENTED_EDGE ( 'NONE', *, *, #111522, .T. ) ;
#55300 = CARTESIAN_POINT ( 'NONE',  ( 184.5000000000000000, 0.000000000000000000, -7.699999999999999289 ) ) ;
#55301 = DIRECTION ( 'NONE',  ( -0.000000000000000000, -1.000000000000000000, -0.000000000000000000 ) ) ;
#55302 = ORIENTED_EDGE ( 'NONE', *, *, #73326, .T. ) ;
#55304 = EDGE_CURVE ( 'NONE', #10784, #126618, #73749, .T. ) ;
#55303 = DIRECTION ( 'NONE',  ( 0.000000000000000000, 0.000000000000000000, 1.000000000000000000 ) ) ;
#55305 = DIRECTION ( 'NONE',  ( 0.000000000000000000, 0.000000000000000000, -1.000000000000000000 ) ) ;
#55306 = EDGE_CURVE ( 'NONE', #112093, #56250, #80360, .T. ) ;
#55307 = ORIENTED_EDGE ( 'NONE', *, *, #90621, .T. ) ;
#55308 = CONICAL_SURFACE ( 'NONE', #63908, 0.1000000000000002554, 0.003490658503988666988 ) ;
#55309 = EDGE_CURVE ( 'NONE', #123444, #124385, #3729, .T. ) ;
#55311 = FACE_OUTER_BOUND ( 'NONE', #9931, .T. ) ;
#55310 = VECTOR ( 'NONE', #67857, 1000.000000000000000 ) ;
#55312 = ORIENTED_EDGE ( 'NONE', *, *, #87597, .T. ) ;
#55313 = ORIENTED_EDGE ( 'NONE', *, *, #49920, .T. ) ;
#55314 = VECTOR ( 'NONE', #114845, 1000.000000000000000 ) ;
#55315 = CIRCLE ( 'NONE', #30285, 0.1000000000000002554 ) ;
#55316 = ORIENTED_EDGE ( 'NONE', *, *, #38690, .T. ) ;
#55317 = FACE_OUTER_BOUND ( 'NONE', #22873, .T. ) ;
#55318 = DIRECTION ( 'NONE',  ( 0.000000000000000000, 0.000000000000000000, -1.000000000000000000 ) ) ;
#55319 = EDGE_CURVE ( 'NONE', #77958, #9996, #929, .T. ) ;
#55320 = CARTESIAN_POINT ( 'NONE',  ( 185.1927083336747160, 6.551208109652275624, -3.782341765624998686 ) ) ;
#55321 = CARTESIAN_POINT ( 'NONE',  ( 10.39999999999991154, 2.500000000000000000, 5.022947341949748790 ) ) ;
#55322 = CONICAL_SURFACE ( 'NONE', #80368, 0.1000000000000002554, 0.003490658503988666988 ) ;
#55323 = DIRECTION ( 'NONE',  ( 0.000000000000000000, 1.000000000000000000, 0.000000000000000000 ) ) ;
#55324 = CIRCLE ( 'NONE', #34694, 0.06509327318403745899 ) ;
#55325 = AXIS2_PLACEMENT_3D ( 'NONE', #34911, #6054, #15883 ) ;
#55326 = LINE ( 'NONE', #115503, #79991 ) ;
#55327 = AXIS2_PLACEMENT_3D ( 'NONE', #128927, #16962, #116482 ) ;
#55328 = ORIENTED_EDGE ( 'NONE', *, *, #48330, .T. ) ;
#55329 = AXIS2_PLACEMENT_3D ( 'NONE', #120348, #81069, #91525 ) ;
#55330 = CARTESIAN_POINT ( 'NONE',  ( -0.6000000000000388356, 2.500000000000000000, 4.083716857408421497 ) ) ;
#55331 = VECTOR ( 'NONE', #13682, 1000.000000000000000 ) ;
#55332 = ORIENTED_EDGE ( 'NONE', *, *, #68678, .T. ) ;
#55333 = CIRCLE ( 'NONE', #61605, 0.09999999999999982514 ) ;
#55334 = CARTESIAN_POINT ( 'NONE',  ( -2.300000000000033573, 2.500000000000000000, 4.576537180435972019 ) ) ;
#55335 = CARTESIAN_POINT ( 'NONE',  ( 154.1524742528378056, 2.500000000000000000, -1.703575533167231537 ) ) ;
#55336 = LINE ( 'NONE', #35697, #100283 ) ;
#55337 = VERTEX_POINT ( 'NONE', #83596 ) ;
#55338 = DIRECTION ( 'NONE',  ( -0.000000000000000000, -1.000000000000000000, -0.000000000000000000 ) ) ;
#55339 = CARTESIAN_POINT ( 'NONE',  ( -7.050000000000016698, 2.500000000000000000, -2.165063509461101710 ) ) ;
#55340 = AXIS2_PLACEMENT_3D ( 'NONE', #76081, #45986, #16487 ) ;
#55341 = EDGE_LOOP ( 'NONE', ( #104984, #104030, #76347, #4469 ) ) ;
#55342 = DIRECTION ( 'NONE',  ( 0.000000000000000000, -0.000000000000000000, 1.000000000000000000 ) ) ;
#55343 = EDGE_LOOP ( 'NONE', ( #92169, #66750 ) ) ;
#55344 = EDGE_LOOP ( 'NONE', ( #93819, #111095, #125102, #35653 ) ) ;
#55345 = LINE ( 'NONE', #104442, #50833 ) ;
#55346 = EDGE_CURVE ( 'NONE', #81635, #92156, #74093, .T. ) ;
#55347 = ADVANCED_FACE ( 'NONE', ( #5650 ), #25979, .T. ) ;
#55348 = ORIENTED_EDGE ( 'NONE', *, *, #109686, .T. ) ;
#55349 = CARTESIAN_POINT ( 'NONE',  ( 17.34645602450336810, 0.4686430837608600575, -5.377443133677279441 ) ) ;
#55351 = ADVANCED_FACE ( 'NONE', ( #63950 ), #15581, .T. ) ;
#55350 = LINE ( 'NONE', #95913, #83961 ) ;
#55352 = DIRECTION ( 'NONE',  ( -0.000000000000000000, -1.000000000000000000, -0.000000000000000000 ) ) ;
#55353 = CIRCLE ( 'NONE', #120203, 7.500000000000000000 ) ;
#55354 = VERTEX_POINT ( 'NONE', #24670 ) ;
#55355 = FACE_BOUND ( 'NONE', #119302, .T. ) ;
#55356 = ADVANCED_FACE ( 'NONE', ( #44296 ), #101378, .T. ) ;
#55358 = ORIENTED_EDGE ( 'NONE', *, *, #77091, .T. ) ;
#55357 = DIRECTION ( 'NONE',  ( 0.000000000000000000, 0.000000000000000000, -1.000000000000000000 ) ) ;
#55359 = CARTESIAN_POINT ( 'NONE',  ( 12.09999999999990195, 2.500000000000000000, 0.5928203230275495006 ) ) ;
#55360 = DIRECTION ( 'NONE',  ( 0.000000000000000000, 0.000000000000000000, 1.000000000000000000 ) ) ;
#55361 = ORIENTED_EDGE ( 'NONE', *, *, #103795, .T. ) ;
#55362 = ADVANCED_FACE ( 'NONE', ( #122874 ), #88759, .T. ) ;
#55363 = CIRCLE ( 'NONE', #7220, 0.06509327318403745899 ) ;
#55364 = EDGE_CURVE ( 'NONE', #37337, #92847, #103875, .T. ) ;
#55365 = VERTEX_POINT ( 'NONE', #33217 ) ;
#55366 = AXIS2_PLACEMENT_3D ( 'NONE', #124301, #104016, #74549 ) ;
#55367 = EDGE_LOOP ( 'NONE', ( #178, #8710, #86000, #109555 ) ) ;
#55368 = FACE_OUTER_BOUND ( 'NONE', #118560, .T. ) ;
#55369 = DIRECTION ( 'NONE',  ( -0.000000000000000000, 1.000000000000000000, -0.000000000000000000 ) ) ;
#55370 = CARTESIAN_POINT ( 'NONE',  ( 7.499999999999961808, 12.50000000000000000, 4.330127018922196314 ) ) ;
#55371 = FACE_BOUND ( 'NONE', #105215, .T. ) ;
#55372 = ORIENTED_EDGE ( 'NONE', *, *, #99248, .T. ) ;
#55373 = CARTESIAN_POINT ( 'NONE',  ( 186.2760416670080588, 6.551208109652274736, 3.782341765625001351 ) ) ;
#55374 = ADVANCED_FACE ( 'NONE', ( #115607 ), #125441, .T. ) ;
#55375 = DIRECTION ( 'NONE',  ( 0.000000000000000000, 0.000000000000000000, 1.000000000000000000 ) ) ;
#55376 = CARTESIAN_POINT ( 'NONE',  ( -8.350000000000010303, 2.500000000000000000, 6.495190528383297135 ) ) ;
#55378 = AXIS2_PLACEMENT_3D ( 'NONE', #104467, #2545, #42517 ) ;
#55377 = CARTESIAN_POINT ( 'NONE',  ( -12.89999999999999325, 2.500000000000000000, 0.5928203230275536084 ) ) ;
#55379 = CONICAL_SURFACE ( 'NONE', #49137, 0.1000000000000002554, 0.003490658503988666988 ) ;
#55380 = CARTESIAN_POINT ( 'NONE',  ( 4.349999999999938360, 2.500000000000000000, 1.718653347947321386 ) ) ;
#55381 = CARTESIAN_POINT ( 'NONE',  ( -8.300000000000009592, 12.50000000000000000, 4.330127018922196314 ) ) ;
#55382 = FACE_OUTER_BOUND ( 'NONE', #2925, .T. ) ;
#55383 = CARTESIAN_POINT ( 'NONE',  ( 2.949999999999945111, 12.50000000000000000, 2.230156782645134950 ) ) ;
#55384 = AXIS2_PLACEMENT_3D ( 'NONE', #50087, #955, #292 ) ;
#55385 = CARTESIAN_POINT ( 'NONE',  ( 5.199999999999931788, 2.500000000000000000, 4.776537180435972196 ) ) ;
#55386 = ORIENTED_EDGE ( 'NONE', *, *, #45128, .F. ) ;
#55387 = ORIENTED_EDGE ( 'NONE', *, *, #7424, .T. ) ;
#55388 = EDGE_LOOP ( 'NONE', ( #8360, #49520, #67590, #122372 ) ) ;
#55389 = VERTEX_POINT ( 'NONE', #124151 ) ;
#55390 = ORIENTED_EDGE ( 'NONE', *, *, #30393, .T. ) ;
#55391 = CARTESIAN_POINT ( 'NONE',  ( 179.5000000000000000, 0.6250000000000000000, 7.634788798650556707 ) ) ;
#55392 = CARTESIAN_POINT ( 'NONE',  ( 3.349999999999945466, 2.500000000000000000, -6.495190528383302464 ) ) ;
#55393 = EDGE_LOOP ( 'NONE', ( #92172, #66396, #91955, #90737 ) ) ;
#55394 = FACE_BOUND ( 'NONE', #101482, .T. ) ;
#55395 = DIRECTION ( 'NONE',  ( 0.000000000000000000, 0.000000000000000000, 1.000000000000000000 ) ) ;
#55396 = CIRCLE ( 'NONE', #34483, 0.1000000000000002554 ) ;
#55397 = DIRECTION ( 'NONE',  ( 0.000000000000000000, 0.000000000000000000, 1.000000000000000000 ) ) ;
#55398 = CIRCLE ( 'NONE', #116031, 0.09999999999999982514 ) ;
#55399 = ORIENTED_EDGE ( 'NONE', *, *, #54265, .F. ) ;
#55400 = AXIS2_PLACEMENT_3D ( 'NONE', #120462, #119173, #57687 ) ;
#55401 = CARTESIAN_POINT ( 'NONE',  ( -6.850000000000017408, 2.500000000000000000, -2.411473670974877859 ) ) ;
#55402 = DIRECTION ( 'NONE',  ( 0.000000000000000000, 0.000000000000000000, 1.000000000000000000 ) ) ;
#55403 = FACE_OUTER_BOUND ( 'NONE', #69421, .T. ) ;
#55404 = ORIENTED_EDGE ( 'NONE', *, *, #58573, .T. ) ;
#55405 = DIRECTION ( 'NONE',  ( -0.000000000000000000, -1.000000000000000000, -0.000000000000000000 ) ) ;
#55406 = AXIS2_PLACEMENT_3D ( 'NONE', #10670, #31013, #80742 ) ;
#55407 = VERTEX_POINT ( 'NONE', #74414 ) ;
#55408 = ADVANCED_FACE ( 'NONE', ( #94686 ), #65874, .T. ) ;
#55409 = CIRCLE ( 'NONE', #5218, 0.06509327318403745899 ) ;
#55410 = ORIENTED_EDGE ( 'NONE', *, *, #17003, .T. ) ;
#55411 = ORIENTED_EDGE ( 'NONE', *, *, #42339, .F. ) ;
#55412 = CARTESIAN_POINT ( 'NONE',  ( -1.850000000000033396, 2.500000000000000000, -6.941600689897077459 ) ) ;
#55413 = AXIS2_PLACEMENT_3D ( 'NONE', #66590, #86873, #26676 ) ;
#55414 = CARTESIAN_POINT ( 'NONE',  ( 1.249999999999988898, 2.500000000000000000, -6.395190528383301931 ) ) ;
#55415 = CARTESIAN_POINT ( 'NONE',  ( -7.499999999999980460, 2.500000000000000000, 0.09999999999999772959 ) ) ;
#55416 = EDGE_LOOP ( 'NONE', ( #105192, #124522 ) ) ;
#55417 = CARTESIAN_POINT ( 'NONE',  ( 15.23091471424993060, 1.499999999999968026, -7.179421170830202925 ) ) ;
#55418 = VECTOR ( 'NONE', #73174, 1000.000000000000000 ) ;
#55419 = CIRCLE ( 'NONE', #93078, 3.000000000000000000 ) ;
#55420 = DIRECTION ( 'NONE',  ( 0.000000000000000000, -0.9999939076577903929, 0.003490651415223739937 ) ) ;
#55421 = CARTESIAN_POINT ( 'NONE',  ( 2.899999999999945732, 2.500000000000000000, -4.330127018922201643 ) ) ;
#55422 = CARTESIAN_POINT ( 'NONE',  ( 184.9062500006828031, -8.891194145520236347, -1.633285867636356693E-15 ) ) ;
#55424 = AXIS2_PLACEMENT_3D ( 'NONE', #104256, #76086, #56430 ) ;
#55423 = DIRECTION ( 'NONE',  ( -0.000000000000000000, -1.000000000000000000, -0.000000000000000000 ) ) ;
#55425 = CARTESIAN_POINT ( 'NONE',  ( -8.300000000000011369, 12.50000000000000000, -2.276824562219559311E-15 ) ) ;
#55426 = ORIENTED_EDGE ( 'NONE', *, *, #108817, .T. ) ;
#55427 = DIRECTION ( 'NONE',  ( 0.000000000000000000, 0.000000000000000000, 1.000000000000000000 ) ) ;
#55428 = VERTEX_POINT ( 'NONE', #14811 ) ;
#55429 = ORIENTED_EDGE ( 'NONE', *, *, #86352, .T. ) ;
#55430 = DIRECTION ( 'NONE',  ( -0.000000000000000000, -1.000000000000000000, -0.000000000000000000 ) ) ;
#55431 = DIRECTION ( 'NONE',  ( 0.000000000000000000, 0.000000000000000000, 1.000000000000000000 ) ) ;
#55432 = DIRECTION ( 'NONE',  ( 0.000000000000000000, 0.000000000000000000, -1.000000000000000000 ) ) ;
#55433 = DIRECTION ( 'NONE',  ( -0.000000000000000000, 1.000000000000000000, -0.000000000000000000 ) ) ;
#55434 = ORIENTED_EDGE ( 'NONE', *, *, #104282, .F. ) ;
#55435 = EDGE_LOOP ( 'NONE', ( #42854, #97130 ) ) ;
#55436 = CARTESIAN_POINT ( 'NONE',  ( 0.6499999999999561684, 2.500000000000000000, -1.918653347947325782 ) ) ;
#55437 = CARTESIAN_POINT ( 'NONE',  ( 65.38824919562647153, 3.824345297732404614, -5.305607913327973435 ) ) ;
#55438 = LINE ( 'NONE', #4372, #87830 ) ;
#55439 = VERTEX_POINT ( 'NONE', #82951 ) ;
#55440 = EDGE_LOOP ( 'NONE', ( #45216, #29417, #104440, #116744 ) ) ;
#55441 = CARTESIAN_POINT ( 'NONE',  ( 14.59999999999989484, 2.500000000000000000, 0.6928203230275494784 ) ) ;
#55442 = CIRCLE ( 'NONE', #118226, 0.1000000000000002554 ) ;
#55443 = CONICAL_SURFACE ( 'NONE', #105623, 0.1000000000000000472, 0.003490658503988666988 ) ;
#55444 = VERTEX_POINT ( 'NONE', #54751 ) ;
#55446 = CONICAL_SURFACE ( 'NONE', #34630, 0.1000000000000002554, 0.003490658503988666988 ) ;
#55445 = DIRECTION ( 'NONE',  ( 0.000000000000000000, 0.000000000000000000, 1.000000000000000000 ) ) ;
#55447 = EDGE_CURVE ( 'NONE', #14963, #72759, #35152, .T. ) ;
#55448 = DIRECTION ( 'NONE',  ( -0.000000000000000000, -1.000000000000000000, -0.000000000000000000 ) ) ;
#55449 = VERTEX_POINT ( 'NONE', #114960 ) ;
#55450 = FACE_OUTER_BOUND ( 'NONE', #118997, .T. ) ;
#55451 = DIRECTION ( 'NONE',  ( -0.000000000000000000, -1.000000000000000000, -0.000000000000000000 ) ) ;
#55452 = CARTESIAN_POINT ( 'NONE',  ( -8.100000000000013856, 12.50000000000000000, -0.3464101615137782364 ) ) ;
#55453 = ADVANCED_FACE ( 'NONE', ( #54125 ), #25286, .T. ) ;
#55454 = PLANE ( 'NONE',  #75099 ) ;
#55455 = EDGE_CURVE ( 'NONE', #26527, #93988, #53492, .T. ) ;
#55456 = EDGE_LOOP ( 'NONE', ( #62490, #37567, #70692, #117843 ) ) ;
#55457 = CIRCLE ( 'NONE', #126565, 0.06509327318403743123 ) ;
#55458 = CARTESIAN_POINT ( 'NONE',  ( -12.89999999999999147, 2.500000000000000000, 3.537306695894645081 ) ) ;
#55460 = AXIS2_PLACEMENT_3D ( 'NONE', #72629, #101438, #121709 ) ;
#55459 = CARTESIAN_POINT ( 'NONE',  ( -7.700000000000016165, 2.500000000000000000, 0.3464101615137735735 ) ) ;
#55461 = EDGE_CURVE ( 'NONE', #79663, #118275, #84647, .T. ) ;
#55462 = ORIENTED_EDGE ( 'NONE', *, *, #3658, .F. ) ;
#55463 = EDGE_CURVE ( 'NONE', #47559, #45160, #92972, .T. ) ;
#55464 = ORIENTED_EDGE ( 'NONE', *, *, #34704, .T. ) ;
#55465 = ADVANCED_FACE ( 'NONE', ( #128703 ), #99233, .T. ) ;
#55466 = CARTESIAN_POINT ( 'NONE',  ( 185.3385416670080872, 6.551208109652274736, 3.782341765625001351 ) ) ;
#55468 = EDGE_CURVE ( 'NONE', #127925, #31177, #113900, .T. ) ;
#55467 = DIRECTION ( 'NONE',  ( 0.000000000000000000, 0.000000000000000000, -1.000000000000000000 ) ) ;
#55469 = DIRECTION ( 'NONE',  ( 0.000000000000000000, 0.000000000000000000, -1.000000000000000000 ) ) ;
#55470 = EDGE_CURVE ( 'NONE', #59296, #70566, #8870, .T. ) ;
#55471 = DIRECTION ( 'NONE',  ( -4.274815082592931898E-19, -0.9999939076577903929, -0.003490651415223739937 ) ) ;
#55472 = CARTESIAN_POINT ( 'NONE',  ( -8.100000000000010303, 2.500000000000000000, 3.983716857408420964 ) ) ;
#55473 = PLANE ( 'NONE',  #96615 ) ;
#55474 = AXIS2_PLACEMENT_3D ( 'NONE', #37029, #76951, #27194 ) ;
#55475 = AXIS2_PLACEMENT_3D ( 'NONE', #88560, #89850, #87267 ) ;
#55476 = DIRECTION ( 'NONE',  ( 0.000000000000000000, -0.000000000000000000, 1.000000000000000000 ) ) ;
#55477 = DIRECTION ( 'NONE',  ( 0.000000000000000000, 0.000000000000000000, 1.000000000000000000 ) ) ;
#55478 = DIRECTION ( 'NONE',  ( 0.000000000000000000, -0.9999939076577903929, 0.003490651415223739937 ) ) ;
#55479 = CARTESIAN_POINT ( 'NONE',  ( -11.89999999999999680, 2.500000000000000000, 0.4464101615137776591 ) ) ;
#55480 = EDGE_CURVE ( 'NONE', #79987, #8533, #55315, .T. ) ;
#55481 = CARTESIAN_POINT ( 'NONE',  ( -14.14999999999998614, 12.50000000000000000, 1.472243186433549456 ) ) ;
#55482 = ORIENTED_EDGE ( 'NONE', *, *, #12471, .F. ) ;
#55484 = ORIENTED_EDGE ( 'NONE', *, *, #25923, .F. ) ;
#55483 = CIRCLE ( 'NONE', #117270, 0.06509327318403745899 ) ;
#55485 = ORIENTED_EDGE ( 'NONE', *, *, #37727, .T. ) ;
#55486 = DIRECTION ( 'NONE',  ( 0.000000000000000000, 1.000000000000000000, 0.000000000000000000 ) ) ;
#55487 = CONICAL_SURFACE ( 'NONE', #3167, 0.09999999999999982514, 0.003490658503988666988 ) ;
#55488 = DIRECTION ( 'NONE',  ( 1.000000000000000000, -0.000000000000000000, -0.000000000000000000 ) ) ;
#55489 = ORIENTED_EDGE ( 'NONE', *, *, #22407, .F. ) ;
#55490 = CARTESIAN_POINT ( 'NONE',  ( 12.04999999999990834, 2.500000000000000000, 6.395190528383296602 ) ) ;
#55491 = CIRCLE ( 'NONE', #116027, 0.06509327318403745899 ) ;
#55492 = AXIS2_PLACEMENT_3D ( 'NONE', #52576, #91221, #2836 ) ;
#55493 = DIRECTION ( 'NONE',  ( -0.000000000000000000, -1.000000000000000000, -0.000000000000000000 ) ) ;
#55495 = VERTEX_POINT ( 'NONE', #97908 ) ;
#55494 = DIRECTION ( 'NONE',  ( 0.000000000000000000, 1.000000000000000000, 0.000000000000000000 ) ) ;
#55496 = CARTESIAN_POINT ( 'NONE',  ( -1.850000000000033840, 2.500000000000000000, 6.148780366869520897 ) ) ;
#55497 = ORIENTED_EDGE ( 'NONE', *, *, #110861, .T. ) ;
#55498 = AXIS2_PLACEMENT_3D ( 'NONE', #5380, #23752, #25032 ) ;
#55499 = AXIS2_PLACEMENT_3D ( 'NONE', #27380, #38541, #79097 ) ;
#55500 = CIRCLE ( 'NONE', #128692, 0.06509327318403745899 ) ;
#55501 = ORIENTED_EDGE ( 'NONE', *, *, #62715, .T. ) ;
#55502 = VERTEX_POINT ( 'NONE', #76988 ) ;
#55503 = EDGE_LOOP ( 'NONE', ( #54340, #89335, #104421, #100317 ) ) ;
#55504 = CARTESIAN_POINT ( 'NONE',  ( 7.099999999999928590, 2.500000000000000000, -4.922947341949753586 ) ) ;
#55505 = CIRCLE ( 'NONE', #5309, 0.06509327318403745899 ) ;
#55506 = EDGE_CURVE ( 'NONE', #4351, #111323, #7263, .T. ) ;
#55507 = CARTESIAN_POINT ( 'NONE',  ( 7.499999999999925393, 12.50000000000000000, 5.088040615133786027 ) ) ;
#55509 = EDGE_CURVE ( 'NONE', #20474, #68081, #38608, .T. ) ;
#55508 = CARTESIAN_POINT ( 'NONE',  ( -1.050000000000038680, 12.50000000000000000, 6.776507416713035248 ) ) ;
#55510 = DIRECTION ( 'NONE',  ( -0.000000000000000000, 1.000000000000000000, -0.000000000000000000 ) ) ;
#55511 = CIRCLE ( 'NONE', #95224, 7.500000000000000000 ) ;
#55512 = VERTEX_POINT ( 'NONE', #36443 ) ;
#55513 = EDGE_CURVE ( 'NONE', #114128, #120638, #19338, .T. ) ;
#55514 = AXIS2_PLACEMENT_3D ( 'NONE', #4692, #124511, #44654 ) ;
#55516 = CONICAL_SURFACE ( 'NONE', #63923, 0.1000000000000002554, 0.003490658503988666988 ) ;
#55515 = CARTESIAN_POINT ( 'NONE',  ( -1.650000000000034328, 2.500000000000000000, -2.065063509461102065 ) ) ;
#55517 = VERTEX_POINT ( 'NONE', #128020 ) ;
#55518 = DIRECTION ( 'NONE',  ( 0.000000000000000000, 0.000000000000000000, 1.000000000000000000 ) ) ;
#55519 = CARTESIAN_POINT ( 'NONE',  ( 15.23091471425135701, -1.500000000000127898, -7.179421170829354715 ) ) ;
#55520 = FACE_OUTER_BOUND ( 'NONE', #8966, .T. ) ;
#55521 = CARTESIAN_POINT ( 'NONE',  ( 15.05551045036142455, -2.483581587658090672, 4.666934263335505761 ) ) ;
#55522 = EDGE_CURVE ( 'NONE', #7922, #111183, #76352, .T. ) ;
#55523 = ADVANCED_FACE ( 'NONE', ( #47536 ), #80455, .T. ) ;
#55524 = ORIENTED_EDGE ( 'NONE', *, *, #41174, .F. ) ;
#55525 = EDGE_CURVE ( 'NONE', #50160, #6072, #120154, .T. ) ;
#55526 = EDGE_CURVE ( 'NONE', #23165, #5682, #26602, .T. ) ;
#55527 = VERTEX_POINT ( 'NONE', #69090 ) ;
#55528 = ORIENTED_EDGE ( 'NONE', *, *, #26388, .F. ) ;
#55529 = CARTESIAN_POINT ( 'NONE',  ( -7.900000000000014566, 2.500000000000000000, -5.122947341949753763 ) ) ;
#55530 = FACE_OUTER_BOUND ( 'NONE', #41991, .T. ) ;
#55531 = LINE ( 'NONE', #45074, #27339 ) ;
#55532 = FACE_BOUND ( 'NONE', #57665, .T. ) ;
#55533 = DIRECTION ( 'NONE',  ( 0.000000000000000000, 0.000000000000000000, 1.000000000000000000 ) ) ;
#55534 = VECTOR ( 'NONE', #70055, 1000.000000000000000 ) ;
#55535 = CARTESIAN_POINT ( 'NONE',  ( -3.950000000000026379, 2.500000000000000000, 6.841600689897072485 ) ) ;
#55536 = EDGE_CURVE ( 'NONE', #45787, #109690, #97165, .T. ) ;
#55537 = DIRECTION ( 'NONE',  ( 0.000000000000000000, 1.000000000000000000, 0.000000000000000000 ) ) ;
#55538 = CARTESIAN_POINT ( 'NONE',  ( -1.450000000000035483, 2.500000000000000000, 6.148780366869520897 ) ) ;
#55539 = DIRECTION ( 'NONE',  ( 0.000000000000000000, -0.000000000000000000, -1.000000000000000000 ) ) ;
#55540 = AXIS2_PLACEMENT_3D ( 'NONE', #19673, #90318, #30797 ) ;
#55541 = CARTESIAN_POINT ( 'NONE',  ( -5.850000000000021849, 12.50000000000000000, -1.472243186433550122 ) ) ;
#55542 = DIRECTION ( 'NONE',  ( -0.000000000000000000, -1.000000000000000000, -0.000000000000000000 ) ) ;
#55543 = AXIS2_PLACEMENT_3D ( 'NONE', #27081, #4190, #64418 ) ;
#55544 = CARTESIAN_POINT ( 'NONE',  ( 10.64999999999991331, 2.500000000000000000, 6.841600689897072485 ) ) ;
#55545 = AXIS2_PLACEMENT_3D ( 'NONE', #109461, #40747, #20436 ) ;
#55546 = ORIENTED_EDGE ( 'NONE', *, *, #8777, .F. ) ;
#55547 = ORIENTED_EDGE ( 'NONE', *, *, #13194, .F. ) ;
#55548 = EDGE_LOOP ( 'NONE', ( #84462, #20338 ) ) ;
#55549 = VERTEX_POINT ( 'NONE', #107074 ) ;
#55550 = DIRECTION ( 'NONE',  ( 0.000000000000000000, -0.9999939076577903929, 0.003490651415223739937 ) ) ;
#55551 = EDGE_CURVE ( 'NONE', #97470, #46758, #61587, .T. ) ;
#55552 = FACE_BOUND ( 'NONE', #109631, .T. ) ;
#55553 = DIRECTION ( 'NONE',  ( 0.000000000000000000, 1.000000000000000000, 0.000000000000000000 ) ) ;
#55554 = CIRCLE ( 'NONE', #109935, 0.09999999999999999167 ) ;
#55555 = CIRCLE ( 'NONE', #53408, 0.09999999999999982514 ) ;
#55556 = ORIENTED_EDGE ( 'NONE', *, *, #15042, .T. ) ;
#55557 = DIRECTION ( 'NONE',  ( 0.000000000000000000, 0.000000000000000000, 1.000000000000000000 ) ) ;
#55558 = DIRECTION ( 'NONE',  ( 0.000000000000000000, 0.000000000000000000, 1.000000000000000000 ) ) ;
#55559 = ORIENTED_EDGE ( 'NONE', *, *, #11487, .F. ) ;
#55560 = FACE_OUTER_BOUND ( 'NONE', #5039, .T. ) ;
#55561 = FACE_OUTER_BOUND ( 'NONE', #7167, .T. ) ;
#55562 = CIRCLE ( 'NONE', #57623, 0.06509327318403745899 ) ;
#55563 = AXIS2_PLACEMENT_3D ( 'NONE', #45279, #43995, #24346 ) ;
#55564 = ADVANCED_FACE ( 'NONE', ( #37076 ), #67913, .T. ) ;
#55565 = ORIENTED_EDGE ( 'NONE', *, *, #60978, .T. ) ;
#55566 = CARTESIAN_POINT ( 'NONE',  ( 13.34999999999990017, 2.500000000000000000, 2.857883832488649301 ) ) ;
#55567 = DIRECTION ( 'NONE',  ( 0.000000000000000000, -0.9999939076577903929, 0.003490651415223739937 ) ) ;
#55568 = VERTEX_POINT ( 'NONE', #37713 ) ;
#55569 = CARTESIAN_POINT ( 'NONE',  ( 4.149999999999938183, 2.500000000000000000, 2.165063509461097713 ) ) ;
#55570 = DIRECTION ( 'NONE',  ( -0.000000000000000000, -1.000000000000000000, -0.000000000000000000 ) ) ;
#55571 = LINE ( 'NONE', #7093, #66072 ) ;
#55572 = ORIENTED_EDGE ( 'NONE', *, *, #110172, .T. ) ;
#55573 = EDGE_LOOP ( 'NONE', ( #67208, #64032 ) ) ;
#55574 = ADVANCED_FACE ( 'NONE', ( #18704 ), #98536, .T. ) ;
#55575 = DIRECTION ( 'NONE',  ( 1.000000000000000000, 0.000000000000000000, 0.000000000000000000 ) ) ;
#55576 = ORIENTED_EDGE ( 'NONE', *, *, #61293, .F. ) ;
#55577 = DIRECTION ( 'NONE',  ( 0.000000000000000000, 0.000000000000000000, 1.000000000000000000 ) ) ;
#55578 = CARTESIAN_POINT ( 'NONE',  ( -3.750000000000027534, 2.500000000000000000, 2.857883832488649301 ) ) ;
#55579 = AXIS2_PLACEMENT_3D ( 'NONE', #122694, #94514, #44792 ) ;
#55580 = VERTEX_POINT ( 'NONE', #88743 ) ;
#55581 = VECTOR ( 'NONE', #64964, 1000.000000000000000 ) ;
#55582 = CARTESIAN_POINT ( 'NONE',  ( 162.5000000000000000, 0.5000000000000000000, -7.500000000000005329 ) ) ;
#55583 = DIRECTION ( 'NONE',  ( 0.000000000000000000, 0.000000000000000000, 1.000000000000000000 ) ) ;
#55584 = DIRECTION ( 'NONE',  ( 0.000000000000000000, 0.000000000000000000, 1.000000000000000000 ) ) ;
#55585 = CARTESIAN_POINT ( 'NONE',  ( 8.949999999999917577, 2.500000000000000000, 6.148780366869520009 ) ) ;
#55586 = DIRECTION ( 'NONE',  ( -4.274815082592931898E-19, -0.9999939076577903929, -0.003490651415223739937 ) ) ;
#55587 = FACE_OUTER_BOUND ( 'NONE', #114258, .T. ) ;
#55588 = EDGE_LOOP ( 'NONE', ( #123425, #90404, #42534, #5139 ) ) ;
#55589 = EDGE_LOOP ( 'NONE', ( #14290, #74837 ) ) ;
#55590 = DIRECTION ( 'NONE',  ( -4.274815082592931898E-19, -0.9999939076577903929, -0.003490651415223739937 ) ) ;
#55591 = DIRECTION ( 'NONE',  ( -0.000000000000000000, 1.000000000000000000, -0.000000000000000000 ) ) ;
#55592 = DIRECTION ( 'NONE',  ( 0.000000000000000000, 0.000000000000000000, 1.000000000000000000 ) ) ;
#55594 = VERTEX_POINT ( 'NONE', #49484 ) ;
#55593 = EDGE_LOOP ( 'NONE', ( #6341, #97199, #108709, #16990 ) ) ;
#55595 = ORIENTED_EDGE ( 'NONE', *, *, #65269, .F. ) ;
#55596 = CARTESIAN_POINT ( 'NONE',  ( -6.850000000000017408, 12.50000000000000000, -2.576566944158915184 ) ) ;
#55597 = AXIS2_PLACEMENT_3D ( 'NONE', #29715, #31035, #12004 ) ;
#55598 = CARTESIAN_POINT ( 'NONE',  ( 4.149999999999941735, 2.500000000000000000, -7.188010851410854052 ) ) ;
#55599 = CARTESIAN_POINT ( 'NONE',  ( 2.699999999999946443, 2.500000000000000000, 0.4464101615137735513 ) ) ;
#55600 = EDGE_CURVE ( 'NONE', #93321, #90179, #123208, .T. ) ;
#55601 = DIRECTION ( 'NONE',  ( 0.000000000000000000, 1.000000000000000000, 0.000000000000000000 ) ) ;
#55602 = CARTESIAN_POINT ( 'NONE',  ( -12.49999999999995914, 12.50000000000000000, 1.843143693225357538E-15 ) ) ;
#55603 = DIRECTION ( 'NONE',  ( -0.000000000000000000, -1.000000000000000000, -0.000000000000000000 ) ) ;
#55604 = AXIS2_PLACEMENT_3D ( 'NONE', #79170, #97502, #47766 ) ;
#55605 = CARTESIAN_POINT ( 'NONE',  ( 11.44999999999991047, 12.50000000000000000, 6.213873640053558134 ) ) ;
#55606 = DIRECTION ( 'NONE',  ( 0.000000000000000000, 1.000000000000000000, 0.000000000000000000 ) ) ;
#55607 = CARTESIAN_POINT ( 'NONE',  ( -14.39999999999998614, 12.50000000000000000, -0.3464101615137760715 ) ) ;
#55608 = ORIENTED_EDGE ( 'NONE', *, *, #68372, .F. ) ;
#55609 = CARTESIAN_POINT ( 'NONE',  ( 7.499999999999961808, 2.500000000000000000, 4.330127018922196314 ) ) ;
#55610 = ADVANCED_FACE ( 'NONE', ( #79573 ), #78313, .T. ) ;
#55611 = ORIENTED_EDGE ( 'NONE', *, *, #10512, .T. ) ;
#55612 = EDGE_CURVE ( 'NONE', #27445, #17419, #115945, .T. ) ;
#55613 = ORIENTED_EDGE ( 'NONE', *, *, #26353, .T. ) ;
#55614 = EDGE_CURVE ( 'NONE', #97372, #101017, #65760, .T. ) ;
#55615 = CARTESIAN_POINT ( 'NONE',  ( 1.049999999999953637, 12.50000000000000000, -1.883746621131363597 ) ) ;
#55617 = ADVANCED_FACE ( 'NONE', ( #32907 ), #9330, .T. ) ;
#55616 = DIRECTION ( 'NONE',  ( 0.000000000000000000, 0.000000000000000000, -1.000000000000000000 ) ) ;
#55618 = CARTESIAN_POINT ( 'NONE',  ( -17.50000000000000000, 2.500000000000000000, 10.00000000000000178 ) ) ;
#55619 = CARTESIAN_POINT ( 'NONE',  ( 0.8499999999999536815, 2.500000000000000000, 6.595190528383296780 ) ) ;
#55620 = DIRECTION ( 'NONE',  ( 0.000000000000000000, 1.000000000000000000, 0.000000000000000000 ) ) ;
#55621 = DIRECTION ( 'NONE',  ( 0.000000000000000000, 0.000000000000000000, -1.000000000000000000 ) ) ;
#55622 = FACE_OUTER_BOUND ( 'NONE', #51984, .T. ) ;
#55623 = ORIENTED_EDGE ( 'NONE', *, *, #116344, .T. ) ;
#55624 = DIRECTION ( 'NONE',  ( 1.000000000000000000, 0.000000000000000000, 0.000000000000000000 ) ) ;
#55625 = AXIS2_PLACEMENT_3D ( 'NONE', #21442, #90162, #120931 ) ;
#55626 = EDGE_CURVE ( 'NONE', #32790, #36953, #74184, .T. ) ;
#55627 = CIRCLE ( 'NONE', #32671, 0.06509327318403743123 ) ;
#55628 = CIRCLE ( 'NONE', #3307, 0.06509327318403745899 ) ;
#55630 = ADVANCED_FACE ( 'NONE', ( #44007 ), #114029, .T. ) ;
#55629 = LINE ( 'NONE', #105376, #123025 ) ;
#55631 = ORIENTED_EDGE ( 'NONE', *, *, #50687, .F. ) ;
#55632 = ADVANCED_FACE ( 'NONE', ( #23713 ), #69986, .T. ) ;
#55633 = ORIENTED_EDGE ( 'NONE', *, *, #4470, .F. ) ;
#55634 = CIRCLE ( 'NONE', #76476, 0.06509327318403745899 ) ;
#55635 = ORIENTED_EDGE ( 'NONE', *, *, #7734, .T. ) ;
#55636 = ORIENTED_EDGE ( 'NONE', *, *, #41327, .F. ) ;
#55637 = CARTESIAN_POINT ( 'NONE',  ( -8.950000000000004619, 12.50000000000000000, 6.083687093685483660 ) ) ;
#55638 = DIRECTION ( 'NONE',  ( 0.000000000000000000, -0.000000000000000000, 1.000000000000000000 ) ) ;
#55639 = VECTOR ( 'NONE', #56782, 1000.000000000000000 ) ;
#55640 = CARTESIAN_POINT ( 'NONE',  ( 16.55874544816229488, 0.4845305829427787869, -6.091953208798931207 ) ) ;
#55641 = CARTESIAN_POINT ( 'NONE',  ( 10.44999999999991402, 12.50000000000000000, 6.430097255199259010 ) ) ;
#55643 = AXIS2_PLACEMENT_3D ( 'NONE', #128008, #50568, #106432 ) ;
#55642 = CIRCLE ( 'NONE', #93209, 0.06509327318403745899 ) ;
#55644 = DIRECTION ( 'NONE',  ( -0.000000000000000000, -1.000000000000000000, -0.000000000000000000 ) ) ;
#55645 = VERTEX_POINT ( 'NONE', #82642 ) ;
#55646 = DIRECTION ( 'NONE',  ( 0.000000000000000000, 1.000000000000000000, 0.000000000000000000 ) ) ;
#55647 = DIRECTION ( 'NONE',  ( 0.000000000000000000, 0.000000000000000000, 1.000000000000000000 ) ) ;
#55648 = DIRECTION ( 'NONE',  ( 0.000000000000000000, 1.000000000000000000, 0.000000000000000000 ) ) ;
#55649 = ORIENTED_EDGE ( 'NONE', *, *, #37721, .F. ) ;
#55650 = ORIENTED_EDGE ( 'NONE', *, *, #90793, .F. ) ;
#55651 = ORIENTED_EDGE ( 'NONE', *, *, #106428, .T. ) ;
#55652 = CARTESIAN_POINT ( 'NONE',  ( -11.24999999999996447, 12.50000000000000000, -2.099970236277060476 ) ) ;
#55653 = CARTESIAN_POINT ( 'NONE',  ( 0.5999999999999551248, 2.500000000000000000, -4.676537180435978769 ) ) ;
#55654 = CARTESIAN_POINT ( 'NONE',  ( 2.299999999999948752, 2.500000000000000000, 0.3464101615137735735 ) ) ;
#55655 = VERTEX_POINT ( 'NONE', #39668 ) ;
#55656 = DIRECTION ( 'NONE',  ( 0.000000000000000000, 0.000000000000000000, -1.000000000000000000 ) ) ;
#55657 = DIRECTION ( 'NONE',  ( 0.000000000000000000, 0.000000000000000000, 1.000000000000000000 ) ) ;
#55658 = DIRECTION ( 'NONE',  ( -0.000000000000000000, -1.000000000000000000, -0.000000000000000000 ) ) ;
#55659 = DIRECTION ( 'NONE',  ( 0.000000000000000000, 0.000000000000000000, 1.000000000000000000 ) ) ;
#55660 = CARTESIAN_POINT ( 'NONE',  ( 4.399999999999939071, 12.50000000000000000, 0.2813168883297362810 ) ) ;
#55661 = EDGE_CURVE ( 'NONE', #76546, #115931, #126416, .T. ) ;
#55662 = ORIENTED_EDGE ( 'NONE', *, *, #7245, .F. ) ;
#55663 = AXIS2_PLACEMENT_3D ( 'NONE', #95669, #105493, #93102 ) ;
#55664 = CARTESIAN_POINT ( 'NONE',  ( -2.900000000000030553, 12.50000000000000000, 5.022947341949748790 ) ) ;
#55665 = AXIS2_PLACEMENT_3D ( 'NONE', #110691, #111318, #51790 ) ;
#55666 = EDGE_CURVE ( 'NONE', #118209, #43898, #78403, .T. ) ;
#55667 = EDGE_LOOP ( 'NONE', ( #13169, #124339 ) ) ;
#55668 = ORIENTED_EDGE ( 'NONE', *, *, #15535, .F. ) ;
#55669 = VERTEX_POINT ( 'NONE', #13225 ) ;
#55670 = DIRECTION ( 'NONE',  ( 0.000000000000000000, -0.9999939076577903929, 0.003490651415223739937 ) ) ;
#55671 = FACE_BOUND ( 'NONE', #56012, .T. ) ;
#55672 = LINE ( 'NONE', #75309, #113947 ) ;
#55673 = FACE_OUTER_BOUND ( 'NONE', #105628, .T. ) ;
#55674 = ADVANCED_FACE ( 'NONE', ( #109679 ), #93062, .T. ) ;
#55675 = AXIS2_PLACEMENT_3D ( 'NONE', #79681, #20769, #91436 ) ;
#55676 = CARTESIAN_POINT ( 'NONE',  ( -0.4000000000000331624, 2.500000000000000000, -0.7928203230275518987 ) ) ;
#55677 = ORIENTED_EDGE ( 'NONE', *, *, #36007, .F. ) ;
#55678 = DIRECTION ( 'NONE',  ( 0.000000000000000000, 1.000000000000000000, 0.000000000000000000 ) ) ;
#55679 = CARTESIAN_POINT ( 'NONE',  ( 8.149999999999923972, 2.500000000000000000, -6.148780366869526226 ) ) ;
#55680 = DIRECTION ( 'NONE',  ( 0.000000000000000000, -0.9999939076577903929, 0.003490651415223739937 ) ) ;
#55681 = LINE ( 'NONE', #75962, #40620 ) ;
#55682 = ORIENTED_EDGE ( 'NONE', *, *, #74556, .T. ) ;
#55684 = CIRCLE ( 'NONE', #15961, 0.06509327318403745899 ) ;
#55683 = AXIS2_PLACEMENT_3D ( 'NONE', #8605, #45994, #127761 ) ;
#55685 = CARTESIAN_POINT ( 'NONE',  ( 6.449999999999931788, 12.50000000000000000, 6.083687093685482772 ) ) ;
#55686 = VECTOR ( 'NONE', #16924, 1000.000000000000000 ) ;
#55687 = CARTESIAN_POINT ( 'NONE',  ( -1.900000000000034994, 2.500000000000000000, -0.4464101615137783252 ) ) ;
#55688 = ORIENTED_EDGE ( 'NONE', *, *, #104684, .F. ) ;
#55689 = DIRECTION ( 'NONE',  ( 0.000000000000000000, 0.000000000000000000, 1.000000000000000000 ) ) ;
#55690 = FACE_BOUND ( 'NONE', #36114, .T. ) ;
#55691 = CARTESIAN_POINT ( 'NONE',  ( -11.64999999999999680, 2.500000000000000000, 2.065063509461097624 ) ) ;
#55692 = ORIENTED_EDGE ( 'NONE', *, *, #82729, .F. ) ;
#55693 = CARTESIAN_POINT ( 'NONE',  ( 3.149999999999946176, 2.500000000000000000, -1.818653347947325916 ) ) ;
#55694 = CARTESIAN_POINT ( 'NONE',  ( -1.900000000000034994, 2.500000000000000000, -0.3464101615137783474 ) ) ;
#55695 = ORIENTED_EDGE ( 'NONE', *, *, #68585, .F. ) ;
#55696 = VERTEX_POINT ( 'NONE', #64272 ) ;
#55697 = CARTESIAN_POINT ( 'NONE',  ( 184.9635416670080872, -4.367472073101519747, 7.564683531249999149 ) ) ;
#55698 = CIRCLE ( 'NONE', #66160, 0.06509327318403745899 ) ;
#55699 = ORIENTED_EDGE ( 'NONE', *, *, #52657, .F. ) ;
#55700 = CARTESIAN_POINT ( 'NONE',  ( 184.5885416670080872, -6.551208109652273848, -3.782341765625003571 ) ) ;
#55701 = CARTESIAN_POINT ( 'NONE',  ( 6.249999999999965361, 2.500000000000000000, 2.165063509461097713 ) ) ;
#55702 = AXIS2_PLACEMENT_3D ( 'NONE', #38302, #97211, #67749 ) ;
#55703 = EDGE_CURVE ( 'NONE', #54702, #54886, #11566, .T. ) ;
#55704 = CARTESIAN_POINT ( 'NONE',  ( 13.34999999999989662, 2.500000000000000000, -2.857883832488653741 ) ) ;
#55705 = DIRECTION ( 'NONE',  ( -0.000000000000000000, 1.000000000000000000, -0.000000000000000000 ) ) ;
#55706 = CIRCLE ( 'NONE', #55625, 0.06509327318403745899 ) ;
#55707 = DIRECTION ( 'NONE',  ( 0.000000000000000000, 1.000000000000000000, 0.000000000000000000 ) ) ;
#55708 = CIRCLE ( 'NONE', #122624, 0.06509327318403745899 ) ;
#55709 = CIRCLE ( 'NONE', #43136, 0.09999999999999982514 ) ;
#55710 = EDGE_LOOP ( 'NONE', ( #95562, #64800, #38367, #24512 ) ) ;
#55711 = CIRCLE ( 'NONE', #20222, 0.06509327318403741736 ) ;
#55712 = VERTEX_POINT ( 'NONE', #3421 ) ;
#55713 = DIRECTION ( 'NONE',  ( -0.000000000000000000, -1.000000000000000000, -0.000000000000000000 ) ) ;
#55714 = DIRECTION ( 'NONE',  ( -0.000000000000000000, 1.000000000000000000, -0.000000000000000000 ) ) ;
#55715 = PLANE ( 'NONE',  #120283 ) ;
#55716 = ADVANCED_FACE ( 'NONE', ( #123825 ), #42908, .T. ) ;
#55717 = CARTESIAN_POINT ( 'NONE',  ( 12.09999999999990195, 2.500000000000000000, 0.5928203230275495006 ) ) ;
#55719 = EDGE_LOOP ( 'NONE', ( #52756, #97601, #29994, #67356 ) ) ;
#55718 = ORIENTED_EDGE ( 'NONE', *, *, #51693, .F. ) ;
#55720 = DIRECTION ( 'NONE',  ( 0.000000000000000000, -1.000000000000000000, 0.000000000000000000 ) ) ;
#55721 = ORIENTED_EDGE ( 'NONE', *, *, #83190, .T. ) ;
#55722 = EDGE_CURVE ( 'NONE', #60318, #16136, #57554, .T. ) ;
#55723 = CARTESIAN_POINT ( 'NONE',  ( -6.900000000000015454, 2.500000000000000000, 3.983716857408420076 ) ) ;
#55724 = DIRECTION ( 'NONE',  ( 0.000000000000000000, 1.000000000000000000, 0.000000000000000000 ) ) ;
#55725 = AXIS2_PLACEMENT_3D ( 'NONE', #48614, #27657, #8025 ) ;
#55726 = EDGE_LOOP ( 'NONE', ( #129448, #72611, #102667, #25656 ) ) ;
#55727 = DIRECTION ( 'NONE',  ( -0.000000000000000000, -1.000000000000000000, -0.000000000000000000 ) ) ;
#55728 = DIRECTION ( 'NONE',  ( 0.000000000000000000, -0.000000000000000000, 1.000000000000000000 ) ) ;
#55729 = DIRECTION ( 'NONE',  ( 0.000000000000000000, 0.000000000000000000, 1.000000000000000000 ) ) ;
#55730 = AXIS2_PLACEMENT_3D ( 'NONE', #28858, #30154, #108694 ) ;
#55731 = CARTESIAN_POINT ( 'NONE',  ( -6.450000000000019718, 12.50000000000000000, -1.753560074763288679 ) ) ;
#55732 = CARTESIAN_POINT ( 'NONE',  ( 6.649999999999930189, 2.500000000000000000, 5.702370205355745014 ) ) ;
#55733 = LINE ( 'NONE', #85194, #89231 ) ;
#55734 = EDGE_CURVE ( 'NONE', #60113, #88053, #84732, .T. ) ;
#55735 = FACE_OUTER_BOUND ( 'NONE', #20182, .T. ) ;
#55736 = CARTESIAN_POINT ( 'NONE',  ( 13.09999999999989839, 2.500000000000000000, 0.3464101615137735735 ) ) ;
#55737 = DIRECTION ( 'NONE',  ( -0.000000000000000000, 1.000000000000000000, -0.000000000000000000 ) ) ;
#55738 = VERTEX_POINT ( 'NONE', #73439 ) ;
#55739 = VERTEX_POINT ( 'NONE', #24360 ) ;
#55740 = CARTESIAN_POINT ( 'NONE',  ( 5.599999999999933031, 2.500000000000000000, -0.2464101615137783419 ) ) ;
#55741 = ORIENTED_EDGE ( 'NONE', *, *, #123821, .F. ) ;
#55742 = DIRECTION ( 'NONE',  ( 0.000000000000000000, 0.000000000000000000, -1.000000000000000000 ) ) ;
#55744 = VERTEX_POINT ( 'NONE', #53185 ) ;
#55743 = VERTEX_POINT ( 'NONE', #23069 ) ;
#55745 = ORIENTED_EDGE ( 'NONE', *, *, #125123, .F. ) ;
#55746 = LINE ( 'NONE', #57022, #77152 ) ;
#55747 = FACE_OUTER_BOUND ( 'NONE', #115838, .T. ) ;
#55748 = ADVANCED_FACE ( 'NONE', ( #43370 ), #83286, .T. ) ;
#55749 =( NAMED_UNIT ( * ) PLANE_ANGLE_UNIT ( ) SI_UNIT ( $, .RADIAN. ) );
#55750 = CARTESIAN_POINT ( 'NONE',  ( 1.649999999999951505, 12.50000000000000000, -2.857883832488653741 ) ) ;
#55751 = CARTESIAN_POINT ( 'NONE',  ( -5.450000000000019718, 2.500000000000000000, 6.595190528383296780 ) ) ;
#55752 = DIRECTION ( 'NONE',  ( -4.274815082592931898E-19, -0.9999939076577903929, -0.003490651415223739937 ) ) ;
#55753 = ORIENTED_EDGE ( 'NONE', *, *, #64008, .T. ) ;
#55754 = DIRECTION ( 'NONE',  ( -0.000000000000000000, 1.000000000000000000, -0.000000000000000000 ) ) ;
#55755 = ORIENTED_EDGE ( 'NONE', *, *, #7632, .F. ) ;
#55756 = EDGE_CURVE ( 'NONE', #18162, #40987, #122315, .T. ) ;
#55758 = VERTEX_POINT ( 'NONE', #5980 ) ;
#55757 = AXIS2_PLACEMENT_3D ( 'NONE', #96944, #116581, #57684 ) ;
#55759 = ORIENTED_EDGE ( 'NONE', *, *, #7096, .F. ) ;
#55760 = EDGE_LOOP ( 'NONE', ( #79442, #60893 ) ) ;
#55761 = CARTESIAN_POINT ( 'NONE',  ( 3.749999999999942268, 12.50000000000000000, 1.407149913249508000 ) ) ;
#55762 = EDGE_CURVE ( 'NONE', #68655, #88216, #36640, .T. ) ;
#55763 = ORIENTED_EDGE ( 'NONE', *, *, #64490, .T. ) ;
#55764 = EDGE_CURVE ( 'NONE', #39804, #78396, #13620, .T. ) ;
#55765 = ORIENTED_EDGE ( 'NONE', *, *, #20363, .T. ) ;
#55766 = EDGE_CURVE ( 'NONE', #123894, #103956, #72129, .T. ) ;
#55767 = EDGE_CURVE ( 'NONE', #45538, #9181, #14512, .T. ) ;
#55768 = CARTESIAN_POINT ( 'NONE',  ( -3.750000000000025757, 2.500000000000000000, 1.472243186433545459 ) ) ;
#55770 = VECTOR ( 'NONE', #14774, 1000.000000000000000 ) ;
#55769 = CIRCLE ( 'NONE', #26524, 0.06509327318403745899 ) ;
#55771 = CARTESIAN_POINT ( 'NONE',  ( 10.44999999999991047, 2.500000000000000000, 2.065063509461097624 ) ) ;
#55772 = PLANE ( 'NONE',  #41704 ) ;
#55773 = CARTESIAN_POINT ( 'NONE',  ( 0.3999999999999563904, 2.500000000000000000, 3.737306695894644371 ) ) ;
#55774 = DIRECTION ( 'NONE',  ( 0.000000000000000000, 0.000000000000000000, -1.000000000000000000 ) ) ;
#55775 = EDGE_CURVE ( 'NONE', #5270, #1764, #21971, .T. ) ;
#55776 = DIRECTION ( 'NONE',  ( 0.000000000000000000, 0.000000000000000000, 1.000000000000000000 ) ) ;
#55777 = ORIENTED_EDGE ( 'NONE', *, *, #91982, .T. ) ;
#55778 = EDGE_CURVE ( 'NONE', #51310, #44668, #45044, .T. ) ;
#55779 = AXIS2_PLACEMENT_3D ( 'NONE', #55097, #125741, #14504 ) ;
#55780 = CARTESIAN_POINT ( 'NONE',  ( -4.150000000000027889, 12.50000000000000000, -7.188010851410854052 ) ) ;
#55782 = CIRCLE ( 'NONE', #82986, 0.06509327318403745899 ) ;
#55781 = VECTOR ( 'NONE', #119871, 1000.000000000000000 ) ;
#55783 = ADVANCED_FACE ( 'NONE', ( #36113 ), #15805, .T. ) ;
#55784 = EDGE_LOOP ( 'NONE', ( #110309, #52985 ) ) ;
#55785 = CARTESIAN_POINT ( 'NONE',  ( -12.09999999999999432, 12.50000000000000000, 4.957854068765711553 ) ) ;
#55786 = AXIS2_PLACEMENT_3D ( 'NONE', #104332, #76168, #13367 ) ;
#55787 = ADVANCED_FACE ( 'NONE', ( #114657 ), #25625, .T. ) ;
#55788 = VERTEX_POINT ( 'NONE', #115954 ) ;
#55789 = DIRECTION ( 'NONE',  ( 0.000000000000000000, 0.000000000000000000, -1.000000000000000000 ) ) ;
#55790 = ORIENTED_EDGE ( 'NONE', *, *, #67555, .T. ) ;
#55791 = EDGE_LOOP ( 'NONE', ( #61939, #116735 ) ) ;
#55792 = EDGE_CURVE ( 'NONE', #78283, #77627, #40851, .T. ) ;
#55793 = DIRECTION ( 'NONE',  ( 0.000000000000000000, 0.000000000000000000, -1.000000000000000000 ) ) ;
#55794 = DIRECTION ( 'NONE',  ( 0.000000000000000000, -0.000000000000000000, -1.000000000000000000 ) ) ;
#55795 = DIRECTION ( 'NONE',  ( 0.000000000000000000, 0.000000000000000000, -1.000000000000000000 ) ) ;
#55796 = PLANE ( 'NONE',  #82236 ) ;
#55797 = DIRECTION ( 'NONE',  ( 0.000000000000000000, -0.9999939076577903929, 0.003490651415223739937 ) ) ;
#55798 = ORIENTED_EDGE ( 'NONE', *, *, #127941, .T. ) ;
#55799 = DIRECTION ( 'NONE',  ( -0.000000000000000000, -1.000000000000000000, -0.000000000000000000 ) ) ;
#55800 = DIRECTION ( 'NONE',  ( 0.000000000000000000, 1.000000000000000000, 0.000000000000000000 ) ) ;
#55801 = DIRECTION ( 'NONE',  ( 0.000000000000000000, 0.000000000000000000, -1.000000000000000000 ) ) ;
#55802 = CONICAL_SURFACE ( 'NONE', #5598, 0.1000000000000000472, 0.003490658503988666988 ) ;
#55803 = CARTESIAN_POINT ( 'NONE',  ( 14.14999999999989200, 2.500000000000000000, -2.265063509461101798 ) ) ;
#55804 = VECTOR ( 'NONE', #119808, 1000.000000000000000 ) ;
#55805 = DIRECTION ( 'NONE',  ( -0.000000000000000000, 1.000000000000000000, -0.000000000000000000 ) ) ;
#55806 = ORIENTED_EDGE ( 'NONE', *, *, #101290, .F. ) ;
#55807 = CIRCLE ( 'NONE', #5606, 0.1000000000000000472 ) ;
#55808 = ORIENTED_EDGE ( 'NONE', *, *, #95416, .T. ) ;
#55809 = UNCERTAINTY_MEASURE_WITH_UNIT (LENGTH_MEASURE( 1.000000000000000082E-05 ), #54949, 'distance_accuracy_value', 'NONE');
#55810 = CIRCLE ( 'NONE', #66269, 0.09999999999999982514 ) ;
#55811 = ORIENTED_EDGE ( 'NONE', *, *, #70059, .T. ) ;
#55812 = AXIS2_PLACEMENT_3D ( 'NONE', #119618, #98682, #69223 ) ;
#55813 = CARTESIAN_POINT ( 'NONE',  ( 0.6499999999999543920, 2.500000000000000000, 6.841600689897072485 ) ) ;
#55814 = PLANE ( 'NONE',  #66869 ) ;
#55815 = CARTESIAN_POINT ( 'NONE',  ( 184.2916666666666572, 4.445597072760120838, -7.699999999999998401 ) ) ;
#55817 = CONICAL_SURFACE ( 'NONE', #85060, 0.1000000000000002554, 0.003490658503988666988 ) ;
#55816 = DIRECTION ( 'NONE',  ( 0.000000000000000000, 0.000000000000000000, -1.000000000000000000 ) ) ;
#55818 = DIRECTION ( 'NONE',  ( -0.000000000000000000, -1.000000000000000000, -0.000000000000000000 ) ) ;
#55819 = DIRECTION ( 'NONE',  ( 0.000000000000000000, 1.000000000000000000, 0.000000000000000000 ) ) ;
#55820 = DIRECTION ( 'NONE',  ( -0.000000000000000000, -1.000000000000000000, -0.000000000000000000 ) ) ;
#55821 = ORIENTED_EDGE ( 'NONE', *, *, #10270, .F. ) ;
#55822 = AXIS2_PLACEMENT_3D ( 'NONE', #92387, #43953, #2719 ) ;
#55823 = EDGE_CURVE ( 'NONE', #13248, #15249, #38706, .T. ) ;
#55824 = CARTESIAN_POINT ( 'NONE',  ( -12.04999999999999538, 2.500000000000000000, 2.165063509461097713 ) ) ;
#55825 = DIRECTION ( 'NONE',  ( 0.000000000000000000, 0.000000000000000000, 1.000000000000000000 ) ) ;
#55826 = EDGE_CURVE ( 'NONE', #53805, #122392, #87128, .T. ) ;
#55827 = ORIENTED_EDGE ( 'NONE', *, *, #104212, .T. ) ;
#55828 = CARTESIAN_POINT ( 'NONE',  ( 9.599999999999914380, 12.50000000000000000, 3.637306695894644726 ) ) ;
#55829 = DIRECTION ( 'NONE',  ( -0.000000000000000000, 1.000000000000000000, -0.000000000000000000 ) ) ;
#55830 = CARTESIAN_POINT ( 'NONE',  ( 8.149999999999923972, 2.500000000000000000, 2.511473670974873507 ) ) ;
#55831 = EDGE_LOOP ( 'NONE', ( #83075, #40668, #86925, #108827 ) ) ;
#55832 = FACE_OUTER_BOUND ( 'NONE', #23168, .T. ) ;
#55833 = ORIENTED_EDGE ( 'NONE', *, *, #111015, .T. ) ;
#55834 = DIRECTION ( 'NONE',  ( 0.000000000000000000, 0.000000000000000000, -1.000000000000000000 ) ) ;
#55835 = DIRECTION ( 'NONE',  ( 0.000000000000000000, 1.000000000000000000, 0.000000000000000000 ) ) ;
#55836 = CONICAL_SURFACE ( 'NONE', #78848, 0.1000000000000002554, 0.003490658503988666988 ) ;
#55837 = ORIENTED_EDGE ( 'NONE', *, *, #3778, .T. ) ;
#55838 = DIRECTION ( 'NONE',  ( 0.000000000000000000, 0.000000000000000000, 1.000000000000000000 ) ) ;
#55839 = CARTESIAN_POINT ( 'NONE',  ( -12.89999999999999147, 2.500000000000000000, 0.1000000000000018513 ) ) ;
#55840 = EDGE_LOOP ( 'NONE', ( #20624, #18264, #97441, #52771 ) ) ;
#55841 = VERTEX_POINT ( 'NONE', #4681 ) ;
#55842 = CARTESIAN_POINT ( 'NONE',  ( 9.149999999999916866, 2.500000000000000000, -1.372243186433550033 ) ) ;
#55843 = VECTOR ( 'NONE', #71198, 1000.000000000000000 ) ;
#55844 = AXIS2_PLACEMENT_3D ( 'NONE', #113776, #84303, #24747 ) ;
#55845 = VERTEX_POINT ( 'NONE', #117210 ) ;
#55846 = DIRECTION ( 'NONE',  ( 0.000000000000000000, 1.000000000000000000, 0.000000000000000000 ) ) ;
#55847 = DIRECTION ( 'NONE',  ( 0.000000000000000000, -0.9999939076577903929, 0.003490651415223739937 ) ) ;
#55848 = ORIENTED_EDGE ( 'NONE', *, *, #63688, .F. ) ;
#55849 = CARTESIAN_POINT ( 'NONE',  ( 4.149999999999939959, 12.50000000000000000, 2.857883832488649301 ) ) ;
#55850 = DIRECTION ( 'NONE',  ( 0.000000000000000000, 0.000000000000000000, -1.000000000000000000 ) ) ;
#55851 = ORIENTED_EDGE ( 'NONE', *, *, #62875, .F. ) ;
#55853 = AXIS2_PLACEMENT_3D ( 'NONE', #111388, #62322, #112705 ) ;
#55852 = AXIS2_PLACEMENT_3D ( 'NONE', #92872, #3830, #3203 ) ;
#55855 = EDGE_CURVE ( 'NONE', #64926, #114462, #64908, .T. ) ;
#55854 = FACE_OUTER_BOUND ( 'NONE', #17834, .T. ) ;
#55856 = CARTESIAN_POINT ( 'NONE',  ( 1.449999999999950440, 2.500000000000000000, 6.048780366869520364 ) ) ;
#55857 = PLANE ( 'NONE',  #120384 ) ;
#55858 = DIRECTION ( 'NONE',  ( 0.000000000000000000, 0.000000000000000000, 1.000000000000000000 ) ) ;
#55859 = DIRECTION ( 'NONE',  ( 0.000000000000000000, 0.000000000000000000, 1.000000000000000000 ) ) ;
#55860 = DIRECTION ( 'NONE',  ( 0.000000000000000000, 1.000000000000000000, 0.000000000000000000 ) ) ;
#55862 = AXIS2_PLACEMENT_3D ( 'NONE', #24792, #83079, #122994 ) ;
#55861 = CIRCLE ( 'NONE', #26536, 0.1000000000000000056 ) ;
#55863 = ORIENTED_EDGE ( 'NONE', *, *, #80122, .F. ) ;
#55864 = VERTEX_POINT ( 'NONE', #6601 ) ;
#55865 = VERTEX_POINT ( 'NONE', #94368 ) ;
#55866 = EDGE_LOOP ( 'NONE', ( #81923, #124082 ) ) ;
#55867 = CARTESIAN_POINT ( 'NONE',  ( -13.09999999999999076, 12.50000000000000000, 4.611443907251934426 ) ) ;
#55868 = CARTESIAN_POINT ( 'NONE',  ( -0.8500000000000386136, 2.500000000000000000, 7.088010851410848190 ) ) ;
#55869 = EDGE_CURVE ( 'NONE', #103647, #87563, #15665, .T. ) ;
#55870 = DIRECTION ( 'NONE',  ( 0.000000000000000000, 0.000000000000000000, -1.000000000000000000 ) ) ;
#55871 = VERTEX_POINT ( 'NONE', #15147 ) ;
#55872 = FACE_BOUND ( 'NONE', #13207, .T. ) ;
#55873 = EDGE_CURVE ( 'NONE', #92109, #93629, #126426, .T. ) ;
#55874 = PLANE ( 'NONE',  #106468 ) ;
#55875 = CARTESIAN_POINT ( 'NONE',  ( 7.899999999999924860, 2.500000000000000000, 4.922947341949748257 ) ) ;
#55876 = DIRECTION ( 'NONE',  ( 0.000000000000000000, 0.000000000000000000, -1.000000000000000000 ) ) ;
#55877 = VECTOR ( 'NONE', #104347, 1000.000000000000000 ) ;
#55878 = FACE_OUTER_BOUND ( 'NONE', #81677, .T. ) ;
#55879 = DIRECTION ( 'NONE',  ( 0.000000000000000000, -0.9999939076577903929, 0.003490651415223739937 ) ) ;
#55880 = CARTESIAN_POINT ( 'NONE',  ( -3.350000000000028955, 12.50000000000000000, -2.165063509461101710 ) ) ;
#55881 = CARTESIAN_POINT ( 'NONE',  ( -0.8500000000000382805, 2.500000000000000000, -5.902370205355750521 ) ) ;
#55882 = CARTESIAN_POINT ( 'NONE',  ( -11.84999999999999609, 12.50000000000000000, 6.148780366869520897 ) ) ;
#55883 = EDGE_CURVE ( 'NONE', #43992, #28400, #126507, .T. ) ;
#55884 = DIRECTION ( 'NONE',  ( -0.000000000000000000, 1.000000000000000000, -0.000000000000000000 ) ) ;
#55885 = CIRCLE ( 'NONE', #1592, 0.06509327318403745899 ) ;
#55886 = DIRECTION ( 'NONE',  ( -0.000000000000000000, -1.000000000000000000, -0.000000000000000000 ) ) ;
#55887 = ORIENTED_EDGE ( 'NONE', *, *, #77573, .T. ) ;
#55889 = VERTEX_POINT ( 'NONE', #65559 ) ;
#55888 = AXIS2_PLACEMENT_3D ( 'NONE', #119395, #118764, #107665 ) ;
#55890 = ORIENTED_EDGE ( 'NONE', *, *, #74565, .T. ) ;
#55891 = ORIENTED_EDGE ( 'NONE', *, *, #57838, .F. ) ;
#55892 = CARTESIAN_POINT ( 'NONE',  ( -11.44999999999999929, 12.50000000000000000, -6.148780366869522673 ) ) ;
#55893 = ORIENTED_EDGE ( 'NONE', *, *, #78944, .T. ) ;
#55894 = CARTESIAN_POINT ( 'NONE',  ( -5.450000000000019718, 2.500000000000000000, 6.595190528383296780 ) ) ;
#55895 = EDGE_LOOP ( 'NONE', ( #72516, #26091, #99105, #22381 ) ) ;
#55897 = EDGE_LOOP ( 'NONE', ( #23831, #1221 ) ) ;
#55896 = AXIS2_PLACEMENT_3D ( 'NONE', #10775, #98520, #8854 ) ;
#55899 = CONICAL_SURFACE ( 'NONE', #122803, 0.1000000000000000472, 0.003490658503988666988 ) ;
#55898 = CARTESIAN_POINT ( 'NONE',  ( 12.29999999999990123, 12.50000000000000000, 0.3464101615137735735 ) ) ;
#55900 = CONICAL_SURFACE ( 'NONE', #112344, 0.1000000000000002554, 0.003490658503988666988 ) ;
#55902 = DIRECTION ( 'NONE',  ( 0.000000000000000000, 0.000000000000000000, 1.000000000000000000 ) ) ;
#55901 = PRODUCT_DEFINITION_CONTEXT ( 'detailed design', #83124, 'design' ) ;
#55903 = FACE_OUTER_BOUND ( 'NONE', #61533, .T. ) ;
#55904 = CARTESIAN_POINT ( 'NONE',  ( -1.450000000000035927, 12.50000000000000000, -6.213873640053564351 ) ) ;
#55905 = CARTESIAN_POINT ( 'NONE',  ( -14.14999999999998614, 12.50000000000000000, -2.230156782645137170 ) ) ;
#55906 = AXIS2_PLACEMENT_3D ( 'NONE', #77789, #18877, #129519 ) ;
#55907 = VERTEX_POINT ( 'NONE', #95675 ) ;
#55908 = EDGE_LOOP ( 'NONE', ( #70529, #82026, #24129, #125265 ) ) ;
#55909 = EDGE_CURVE ( 'NONE', #113368, #104854, #82597, .T. ) ;
#55910 = AXIS2_PLACEMENT_3D ( 'NONE', #116128, #114831, #16625 ) ;
#55911 = EDGE_LOOP ( 'NONE', ( #104851, #979, #39321, #7611 ) ) ;
#55912 = EDGE_LOOP ( 'NONE', ( #8760, #77299 ) ) ;
#55913 = DIRECTION ( 'NONE',  ( 0.9974916312695811804, -0.05217691604167150332, -0.04783319955355572195 ) ) ;
#55914 =( BOUNDED_SURFACE ( )  B_SPLINE_SURFACE ( 3, 2, ( 
 ( #49250, #9951, #100268 ),
 ( #51180, #79975, #108781 ),
 ( #121187, #128458, #20419 ),
 ( #89152, #49893, #60976 ),
 ( #31526, #98314, #38798 ),
 ( #60363, #119903, #89795 ),
 ( #10572, #88498, #39442 ),
 ( #110084, #119250, #50508 ),
 ( #90419, #91086, #80636 ),
 ( #110715, #70799, #120548 ),
 ( #9211, #108700, #28867 ),
 ( #98231, #70071, #88397 ) ),
 .UNSPECIFIED., .F., .F., .F. ) 
 B_SPLINE_SURFACE_WITH_KNOTS ( ( 4, 2, 2, 2, 2, 4 ),
 ( 3, 3 ),
 ( 0.02236387153718017232, 0.03065407938765537382, 0.03894428723813057880, 0.05552470293908098875, 0.07210511864003139870, 0.08868553434098180865 ),
 ( 0.000000000000000000, 1.000000000000000000 ),
 .UNSPECIFIED. ) 
 GEOMETRIC_REPRESENTATION_ITEM ( )  RATIONAL_B_SPLINE_SURFACE ( (
 ( 1.000000000000000000, 0.7318752858502177716, 1.000000000000000000),
 ( 1.000000000000000000, 0.7503381610177722871, 1.000000000000000000),
 ( 1.000000000000000000, 0.7702514485279070566, 1.000000000000000000),
 ( 1.000000000000000000, 0.8097395513079956864, 1.000000000000000000),
 ( 1.000000000000000000, 0.8293075644331776575, 1.000000000000000000),
 ( 1.000000000000000000, 0.8842435496613439971, 1.000000000000000000),
 ( 1.000000000000000000, 0.9156028214505685936, 1.000000000000000000),
 ( 1.000000000000000000, 0.9624374057520458381, 1.000000000000000000),
 ( 1.000000000000000000, 0.9780629942474001748, 1.000000000000000000),
 ( 1.000000000000000000, 0.9967432622277094811, 1.000000000000000000),
 ( 1.000000000000000000, 0.9999962847131013133, 1.000000000000000000),
 ( 1.000000000000000000, 1.000000000000000000, 1.000000000000000000) ) ) 
 REPRESENTATION_ITEM ( '' )  SURFACE ( )  );
#55915 = ORIENTED_EDGE ( 'NONE', *, *, #23802, .F. ) ;
#55916 = EDGE_CURVE ( 'NONE', #3681, #6598, #86779, .T. ) ;
#55917 = ORIENTED_EDGE ( 'NONE', *, *, #60903, .F. ) ;
#55918 = EDGE_CURVE ( 'NONE', #103499, #23121, #88846, .T. ) ;
#55919 = DIRECTION ( 'NONE',  ( 0.000000000000000000, -0.000000000000000000, 1.000000000000000000 ) ) ;
#55920 = DIRECTION ( 'NONE',  ( 0.000000000000000000, 0.000000000000000000, 1.000000000000000000 ) ) ;
#55921 = FACE_OUTER_BOUND ( 'NONE', #92686, .T. ) ;
#55922 = DIRECTION ( 'NONE',  ( 0.000000000000000000, 0.000000000000000000, 1.000000000000000000 ) ) ;
#55923 = ADVANCED_FACE ( 'NONE', ( #59644 ), #7921, .T. ) ;
#55924 = EDGE_CURVE ( 'NONE', #6869, #88265, #65853, .T. ) ;
#55925 = CARTESIAN_POINT ( 'NONE',  ( 12.94999999999990337, 12.50000000000000000, 2.099970236277060032 ) ) ;
#55926 = DIRECTION ( 'NONE',  ( 0.000000000000000000, 0.000000000000000000, 1.000000000000000000 ) ) ;
#55927 = EDGE_CURVE ( 'NONE', #26594, #123378, #80544, .T. ) ;
#55928 = VERTEX_POINT ( 'NONE', #49811 ) ;
#55929 = DIRECTION ( 'NONE',  ( 0.000000000000000000, 0.000000000000000000, 1.000000000000000000 ) ) ;
#55930 = ORIENTED_EDGE ( 'NONE', *, *, #35679, .F. ) ;
#55931 = DIRECTION ( 'NONE',  ( 0.000000000000000000, 1.000000000000000000, 0.000000000000000000 ) ) ;
#55932 = EDGE_CURVE ( 'NONE', #101170, #8727, #48501, .T. ) ;
#55933 = ORIENTED_EDGE ( 'NONE', *, *, #90615, .F. ) ;
#55934 = LINE ( 'NONE', #127271, #126728 ) ;
#55935 = PLANE ( 'NONE',  #15580 ) ;
#55936 = VERTEX_POINT ( 'NONE', #89713 ) ;
#55937 = CARTESIAN_POINT ( 'NONE',  ( 10.59999999999990905, 2.500000000000000000, 4.676537180435972552 ) ) ;
#55938 = DIRECTION ( 'NONE',  ( -0.000000000000000000, -1.000000000000000000, -0.000000000000000000 ) ) ;
#55939 = VERTEX_POINT ( 'NONE', #69416 ) ;
#55940 = EDGE_CURVE ( 'NONE', #34057, #73263, #24101, .T. ) ;
#55941 = DIRECTION ( 'NONE',  ( -0.000000000000000000, 1.000000000000000000, -0.000000000000000000 ) ) ;
#55942 = AXIS2_PLACEMENT_3D ( 'NONE', #19189, #99072, #29681 ) ;
#55943 = DIRECTION ( 'NONE',  ( -0.000000000000000000, 1.000000000000000000, -0.000000000000000000 ) ) ;
#55944 = EDGE_LOOP ( 'NONE', ( #73735, #57890, #66484, #19142 ) ) ;
#55945 = ORIENTED_EDGE ( 'NONE', *, *, #49431, .T. ) ;
#55946 = CARTESIAN_POINT ( 'NONE',  ( 9.149999999999915090, 2.500000000000000000, -2.165063509461101710 ) ) ;
#55947 = LINE ( 'NONE', #118089, #97357 ) ;
#55948 = CARTESIAN_POINT ( 'NONE',  ( 186.9635416670080303, -4.367472073101519747, 7.564683531249999149 ) ) ;
#55949 = DIRECTION ( 'NONE',  ( 0.000000000000000000, 0.000000000000000000, 1.000000000000000000 ) ) ;
#55950 = AXIS2_PLACEMENT_3D ( 'NONE', #107611, #125946, #56559 ) ;
#55951 = AXIS2_PLACEMENT_3D ( 'NONE', #45951, #95049, #13887 ) ;
#55952 = DIRECTION ( 'NONE',  ( 0.000000000000000000, 1.000000000000000000, 0.000000000000000000 ) ) ;
#55953 = CIRCLE ( 'NONE', #32990, 0.1000000000000002554 ) ;
#55954 = DIRECTION ( 'NONE',  ( 0.000000000000000000, 0.000000000000000000, 1.000000000000000000 ) ) ;
#55955 = ORIENTED_EDGE ( 'NONE', *, *, #46130, .T. ) ;
#55956 = CARTESIAN_POINT ( 'NONE',  ( 4.149999999999941735, 2.500000000000000000, -7.288010851410854585 ) ) ;
#55957 = ORIENTED_EDGE ( 'NONE', *, *, #6933, .F. ) ;
#55958 = AXIS2_PLACEMENT_3D ( 'NONE', #74313, #84114, #124044 ) ;
#55959 = DIRECTION ( 'NONE',  ( 0.000000000000000000, 0.000000000000000000, 1.000000000000000000 ) ) ;
#55960 = CARTESIAN_POINT ( 'NONE',  ( 4.599999999999935696, 2.500000000000000000, 5.122947341949749323 ) ) ;
#55961 = DIRECTION ( 'NONE',  ( 0.000000000000000000, 1.000000000000000000, 0.000000000000000000 ) ) ;
#55962 = ORIENTED_EDGE ( 'NONE', *, *, #44811, .F. ) ;
#55963 = AXIS2_PLACEMENT_3D ( 'NONE', #86255, #113313, #62925 ) ;
#55964 = EDGE_CURVE ( 'NONE', #17990, #126026, #113980, .T. ) ;
#55965 = DIRECTION ( 'NONE',  ( -4.274815082592931898E-19, -0.9999939076577903929, -0.003490651415223739937 ) ) ;
#55966 = DIRECTION ( 'NONE',  ( -0.000000000000000000, 1.000000000000000000, -0.000000000000000000 ) ) ;
#55967 = CONICAL_SURFACE ( 'NONE', #64292, 0.1000000000000002554, 0.003490658503988666988 ) ;
#55968 = VERTEX_POINT ( 'NONE', #50431 ) ;
#55969 = CONICAL_SURFACE ( 'NONE', #74862, 0.1000000000000002554, 0.003490658503988666988 ) ;
#55970 = LINE ( 'NONE', #77543, #84423 ) ;
#55971 = EDGE_CURVE ( 'NONE', #84309, #19348, #74280, .T. ) ;
#55972 = VECTOR ( 'NONE', #76113, 1000.000000000000000 ) ;
#55973 = VERTEX_POINT ( 'NONE', #118521 ) ;
#55974 = ORIENTED_EDGE ( 'NONE', *, *, #104545, .T. ) ;
#55975 = FACE_OUTER_BOUND ( 'NONE', #106140, .T. ) ;
#55976 = CONICAL_SURFACE ( 'NONE', #76919, 0.1000000000000002554, 0.003490658503988666988 ) ;
#55977 = ORIENTED_EDGE ( 'NONE', *, *, #22308, .F. ) ;
#55978 = CARTESIAN_POINT ( 'NONE',  ( 11.69999999999990870, 2.500000000000000000, -4.330127018922201643 ) ) ;
#55979 = CARTESIAN_POINT ( 'NONE',  ( -14.79999999999998472, 2.500000000000000000, 0.2464101615137758439 ) ) ;
#55980 = CIRCLE ( 'NONE', #10033, 0.1000000000000002554 ) ;
#55981 = DIRECTION ( 'NONE',  ( 0.000000000000000000, 1.000000000000000000, 0.000000000000000000 ) ) ;
#55982 = ORIENTED_EDGE ( 'NONE', *, *, #77544, .F. ) ;
#55983 = CIRCLE ( 'NONE', #66452, 0.06509327318403745899 ) ;
#55984 = FACE_BOUND ( 'NONE', #96430, .T. ) ;
#55986 = ORIENTED_EDGE ( 'NONE', *, *, #34968, .T. ) ;
#55985 = DIRECTION ( 'NONE',  ( -4.274815082592931898E-19, -0.9999939076577903929, -0.003490651415223739937 ) ) ;
#55987 = FACE_OUTER_BOUND ( 'NONE', #21788, .T. ) ;
#55988 = VECTOR ( 'NONE', #10812, 1000.000000000000000 ) ;
#55989 = DIRECTION ( 'NONE',  ( -4.274815082592931898E-19, -0.9999939076577903929, -0.003490651415223739937 ) ) ;
#55990 = ORIENTED_EDGE ( 'NONE', *, *, #102356, .T. ) ;
#55992 = CIRCLE ( 'NONE', #1619, 0.5000000000000000000 ) ;
#55991 = CIRCLE ( 'NONE', #72736, 0.06509327318403745899 ) ;
#55993 = VERTEX_POINT ( 'NONE', #38036 ) ;
#55994 = ORIENTED_EDGE ( 'NONE', *, *, #84735, .T. ) ;
#55995 = CARTESIAN_POINT ( 'NONE',  ( -3.750000000000027534, 2.500000000000000000, -1.372243186433550033 ) ) ;
#55996 = CARTESIAN_POINT ( 'NONE',  ( -8.550000000000011369, 2.500000000000000000, 1.818653347947321475 ) ) ;
#55997 = CARTESIAN_POINT ( 'NONE',  ( 3.099999999999945022, 2.500000000000000000, -4.576537180435978236 ) ) ;
#55998 = FACE_BOUND ( 'NONE', #44188, .T. ) ;
#55999 = ORIENTED_EDGE ( 'NONE', *, *, #84164, .F. ) ;
#56000 = CARTESIAN_POINT ( 'NONE',  ( 185.6510416670080303, 4.367472073101518859, -7.564683531249999149 ) ) ;
#56001 = LINE ( 'NONE', #105100, #44925 ) ;
#56002 = DIRECTION ( 'NONE',  ( -0.000000000000000000, -1.000000000000000000, -0.000000000000000000 ) ) ;
#56003 = ADVANCED_FACE ( 'NONE', ( #110007 ), #57892, .T. ) ;
#56004 = CARTESIAN_POINT ( 'NONE',  ( -2.000000000000000000, 2.449293598294706414E-16, -5.000000000000004441 ) ) ;
#56005 = CARTESIAN_POINT ( 'NONE',  ( -6.250000000000019540, 2.500000000000000000, -7.188010851410854052 ) ) ;
#56006 = DIRECTION ( 'NONE',  ( 0.000000000000000000, 1.000000000000000000, 0.000000000000000000 ) ) ;
#56007 = DIRECTION ( 'NONE',  ( 0.000000000000000000, 0.000000000000000000, 1.000000000000000000 ) ) ;
#56008 = LINE ( 'NONE', #116861, #50267 ) ;
#56009 = EDGE_CURVE ( 'NONE', #104853, #41663, #51311, .T. ) ;
#56010 = CARTESIAN_POINT ( 'NONE',  ( -7.900000000000014566, 2.500000000000000000, -5.022947341949754119 ) ) ;
#56011 = ORIENTED_EDGE ( 'NONE', *, *, #78930, .F. ) ;
#56012 = EDGE_LOOP ( 'NONE', ( #78378, #49325 ) ) ;
#56013 = ORIENTED_EDGE ( 'NONE', *, *, #50466, .T. ) ;
#56014 = VERTEX_POINT ( 'NONE', #58971 ) ;
#56015 = ORIENTED_EDGE ( 'NONE', *, *, #34862, .F. ) ;
#56016 = DIRECTION ( 'NONE',  ( -1.000000000000000000, 0.000000000000000000, 0.000000000000000000 ) ) ;
#56018 = ADVANCED_FACE ( 'NONE', ( #681 ), #68128, .T. ) ;
#56017 = AXIS2_PLACEMENT_3D ( 'NONE', #50262, #129489, #118991 ) ;
#56019 = CARTESIAN_POINT ( 'NONE',  ( -15.39999999999998082, 2.500000000000000000, 0.7928203230275517877 ) ) ;
#56020 = ORIENTED_EDGE ( 'NONE', *, *, #81163, .T. ) ;
#56021 = FACE_BOUND ( 'NONE', #53370, .T. ) ;
#56022 = EDGE_CURVE ( 'NONE', #118638, #26544, #30710, .T. ) ;
#56023 = LINE ( 'NONE', #126056, #83486 ) ;
#56024 = CONICAL_SURFACE ( 'NONE', #45583, 0.09999999999999999167, 0.003490658503988666988 ) ;
#56025 = VECTOR ( 'NONE', #70161, 1000.000000000000000 ) ;
#56026 = EDGE_CURVE ( 'NONE', #94402, #96192, #9846, .T. ) ;
#56027 = LINE ( 'NONE', #54733, #5092 ) ;
#56028 = DIRECTION ( 'NONE',  ( 0.000000000000000000, 0.000000000000000000, 1.000000000000000000 ) ) ;
#56029 = CARTESIAN_POINT ( 'NONE',  ( 185.5000000000000000, 0.000000000000000000, 7.700000000000000178 ) ) ;
#56030 = ADVANCED_FACE ( 'NONE', ( #88408 ), #49574, .T. ) ;
#56031 = DIRECTION ( 'NONE',  ( 0.000000000000000000, 1.000000000000000000, 0.000000000000000000 ) ) ;
#56032 = EDGE_LOOP ( 'NONE', ( #96080, #128165, #106419, #4989 ) ) ;
#56033 = CONICAL_SURFACE ( 'NONE', #70714, 0.1000000000000002554, 0.003490658503988666988 ) ;
#56034 = ORIENTED_EDGE ( 'NONE', *, *, #125476, .T. ) ;
#56035 = CIRCLE ( 'NONE', #102025, 0.06509327318403745899 ) ;
#56036 = EDGE_LOOP ( 'NONE', ( #121779, #14802 ) ) ;
#56037 = EDGE_LOOP ( 'NONE', ( #9512, #81616 ) ) ;
#56038 = CARTESIAN_POINT ( 'NONE',  ( -9.800000000000006040, 12.50000000000000000, -4.676537180435974328 ) ) ;
#56039 = DIRECTION ( 'NONE',  ( 1.000000000000000000, 0.000000000000000000, 0.000000000000000000 ) ) ;
#56040 = DIRECTION ( 'NONE',  ( 0.000000000000000000, 0.000000000000000000, 1.000000000000000000 ) ) ;
#56041 = ORIENTED_EDGE ( 'NONE', *, *, #16988, .T. ) ;
#56042 = DIRECTION ( 'NONE',  ( -0.000000000000000000, 1.000000000000000000, -0.000000000000000000 ) ) ;
#56043 = CONICAL_SURFACE ( 'NONE', #129251, 0.1000000000000002554, 0.003490658503988666988 ) ;
#56044 = DIRECTION ( 'NONE',  ( 0.000000000000000000, 1.000000000000000000, 0.000000000000000000 ) ) ;
#56045 = LINE ( 'NONE', #124807, #30690 ) ;
#56046 = CARTESIAN_POINT ( 'NONE',  ( 184.1145833340161175, 6.668395609140177704, -3.849999999999998312 ) ) ;
#56047 = FACE_OUTER_BOUND ( 'NONE', #84836, .T. ) ;
#56048 = AXIS2_PLACEMENT_3D ( 'NONE', #58395, #47280, #47926 ) ;
#56049 = CARTESIAN_POINT ( 'NONE',  ( -11.05000000000000071, 12.50000000000000000, 6.906693963081109722 ) ) ;
#56050 = ORIENTED_EDGE ( 'NONE', *, *, #99140, .T. ) ;
#56051 = FACE_OUTER_BOUND ( 'NONE', #38295, .T. ) ;
#56052 = CIRCLE ( 'NONE', #60302, 0.06509327318403745899 ) ;
#56053 = EDGE_LOOP ( 'NONE', ( #110746, #67034 ) ) ;
#56054 = EDGE_LOOP ( 'NONE', ( #4205, #31380 ) ) ;
#56055 = AXIS2_PLACEMENT_3D ( 'NONE', #10036, #29044, #37571 ) ;
#56056 = CARTESIAN_POINT ( 'NONE',  ( -11.44999999999999929, 12.50000000000000000, -1.818653347947322141 ) ) ;
#56057 = DIRECTION ( 'NONE',  ( 0.000000000000000000, 1.000000000000000000, 0.000000000000000000 ) ) ;
#56058 = CARTESIAN_POINT ( 'NONE',  ( 2.899999999999946620, 2.500000000000000000, -0.6928203230275542523 ) ) ;
#56059 = CIRCLE ( 'NONE', #64383, 0.06509327318403741736 ) ;
#56060 = ORIENTED_EDGE ( 'NONE', *, *, #45605, .F. ) ;
#56061 = CIRCLE ( 'NONE', #62444, 0.06509327318403745899 ) ;
#56063 = ADVANCED_FACE ( 'NONE', ( #79267 ), #28876, .T. ) ;
#56062 = EDGE_LOOP ( 'NONE', ( #67850, #53791 ) ) ;
#56064 = CARTESIAN_POINT ( 'NONE',  ( 3.149999999999946176, 2.500000000000000000, -1.718653347947325827 ) ) ;
#56065 = AXIS2_PLACEMENT_3D ( 'NONE', #117954, #126504, #37492 ) ;
#56066 = DIRECTION ( 'NONE',  ( 0.000000000000000000, -0.9999939076577903929, 0.003490651415223739937 ) ) ;
#56068 = EDGE_CURVE ( 'NONE', #125967, #72978, #101800, .T. ) ;
#56067 = DIRECTION ( 'NONE',  ( -4.274815082592931898E-19, -0.9999939076577903929, -0.003490651415223739937 ) ) ;
#56069 = EDGE_LOOP ( 'NONE', ( #15416, #19382, #16716, #68072 ) ) ;
#56070 = VERTEX_POINT ( 'NONE', #113207 ) ;
#56071 = EDGE_CURVE ( 'NONE', #92620, #66161, #72559, .T. ) ;
#56072 = DIRECTION ( 'NONE',  ( 0.000000000000000000, -0.9999939076577903929, 0.003490651415223739937 ) ) ;
#56073 = CIRCLE ( 'NONE', #68596, 0.1000000000000002554 ) ;
#56074 = EDGE_CURVE ( 'NONE', #58451, #73869, #70399, .T. ) ;
#56075 = EDGE_CURVE ( 'NONE', #27855, #64286, #99749, .T. ) ;
#56076 = VERTEX_POINT ( 'NONE', #31450 ) ;
#56077 = DIRECTION ( 'NONE',  ( -0.000000000000000000, 1.000000000000000000, -0.000000000000000000 ) ) ;
#56078 = CARTESIAN_POINT ( 'NONE',  ( -8.950000000000011724, 2.500000000000000000, -6.148780366869520897 ) ) ;
#56079 = EDGE_LOOP ( 'NONE', ( #27913, #87203, #121550, #119355 ) ) ;
#56080 = DIRECTION ( 'NONE',  ( 0.000000000000000000, 1.000000000000000000, 0.000000000000000000 ) ) ;
#56081 = EDGE_CURVE ( 'NONE', #128794, #105778, #97576, .T. ) ;
#56082 = DIRECTION ( 'NONE',  ( 0.000000000000000000, -0.9999939076577903929, 0.003490651415223739937 ) ) ;
#56083 = DIRECTION ( 'NONE',  ( 0.000000000000000000, 0.000000000000000000, 1.000000000000000000 ) ) ;
#56084 = AXIS2_PLACEMENT_3D ( 'NONE', #26732, #106570, #117657 ) ;
#56085 = CARTESIAN_POINT ( 'NONE',  ( 10.64999999999990976, 12.50000000000000000, 1.883746621131358934 ) ) ;
#56086 = ORIENTED_EDGE ( 'NONE', *, *, #67123, .T. ) ;
#56087 = EDGE_CURVE ( 'NONE', #111256, #19044, #11895, .T. ) ;
#56088 = CARTESIAN_POINT ( 'NONE',  ( -0.8500000000000390576, 2.500000000000000000, -6.495190528383302464 ) ) ;
#56090 = EDGE_CURVE ( 'NONE', #59007, #16781, #123048, .T. ) ;
#56089 = CIRCLE ( 'NONE', #53957, 0.06509327318403745899 ) ;
#56091 = LINE ( 'NONE', #32405, #45736 ) ;
#56092 = EDGE_LOOP ( 'NONE', ( #128608, #31077, #108898, #114075 ) ) ;
#56093 = VERTEX_POINT ( 'NONE', #110639 ) ;
#56094 = CARTESIAN_POINT ( 'NONE',  ( 184.2135416670080588, 4.367472073101518859, -7.564683531249999149 ) ) ;
#56095 = DIRECTION ( 'NONE',  ( -0.000000000000000000, -1.000000000000000000, -0.000000000000000000 ) ) ;
#56096 = PLANE ( 'NONE',  #84497 ) ;
#56097 = FACE_OUTER_BOUND ( 'NONE', #115776, .T. ) ;
#56098 = CARTESIAN_POINT ( 'NONE',  ( -12.49999999999999467, 2.500000000000000000, -3.537306695894647302 ) ) ;
#56099 = CARTESIAN_POINT ( 'NONE',  ( 8.549999999999918998, 12.50000000000000000, -1.818653347947326138 ) ) ;
#56100 = CARTESIAN_POINT ( 'NONE',  ( 5.449999999999937117, 12.50000000000000000, -6.430097255199264339 ) ) ;
#56101 = CARTESIAN_POINT ( 'NONE',  ( -6.050000000000022027, 2.500000000000000000, -6.248780366869526759 ) ) ;
#56102 = CARTESIAN_POINT ( 'NONE',  ( -3.350000000000028955, 12.50000000000000000, 7.188010851410848723 ) ) ;
#56103 = AXIS2_PLACEMENT_3D ( 'NONE', #121705, #71313, #71983 ) ;
#56104 = CARTESIAN_POINT ( 'NONE',  ( 10.64999999999991331, 2.500000000000000000, -2.511473670974877948 ) ) ;
#56105 = VERTEX_POINT ( 'NONE', #111257 ) ;
#56106 = CIRCLE ( 'NONE', #119100, 7.500000000000000000 ) ;
#56107 = CONICAL_SURFACE ( 'NONE', #72852, 0.1000000000000002554, 0.003490658503988666988 ) ;
#56108 = ORIENTED_EDGE ( 'NONE', *, *, #127435, .T. ) ;
#56109 = AXIS2_PLACEMENT_3D ( 'NONE', #4376, #44990, #66539 ) ;
#56110 = DIRECTION ( 'NONE',  ( 0.000000000000000000, 1.000000000000000000, 0.000000000000000000 ) ) ;
#56111 = VERTEX_POINT ( 'NONE', #102117 ) ;
#56112 = DIRECTION ( 'NONE',  ( 0.000000000000000000, -0.000000000000000000, 1.000000000000000000 ) ) ;
#56113 = DIRECTION ( 'NONE',  ( -0.000000000000000000, -1.000000000000000000, -0.000000000000000000 ) ) ;
#56114 = CARTESIAN_POINT ( 'NONE',  ( 11.24999999999991118, 2.500000000000000000, 5.802370205355744659 ) ) ;
#56115 = AXIS2_PLACEMENT_3D ( 'NONE', #22605, #90673, #111606 ) ;
#56116 = EDGE_LOOP ( 'NONE', ( #53926, #51583 ) ) ;
#56117 = AXIS2_PLACEMENT_3D ( 'NONE', #53675, #15006, #43875 ) ;
#56118 = CARTESIAN_POINT ( 'NONE',  ( -14.14999999999998614, 12.50000000000000000, -2.165063509461099489 ) ) ;
#56119 = VECTOR ( 'NONE', #82989, 1000.000000000000000 ) ;
#56120 = CARTESIAN_POINT ( 'NONE',  ( 7.499999999999960032, 2.500000000000000000, 0.09999999999999772959 ) ) ;
#56122 = ORIENTED_EDGE ( 'NONE', *, *, #8470, .F. ) ;
#56121 = CARTESIAN_POINT ( 'NONE',  ( 13.29999999999990301, 12.50000000000000000, 4.330127018922196314 ) ) ;
#56123 = AXIS2_PLACEMENT_3D ( 'NONE', #87547, #38484, #109780 ) ;
#56124 = CARTESIAN_POINT ( 'NONE',  ( 4.799999999999937650, 2.500000000000000000, -4.083716857408426826 ) ) ;
#56125 = ORIENTED_EDGE ( 'NONE', *, *, #23212, .F. ) ;
#56126 = EDGE_CURVE ( 'NONE', #120581, #63587, #47424, .T. ) ;
#56127 = AXIS2_PLACEMENT_3D ( 'NONE', #100854, #11188, #71391 ) ;
#56128 = VERTEX_POINT ( 'NONE', #12429 ) ;
#56129 = EDGE_LOOP ( 'NONE', ( #51192, #119662 ) ) ;
#56130 = VERTEX_POINT ( 'NONE', #33392 ) ;
#56131 = LINE ( 'NONE', #113785, #119988 ) ;
#56132 = DIRECTION ( 'NONE',  ( 0.000000000000000000, 0.000000000000000000, 1.000000000000000000 ) ) ;
#56133 = CARTESIAN_POINT ( 'NONE',  ( 3.299999999999942979, 12.50000000000000000, 4.330127018922196314 ) ) ;
#56134 = CARTESIAN_POINT ( 'NONE',  ( -8.350000000000012079, 2.500000000000000000, 1.472243186433545459 ) ) ;
#56135 = CIRCLE ( 'NONE', #47652, 0.06509327318403745899 ) ;
#56136 = VERTEX_POINT ( 'NONE', #41916 ) ;
#56137 = CLOSED_SHELL ( 'NONE', ( #6996, #119013, #7002, #12005, #47034, #21334, #85328, #29069, #24387, #46124, #123627, #104998, #127169, #76353, #25927, #65525, #48372, #115425, #39012, #111285, #33928, #24746, #20525, #4934, #77923, #101654, #962, #103386, #64646, #18183, #46466, #40884, #113944, #5637, #100360, #78667 ) ) ;
#56138 = DIRECTION ( 'NONE',  ( 0.000000000000000000, 0.000000000000000000, 1.000000000000000000 ) ) ;
#56139 = VERTEX_POINT ( 'NONE', #22916 ) ;
#56140 = AXIS2_PLACEMENT_3D ( 'NONE', #126155, #75122, #5080 ) ;
#56141 = DIRECTION ( 'NONE',  ( 0.000000000000000000, -0.000000000000000000, -1.000000000000000000 ) ) ;
#56142 = DIRECTION ( 'NONE',  ( 0.000000000000000000, 0.000000000000000000, 1.000000000000000000 ) ) ;
#56143 = FACE_OUTER_BOUND ( 'NONE', #14911, .T. ) ;
#56144 = CARTESIAN_POINT ( 'NONE',  ( 20.69433222467931444, -2.585316282066745242, 4.139109617385087425 ) ) ;
#56145 = VERTEX_POINT ( 'NONE', #83130 ) ;
#56146 = AXIS2_PLACEMENT_3D ( 'NONE', #83652, #63362, #103293 ) ;
#56147 = PRESENTATION_LAYER_ASSIGNMENT (  '', '', ( #33199 ) ) ;
#56148 = ORIENTED_EDGE ( 'NONE', *, *, #52542, .F. ) ;
#56149 = EDGE_LOOP ( 'NONE', ( #13805, #19063, #109917, #40795 ) ) ;
#56150 = CARTESIAN_POINT ( 'NONE',  ( 1.049999999999954525, 12.50000000000000000, -2.511473670974877948 ) ) ;
#56151 = LINE ( 'NONE', #96087, #14266 ) ;
#56152 = DIRECTION ( 'NONE',  ( -0.000000000000000000, -1.000000000000000000, -0.000000000000000000 ) ) ;
#56153 = FACE_BOUND ( 'NONE', #97108, .T. ) ;
#56154 = FACE_OUTER_BOUND ( 'NONE', #80344, .T. ) ;
#56155 = DIRECTION ( 'NONE',  ( 0.000000000000000000, 1.000000000000000000, 0.000000000000000000 ) ) ;
#56156 = AXIS2_PLACEMENT_3D ( 'NONE', #97143, #68319, #7458 ) ;
#56157 = DIRECTION ( 'NONE',  ( 0.000000000000000000, -0.000000000000000000, 1.000000000000000000 ) ) ;
#56158 = FACE_OUTER_BOUND ( 'NONE', #12225, .T. ) ;
#56159 = CIRCLE ( 'NONE', #110546, 0.1000000000000002554 ) ;
#56160 = CARTESIAN_POINT ( 'NONE',  ( 185.0052083336747444, -6.551208109652278289, 3.782341765624995134 ) ) ;
#56161 = DIRECTION ( 'NONE',  ( -4.274815082592931898E-19, -0.9999939076577903929, -0.003490651415223739937 ) ) ;
#56162 = CIRCLE ( 'NONE', #35264, 0.1000000000000000472 ) ;
#56163 = DIRECTION ( 'NONE',  ( -0.000000000000000000, 1.000000000000000000, -0.000000000000000000 ) ) ;
#56164 = EDGE_CURVE ( 'NONE', #50689, #18883, #60894, .T. ) ;
#56165 = DIRECTION ( 'NONE',  ( 0.000000000000000000, 0.000000000000000000, -1.000000000000000000 ) ) ;
#56166 = AXIS2_PLACEMENT_3D ( 'NONE', #75311, #97528, #56941 ) ;
#56167 = VERTEX_POINT ( 'NONE', #93584 ) ;
#56168 = EDGE_LOOP ( 'NONE', ( #113014, #79162, #41762, #123618 ) ) ;
#56169 = VERTEX_POINT ( 'NONE', #32750 ) ;
#56170 = ORIENTED_EDGE ( 'NONE', *, *, #71914, .F. ) ;
#56171 = ADVANCED_FACE ( 'NONE', ( #61557 ), #72662, .F. ) ;
#56172 = CARTESIAN_POINT ( 'NONE',  ( 9.349999999999916156, 2.500000000000000000, 6.248780366869520542 ) ) ;
#56173 = FACE_BOUND ( 'NONE', #60042, .T. ) ;
#56174 = EDGE_CURVE ( 'NONE', #12327, #30034, #112265, .T. ) ;
#56175 = DIRECTION ( 'NONE',  ( -0.000000000000000000, -1.000000000000000000, -0.000000000000000000 ) ) ;
#56176 = DIRECTION ( 'NONE',  ( -0.000000000000000000, -1.000000000000000000, -0.000000000000000000 ) ) ;
#56178 = AXIS2_PLACEMENT_3D ( 'NONE', #67215, #16828, #26690 ) ;
#56177 = VECTOR ( 'NONE', #11010, 1000.000000000000000 ) ;
#56179 = ADVANCED_FACE ( 'NONE', ( #102741 ), #68338, .T. ) ;
#56180 = ADVANCED_FACE ( 'NONE', ( #91006 ), #55817, .T. ) ;
#56181 = ORIENTED_EDGE ( 'NONE', *, *, #72468, .T. ) ;
#56182 = DIRECTION ( 'NONE',  ( 0.000000000000000000, -0.000000000000000000, 1.000000000000000000 ) ) ;
#56183 = ADVANCED_FACE ( 'NONE', ( #3270 ), #111940, .T. ) ;
#56184 = DIRECTION ( 'NONE',  ( 0.000000000000000000, 1.000000000000000000, 0.000000000000000000 ) ) ;
#56185 = ADVANCED_FACE ( 'NONE', ( #91646 ), #1965, .T. ) ;
#56186 = EDGE_LOOP ( 'NONE', ( #107460, #91354, #35188, #68340 ) ) ;
#56187 = CARTESIAN_POINT ( 'NONE',  ( -6.505213034913026604E-15, 2.500000000000000000, 4.430127018922196847 ) ) ;
#56188 = DIRECTION ( 'NONE',  ( -0.000000000000000000, 1.000000000000000000, -0.000000000000000000 ) ) ;
#56189 = ORIENTED_EDGE ( 'NONE', *, *, #55152, .F. ) ;
#56190 = AXIS2_PLACEMENT_3D ( 'NONE', #45740, #36578, #47035 ) ;
#56191 = CARTESIAN_POINT ( 'NONE',  ( -12.94999999999999218, 12.50000000000000000, 2.165063509461101265 ) ) ;
#56193 = ADVANCED_FACE ( 'NONE', ( #7116 ), #59966, .T. ) ;
#56192 = DIRECTION ( 'NONE',  ( 0.000000000000000000, 0.000000000000000000, -1.000000000000000000 ) ) ;
#56194 = ORIENTED_EDGE ( 'NONE', *, *, #29482, .T. ) ;
#56195 = VECTOR ( 'NONE', #117122, 1000.000000000000000 ) ;
#56196 = DIRECTION ( 'NONE',  ( 0.000000000000000000, 0.000000000000000000, 1.000000000000000000 ) ) ;
#56197 = CIRCLE ( 'NONE', #12286, 0.06509327318403741736 ) ;
#56198 = CARTESIAN_POINT ( 'NONE',  ( 7.099999999999926814, 12.50000000000000000, -0.6928203230275541413 ) ) ;
#56199 = ORIENTED_EDGE ( 'NONE', *, *, #43095, .T. ) ;
#56200 = DIRECTION ( 'NONE',  ( 0.000000000000000000, 0.000000000000000000, 1.000000000000000000 ) ) ;
#56201 = EDGE_LOOP ( 'NONE', ( #14776, #103589 ) ) ;
#56202 = EDGE_LOOP ( 'NONE', ( #85358, #80108 ) ) ;
#56203 = DIRECTION ( 'NONE',  ( 0.000000000000000000, 0.000000000000000000, 1.000000000000000000 ) ) ;
#56205 = VERTEX_POINT ( 'NONE', #4521 ) ;
#56204 = VECTOR ( 'NONE', #110845, 1000.000000000000000 ) ;
#56206 = CARTESIAN_POINT ( 'NONE',  ( -0.2000000000000404232, 12.50000000000000000, 3.983716857408420964 ) ) ;
#56207 = CARTESIAN_POINT ( 'NONE',  ( 6.449999999999933564, 2.500000000000000000, -6.841600689897078702 ) ) ;
#56208 = AXIS2_PLACEMENT_3D ( 'NONE', #101985, #79756, #12294 ) ;
#56209 = ORIENTED_EDGE ( 'NONE', *, *, #83826, .T. ) ;
#56210 = CARTESIAN_POINT ( 'NONE',  ( 0.8499999999999550138, 12.50000000000000000, -5.802370205355749988 ) ) ;
#56211 = FACE_OUTER_BOUND ( 'NONE', #30632, .T. ) ;
#56212 = CARTESIAN_POINT ( 'NONE',  ( 10.59999999999990905, 2.500000000000000000, 4.083716857408420609 ) ) ;
#56213 = CARTESIAN_POINT ( 'NONE',  ( 194.5000000000000000, 0.000000000000000000, -5.000000000000000000 ) ) ;
#56214 = EDGE_CURVE ( 'NONE', #94677, #8342, #41179, .T. ) ;
#56215 = CARTESIAN_POINT ( 'NONE',  ( -8.750000000000008882, 2.500000000000000000, -2.857883832488653741 ) ) ;
#56216 = DIRECTION ( 'NONE',  ( -0.000000000000000000, -1.000000000000000000, -0.000000000000000000 ) ) ;
#56217 = AXIS2_PLACEMENT_3D ( 'NONE', #13491, #124749, #14137 ) ;
#56218 = VERTEX_POINT ( 'NONE', #54933 ) ;
#56220 = ORIENTED_EDGE ( 'NONE', *, *, #46316, .F. ) ;
#56219 = AXIS2_PLACEMENT_3D ( 'NONE', #94760, #43755, #3804 ) ;
#56221 = DIRECTION ( 'NONE',  ( -0.000000000000000000, -1.000000000000000000, -0.000000000000000000 ) ) ;
#56222 = DIRECTION ( 'NONE',  ( 0.000000000000000000, 0.000000000000000000, 1.000000000000000000 ) ) ;
#56224 = EDGE_CURVE ( 'NONE', #81996, #20105, #78829, .T. ) ;
#56223 = FACE_OUTER_BOUND ( 'NONE', #95994, .T. ) ;
#56226 = ORIENTED_EDGE ( 'NONE', *, *, #97191, .F. ) ;
#56225 = EDGE_LOOP ( 'NONE', ( #106936, #45975, #4885, #47615 ) ) ;
#56227 = ORIENTED_EDGE ( 'NONE', *, *, #54546, .T. ) ;
#56228 = ADVANCED_FACE ( 'NONE', ( #64755 ), #93385, .T. ) ;
#56229 = DIRECTION ( 'NONE',  ( -0.000000000000000000, 1.000000000000000000, -0.000000000000000000 ) ) ;
#56230 = EDGE_CURVE ( 'NONE', #10639, #39846, #123661, .T. ) ;
#56232 = DIRECTION ( 'NONE',  ( -0.000000000000000000, -1.000000000000000000, -0.000000000000000000 ) ) ;
#56231 = CIRCLE ( 'NONE', #89410, 0.06509327318403745899 ) ;
#56233 = DIRECTION ( 'NONE',  ( 0.000000000000000000, 1.000000000000000000, 0.000000000000000000 ) ) ;
#56234 = EDGE_CURVE ( 'NONE', #1556, #125732, #115121, .T. ) ;
#56235 = CARTESIAN_POINT ( 'NONE',  ( 0.000000000000000000, 0.000000000000000000, 0.000000000000000000 ) ) ;
#56236 = CARTESIAN_POINT ( 'NONE',  ( -12.89999999999999325, 2.500000000000000000, -3.537306695894647302 ) ) ;
#56237 = DIRECTION ( 'NONE',  ( -0.000000000000000000, -1.000000000000000000, -0.000000000000000000 ) ) ;
#56238 = LINE ( 'NONE', #126284, #56942 ) ;
#56239 = FACE_OUTER_BOUND ( 'NONE', #100566, .T. ) ;
#56240 = AXIS2_PLACEMENT_3D ( 'NONE', #27725, #27097, #36287 ) ;
#56241 = FACE_OUTER_BOUND ( 'NONE', #57042, .T. ) ;
#56242 = ADVANCED_FACE ( 'NONE', ( #95518 ), #104670, .T. ) ;
#56243 = CARTESIAN_POINT ( 'NONE',  ( -9.350000000000006750, 2.500000000000000000, 2.611473670974873151 ) ) ;
#56244 = ADVANCED_FACE ( 'NONE', ( #47070 ), #74603, .T. ) ;
#56246 = EDGE_LOOP ( 'NONE', ( #25767, #101916 ) ) ;
#56245 = ADVANCED_FACE ( 'NONE', ( #14986 ), #122722, .T. ) ;
#56247 = ADVANCED_FACE ( 'NONE', ( #125600 ), #75224, .T. ) ;
#56248 = AXIS2_PLACEMENT_3D ( 'NONE', #89432, #99905, #128743 ) ;
#56249 = CARTESIAN_POINT ( 'NONE',  ( 10.44999999999991402, 12.50000000000000000, -2.230156782645139391 ) ) ;
#56250 = VERTEX_POINT ( 'NONE', #96783 ) ;
#56251 = EDGE_LOOP ( 'NONE', ( #61672, #31455, #95750, #10937 ) ) ;
#56252 = DIRECTION ( 'NONE',  ( 0.000000000000000000, 1.000000000000000000, 0.000000000000000000 ) ) ;
#56253 = DIRECTION ( 'NONE',  ( -0.000000000000000000, -1.000000000000000000, -0.000000000000000000 ) ) ;
#56254 = AXIS2_PLACEMENT_3D ( 'NONE', #114684, #64933, #85234 ) ;
#56255 = DIRECTION ( 'NONE',  ( 0.000000000000000000, 0.000000000000000000, 1.000000000000000000 ) ) ;
#56256 = ADVANCED_FACE ( 'NONE', ( #5180 ), #36958, .T. ) ;
#56258 = VECTOR ( 'NONE', #126013, 1000.000000000000000 ) ;
#56257 = FACE_OUTER_BOUND ( 'NONE', #50579, .T. ) ;
#56259 = CARTESIAN_POINT ( 'NONE',  ( 185.2500000000000000, 9.429780353434619030E-16, -7.700000000000000178 ) ) ;
#56260 = DIRECTION ( 'NONE',  ( -0.000000000000000000, -1.000000000000000000, -0.000000000000000000 ) ) ;
#56261 = LINE ( 'NONE', #96179, #57294 ) ;
#56262 = VERTEX_POINT ( 'NONE', #94868 ) ;
#56263 = CARTESIAN_POINT ( 'NONE',  ( 10.39999999999990976, 12.50000000000000000, -4.395220292106239768 ) ) ;
#56264 = AXIS2_PLACEMENT_3D ( 'NONE', #125115, #15791, #36095 ) ;
#56265 = DIRECTION ( 'NONE',  ( 0.000000000000000000, -0.000000000000000000, 1.000000000000000000 ) ) ;
#56266 = ORIENTED_EDGE ( 'NONE', *, *, #74731, .F. ) ;
#56267 = VERTEX_POINT ( 'NONE', #14357 ) ;
#56269 = CONICAL_SURFACE ( 'NONE', #121025, 0.1000000000000000472, 0.003490658503988666988 ) ;
#56268 = CIRCLE ( 'NONE', #127297, 0.06509327318403745899 ) ;
#56270 = ORIENTED_EDGE ( 'NONE', *, *, #30073, .T. ) ;
#56271 = CONICAL_SURFACE ( 'NONE', #66730, 0.1000000000000000472, 0.003490658503988666988 ) ;
#56272 = ORIENTED_EDGE ( 'NONE', *, *, #33484, .F. ) ;
#56273 = CARTESIAN_POINT ( 'NONE',  ( 9.149999999999916866, 12.50000000000000000, -2.922977105672691422 ) ) ;
#56274 = CARTESIAN_POINT ( 'NONE',  ( 1.049999999999952083, 2.500000000000000000, 6.841600689897072485 ) ) ;
#56275 = AXIS2_PLACEMENT_3D ( 'NONE', #72423, #101877, #103158 ) ;
#56276 = DIRECTION ( 'NONE',  ( 0.000000000000000000, 0.000000000000000000, -1.000000000000000000 ) ) ;
#56277 = CARTESIAN_POINT ( 'NONE',  ( 17.50000000000000000, 0.9166666666666682950, -3.999999999999998224 ) ) ;
#56278 = DIRECTION ( 'NONE',  ( -0.000000000000000000, -1.000000000000000000, -0.000000000000000000 ) ) ;
#56279 = ORIENTED_EDGE ( 'NONE', *, *, #93295, .T. ) ;
#56280 = CARTESIAN_POINT ( 'NONE',  ( -1.250000000000037526, 2.500000000000000000, -1.472243186433550122 ) ) ;
#56281 = CARTESIAN_POINT ( 'NONE',  ( -8.550000000000013145, 2.500000000000000000, -1.718653347947326049 ) ) ;
#56282 = ORIENTED_EDGE ( 'NONE', *, *, #80124, .T. ) ;
#56283 = EDGE_CURVE ( 'NONE', #28419, #122300, #91324, .T. ) ;
#56284 = ORIENTED_EDGE ( 'NONE', *, *, #115591, .F. ) ;
#56285 = VERTEX_POINT ( 'NONE', #34682 ) ;
#56286 = VECTOR ( 'NONE', #97097, 1000.000000000000000 ) ;
#56287 = DIRECTION ( 'NONE',  ( 0.000000000000000000, 0.000000000000000000, 1.000000000000000000 ) ) ;
#56288 = DIRECTION ( 'NONE',  ( -0.000000000000000000, 1.000000000000000000, -0.000000000000000000 ) ) ;
#56289 = VECTOR ( 'NONE', #33919, 1000.000000000000000 ) ;
#56290 = VECTOR ( 'NONE', #18908, 1000.000000000000000 ) ;
#56291 = ORIENTED_EDGE ( 'NONE', *, *, #13608, .F. ) ;
#56292 = DIRECTION ( 'NONE',  ( 0.000000000000000000, 1.000000000000000000, 0.000000000000000000 ) ) ;
#56293 = CARTESIAN_POINT ( 'NONE',  ( -4.077824815344644402E-14, 2.500000000000000000, -5.122947341949753763 ) ) ;
#56294 = ADVANCED_FACE ( 'NONE', ( #44473 ), #66373, .T. ) ;
#56295 = CARTESIAN_POINT ( 'NONE',  ( 8.549999999999924327, 2.500000000000000000, 1.818653347947321475 ) ) ;
#56296 = DIRECTION ( 'NONE',  ( -0.000000000000000000, -1.000000000000000000, -0.000000000000000000 ) ) ;
#56297 = AXIS2_PLACEMENT_3D ( 'NONE', #26357, #64966, #37470 ) ;
#56298 = CONICAL_SURFACE ( 'NONE', #24920, 0.1000000000000002554, 0.003490658503988666988 ) ;
#56299 = VERTEX_POINT ( 'NONE', #126266 ) ;
#56300 = AXIS2_PLACEMENT_3D ( 'NONE', #85841, #76039, #116593 ) ;
#56301 = CARTESIAN_POINT ( 'NONE',  ( 7.099999999999928590, 12.50000000000000000, 3.637306695894644726 ) ) ;
#56302 = EDGE_LOOP ( 'NONE', ( #37693, #43897 ) ) ;
#56303 = EDGE_LOOP ( 'NONE', ( #43855, #85500, #52463, #36844 ) ) ;
#56304 = ORIENTED_EDGE ( 'NONE', *, *, #53272, .F. ) ;
#56305 = DIRECTION ( 'NONE',  ( -0.000000000000000000, 1.000000000000000000, -0.000000000000000000 ) ) ;
#56306 = FACE_BOUND ( 'NONE', #12812, .T. ) ;
#56307 = AXIS2_PLACEMENT_3D ( 'NONE', #90613, #111549, #62473 ) ;
#56308 = CARTESIAN_POINT ( 'NONE',  ( -13.34999999999999076, 12.50000000000000000, 1.472243186433549456 ) ) ;
#56309 = DIRECTION ( 'NONE',  ( 0.000000000000000000, 0.000000000000000000, -1.000000000000000000 ) ) ;
#56310 = DIRECTION ( 'NONE',  ( 0.000000000000000000, 0.000000000000000000, -1.000000000000000000 ) ) ;
#56311 = AXIS2_PLACEMENT_3D ( 'NONE', #114091, #94435, #83969 ) ;
#56312 = AXIS2_PLACEMENT_3D ( 'NONE', #48601, #46665, #40069 ) ;
#56313 = ORIENTED_EDGE ( 'NONE', *, *, #19435, .T. ) ;
#56314 = PLANE ( 'NONE',  #79800 ) ;
#56315 = CARTESIAN_POINT ( 'NONE',  ( 1.649999999999951061, 12.50000000000000000, -6.495190528383302464 ) ) ;
#56316 = DIRECTION ( 'NONE',  ( -0.000000000000000000, 1.000000000000000000, -0.000000000000000000 ) ) ;
#56317 = CARTESIAN_POINT ( 'NONE',  ( -1.650000000000034328, 2.500000000000000000, -2.857883832488653741 ) ) ;
#56318 = ORIENTED_EDGE ( 'NONE', *, *, #24924, .F. ) ;
#56319 = CARTESIAN_POINT ( 'NONE',  ( -1.900000000000034994, 2.500000000000000000, -4.676537180435978769 ) ) ;
#56320 = ADVANCED_FACE ( 'NONE', ( #36616 ), #51715, .T. ) ;
#56321 = DIRECTION ( 'NONE',  ( 0.000000000000000000, 1.000000000000000000, 0.000000000000000000 ) ) ;
#56322 = CIRCLE ( 'NONE', #73246, 0.06509327318403745899 ) ;
#56323 = ORIENTED_EDGE ( 'NONE', *, *, #5112, .T. ) ;
#56324 = FACE_OUTER_BOUND ( 'NONE', #57555, .T. ) ;
#56325 = FACE_BOUND ( 'NONE', #59472, .T. ) ;
#56326 = EDGE_CURVE ( 'NONE', #32792, #51798, #74585, .T. ) ;
#56327 = FACE_OUTER_BOUND ( 'NONE', #127407, .T. ) ;
#56328 = EDGE_LOOP ( 'NONE', ( #99953, #102247, #102392, #66458 ) ) ;
#56329 = CARTESIAN_POINT ( 'NONE',  ( -3.150000000000029665, 2.500000000000000000, 6.841600689897072485 ) ) ;
#56330 = DIRECTION ( 'NONE',  ( -0.000000000000000000, 1.000000000000000000, -0.000000000000000000 ) ) ;
#56331 = EDGE_CURVE ( 'NONE', #28423, #2568, #3676, .T. ) ;
#56332 = ORIENTED_EDGE ( 'NONE', *, *, #55767, .F. ) ;
#56333 = EDGE_CURVE ( 'NONE', #104821, #127509, #83111, .T. ) ;
#56334 = ORIENTED_EDGE ( 'NONE', *, *, #54461, .F. ) ;
#56336 = EDGE_CURVE ( 'NONE', #10701, #109829, #118598, .T. ) ;
#56335 = APPLICATION_CONTEXT ( 'automotive_design' ) ;
#56337 = ADVANCED_FACE ( 'NONE', ( #119655 ), #11995, .T. ) ;
#56338 = CARTESIAN_POINT ( 'NONE',  ( 184.0052083336747160, -6.551208109652278289, 3.782341765624995134 ) ) ;
#56339 = ADVANCED_FACE ( 'NONE', ( #27394 ), #67304, .T. ) ;
#56340 = VERTEX_POINT ( 'NONE', #60125 ) ;
#56341 = CARTESIAN_POINT ( 'NONE',  ( 185.5052083336747444, -6.551208109652278289, 3.782341765624995134 ) ) ;
#56342 = CARTESIAN_POINT ( 'NONE',  ( -7.100000000000018296, 12.50000000000000000, -4.265033745738164406 ) ) ;
#56343 = CARTESIAN_POINT ( 'NONE',  ( 1.249999999999988454, 2.500000000000000000, 2.065063509461097624 ) ) ;
#56344 = LINE ( 'NONE', #60083, #25926 ) ;
#56345 = CARTESIAN_POINT ( 'NONE',  ( 8.099999999999921485, 2.500000000000000000, 0.4464101615137735513 ) ) ;
#56346 = AXIS2_PLACEMENT_3D ( 'NONE', #30340, #39524, #121276 ) ;
#56347 = ADVANCED_FACE ( 'NONE', ( #47714 ), #91411, .T. ) ;
#56348 = ADVANCED_FACE ( 'NONE', ( #87615 ), #30009, .T. ) ;
#56349 = ADVANCED_FACE ( 'NONE', ( #37253 ), #76750, .T. ) ;
#56350 = VERTEX_POINT ( 'NONE', #126916 ) ;
#56351 = DIRECTION ( 'NONE',  ( 0.000000000000000000, 0.000000000000000000, -1.000000000000000000 ) ) ;
#56352 = AXIS2_PLACEMENT_3D ( 'NONE', #107147, #28611, #17471 ) ;
#56353 = DIRECTION ( 'NONE',  ( 0.000000000000000000, -0.9999939076577903929, 0.003490651415223739937 ) ) ;
#56354 = DIRECTION ( 'NONE',  ( 0.000000000000000000, -0.9999939076577903929, 0.003490651415223739937 ) ) ;
#56355 = DIRECTION ( 'NONE',  ( -4.274815082592931898E-19, -0.9999939076577903929, -0.003490651415223739937 ) ) ;
#56356 = AXIS2_PLACEMENT_3D ( 'NONE', #87898, #68269, #57824 ) ;
#56358 = ORIENTED_EDGE ( 'NONE', *, *, #26004, .T. ) ;
#56357 = ORIENTED_EDGE ( 'NONE', *, *, #9231, .T. ) ;
#56359 = FACE_BOUND ( 'NONE', #43598, .T. ) ;
#56360 = ORIENTED_EDGE ( 'NONE', *, *, #123838, .F. ) ;
#56361 = FACE_OUTER_BOUND ( 'NONE', #5827, .T. ) ;
#56362 = DIRECTION ( 'NONE',  ( -0.000000000000000000, 1.000000000000000000, -0.000000000000000000 ) ) ;
#56363 = ORIENTED_EDGE ( 'NONE', *, *, #52533, .F. ) ;
#56364 = DIRECTION ( 'NONE',  ( 0.000000000000000000, 0.000000000000000000, 1.000000000000000000 ) ) ;
#56367 = FACE_OUTER_BOUND ( 'NONE', #73447, .T. ) ;
#56366 = AXIS2_PLACEMENT_3D ( 'NONE', #81902, #100271, #10576 ) ;
#56365 =( GEOMETRIC_REPRESENTATION_CONTEXT ( 3 ) GLOBAL_UNCERTAINTY_ASSIGNED_CONTEXT ( ( #64969 ) ) GLOBAL_UNIT_ASSIGNED_CONTEXT ( ( #129393, #51462, #50174 ) ) REPRESENTATION_CONTEXT ( 'NONE', 'WORKASPACE' ) );
#56368 = CARTESIAN_POINT ( 'NONE',  ( 8.349999999999919709, 12.50000000000000000, -2.857883832488653741 ) ) ;
#56369 = CARTESIAN_POINT ( 'NONE',  ( -14.39999999999998614, 2.500000000000000000, 0.3464101615137758494 ) ) ;
#56370 = ORIENTED_EDGE ( 'NONE', *, *, #116910, .F. ) ;
#56371 = DIRECTION ( 'NONE',  ( -0.000000000000000000, 1.000000000000000000, -0.000000000000000000 ) ) ;
#56372 = CARTESIAN_POINT ( 'NONE',  ( -7.950000000000016165, 2.500000000000000000, -6.595190528383296780 ) ) ;
#56373 = CARTESIAN_POINT ( 'NONE',  ( 186.6927083336747160, 6.551208109652275624, -3.782341765624998686 ) ) ;
#56374 = DIRECTION ( 'NONE',  ( -0.000000000000000000, -1.000000000000000000, -0.000000000000000000 ) ) ;
#56375 = CARTESIAN_POINT ( 'NONE',  ( -4.600000000000025402, 2.500000000000000000, 4.430127018922196847 ) ) ;
#56376 = EDGE_LOOP ( 'NONE', ( #27425, #31906 ) ) ;
#56377 = ORIENTED_EDGE ( 'NONE', *, *, #120361, .T. ) ;
#56378 = DIRECTION ( 'NONE',  ( 0.000000000000000000, 0.000000000000000000, 1.000000000000000000 ) ) ;
#56379 = EDGE_LOOP ( 'NONE', ( #42246, #33433, #34628, #64858 ) ) ;
#56380 = DIRECTION ( 'NONE',  ( -0.000000000000000000, 1.000000000000000000, -0.000000000000000000 ) ) ;
#56382 = ORIENTED_EDGE ( 'NONE', *, *, #85065, .T. ) ;
#56381 = ORIENTED_EDGE ( 'NONE', *, *, #57235, .F. ) ;
#56383 = EDGE_LOOP ( 'NONE', ( #118033, #109413 ) ) ;
#56384 = DIRECTION ( 'NONE',  ( -0.000000000000000000, -1.000000000000000000, -0.000000000000000000 ) ) ;
#56385 = VECTOR ( 'NONE', #41520, 1000.000000000000000 ) ;
#56386 = DIRECTION ( 'NONE',  ( 0.000000000000000000, 0.000000000000000000, 1.000000000000000000 ) ) ;
#56387 = CIRCLE ( 'NONE', #100223, 0.06509327318403745899 ) ;
#56388 = CARTESIAN_POINT ( 'NONE',  ( 10.59999999999991260, 12.50000000000000000, -0.3464101615137783474 ) ) ;
#56389 = DIRECTION ( 'NONE',  ( 0.000000000000000000, 0.000000000000000000, 1.000000000000000000 ) ) ;
#56390 = CARTESIAN_POINT ( 'NONE',  ( 8.099999999999923261, 2.500000000000000000, -4.576537180435978236 ) ) ;
#56391 = CARTESIAN_POINT ( 'NONE',  ( 175.5000000000000000, 0.000000000000000000, -4.000000000000000000 ) ) ;
#56392 = ORIENTED_EDGE ( 'NONE', *, *, #109077, .F. ) ;
#56393 = EDGE_CURVE ( 'NONE', #64447, #101569, #108558, .T. ) ;
#56396 = CONICAL_SURFACE ( 'NONE', #89848, 0.1000000000000002554, 0.003490658503988666988 ) ;
#56395 = PLANE ( 'NONE',  #28859 ) ;
#56394 = AXIS2_PLACEMENT_3D ( 'NONE', #128736, #79606, #100522 ) ;
#56397 = EDGE_LOOP ( 'NONE', ( #91635, #23882 ) ) ;
#56398 = EDGE_CURVE ( 'NONE', #47981, #114315, #9940, .T. ) ;
#56399 = EDGE_LOOP ( 'NONE', ( #61112, #111792, #10278, #27042 ) ) ;
#56400 = ORIENTED_EDGE ( 'NONE', *, *, #6078, .T. ) ;
#56401 = ORIENTED_EDGE ( 'NONE', *, *, #85061, .T. ) ;
#56402 = ADVANCED_FACE ( 'NONE', ( #38556 ), #89368, .T. ) ;
#56403 = CARTESIAN_POINT ( 'NONE',  ( -11.64999999999999680, 12.50000000000000000, -2.857883832488649745 ) ) ;
#56404 = ORIENTED_EDGE ( 'NONE', *, *, #89620, .T. ) ;
#56405 = EDGE_LOOP ( 'NONE', ( #69659, #93201, #127406, #45217 ) ) ;
#56406 = AXIS2_PLACEMENT_3D ( 'NONE', #128482, #38827, #17854 ) ;
#56407 = EDGE_CURVE ( 'NONE', #37781, #119461, #95622, .T. ) ;
#56408 = AXIS2_PLACEMENT_3D ( 'NONE', #59709, #90409, #748 ) ;
#56409 = LINE ( 'NONE', #65588, #51912 ) ;
#56410 = CARTESIAN_POINT ( 'NONE',  ( 1.849999999999949685, 2.500000000000000000, 1.818653347947321475 ) ) ;
#56411 = AXIS2_PLACEMENT_3D ( 'NONE', #74678, #73378, #114589 ) ;
#56412 = CARTESIAN_POINT ( 'NONE',  ( -0.4000000000000339950, 2.500000000000000000, 0.6928203230275518099 ) ) ;
#56413 = CARTESIAN_POINT ( 'NONE',  ( 8.749999999999920064, 2.500000000000000000, -2.757883832488654097 ) ) ;
#56414 = PLANE ( 'NONE',  #94756 ) ;
#56415 = VERTEX_POINT ( 'NONE', #67975 ) ;
#56416 = LINE ( 'NONE', #100685, #88954 ) ;
#56417 = VECTOR ( 'NONE', #16187, 1000.000000000000000 ) ;
#56418 = ORIENTED_EDGE ( 'NONE', *, *, #89783, .F. ) ;
#56419 = FACE_OUTER_BOUND ( 'NONE', #14253, .T. ) ;
#56420 = ORIENTED_EDGE ( 'NONE', *, *, #114497, .F. ) ;
#56421 = FACE_OUTER_BOUND ( 'NONE', #38778, .T. ) ;
#56422 = CONICAL_SURFACE ( 'NONE', #123247, 0.1000000000000000472, 0.003490658503988666988 ) ;
#56423 = VERTEX_POINT ( 'NONE', #107909 ) ;
#56424 = ADVANCED_FACE ( 'NONE', ( #29367 ), #43416, .T. ) ;
#56425 = ORIENTED_EDGE ( 'NONE', *, *, #67377, .T. ) ;
#56426 = DIRECTION ( 'NONE',  ( 0.000000000000000000, -0.9999939076577903929, 0.003490651415223739937 ) ) ;
#56427 = DIRECTION ( 'NONE',  ( 0.000000000000000000, 0.000000000000000000, -1.000000000000000000 ) ) ;
#56428 = CARTESIAN_POINT ( 'NONE',  ( -2.100000000000033396, 2.500000000000000000, -3.737306695894649700 ) ) ;
#56429 = DIRECTION ( 'NONE',  ( 0.000000000000000000, 0.000000000000000000, 1.000000000000000000 ) ) ;
#56430 = DIRECTION ( 'NONE',  ( 0.000000000000000000, 0.000000000000000000, 1.000000000000000000 ) ) ;
#56431 = EDGE_LOOP ( 'NONE', ( #113702, #67267, #45599, #79784 ) ) ;
#56432 = DIRECTION ( 'NONE',  ( -4.274815082592931898E-19, -0.9999939076577903929, -0.003490651415223739937 ) ) ;
#56433 = CARTESIAN_POINT ( 'NONE',  ( -6.650000000000015454, 2.500000000000000000, 7.188010851410848723 ) ) ;
#56434 = DIRECTION ( 'NONE',  ( 0.000000000000000000, 0.000000000000000000, 1.000000000000000000 ) ) ;
#56435 = DIRECTION ( 'NONE',  ( 0.000000000000000000, 1.000000000000000000, 0.000000000000000000 ) ) ;
#56436 = CARTESIAN_POINT ( 'NONE',  ( 7.099999999999926814, 2.500000000000000000, -0.6928203230275541413 ) ) ;
#56437 = EDGE_LOOP ( 'NONE', ( #44590, #81396, #52527 ) ) ;
#56438 = ADVANCED_FACE ( 'NONE', ( #69259 ), #62187, .T. ) ;
#56439 = ORIENTED_EDGE ( 'NONE', *, *, #81594, .F. ) ;
#56440 = EDGE_CURVE ( 'NONE', #16833, #113875, #5717, .T. ) ;
#56441 = DIRECTION ( 'NONE',  ( -0.000000000000000000, 1.000000000000000000, -0.000000000000000000 ) ) ;
#56442 = VECTOR ( 'NONE', #9065, 1000.000000000000000 ) ;
#56443 = VERTEX_POINT ( 'NONE', #48346 ) ;
#56444 = CARTESIAN_POINT ( 'NONE',  ( -10.45000000000000107, 2.500000000000000000, 6.595190528383296780 ) ) ;
#56445 = LINE ( 'NONE', #7987, #4162 ) ;
#56447 = CIRCLE ( 'NONE', #35546, 0.06509327318403745899 ) ;
#56446 = AXIS2_PLACEMENT_3D ( 'NONE', #106359, #16664, #87987 ) ;
#56448 = ORIENTED_EDGE ( 'NONE', *, *, #100409, .F. ) ;
#56449 = CARTESIAN_POINT ( 'NONE',  ( 186.5833333333333144, -6.668395609140180369, 3.849999999999994760 ) ) ;
#56450 = CARTESIAN_POINT ( 'NONE',  ( -0.6000000000000388356, 12.50000000000000000, 4.741630453620009789 ) ) ;
#56451 = FACE_OUTER_BOUND ( 'NONE', #104451, .T. ) ;
#56452 = EDGE_CURVE ( 'NONE', #114810, #112120, #97673, .T. ) ;
#56453 = CARTESIAN_POINT ( 'NONE',  ( 2.099999999999950351, 2.500000000000000000, -2.276824562219559311E-15 ) ) ;
#56454 = DIRECTION ( 'NONE',  ( -0.000000000000000000, -1.000000000000000000, -0.000000000000000000 ) ) ;
#56455 = ORIENTED_EDGE ( 'NONE', *, *, #26804, .F. ) ;
#56456 = AXIS2_PLACEMENT_3D ( 'NONE', #68069, #66136, #107349 ) ;
#56457 = CARTESIAN_POINT ( 'NONE',  ( 12.29999999999990656, 12.50000000000000000, -4.676537180435977881 ) ) ;
#56458 = FACE_OUTER_BOUND ( 'NONE', #126107, .T. ) ;
#56459 = ORIENTED_EDGE ( 'NONE', *, *, #117371, .F. ) ;
#56460 = DIRECTION ( 'NONE',  ( 0.000000000000000000, -0.000000000000000000, -1.000000000000000000 ) ) ;
#56461 = CARTESIAN_POINT ( 'NONE',  ( -14.14999999999998614, 2.500000000000000000, -2.065063509461099844 ) ) ;
#56462 = CARTESIAN_POINT ( 'NONE',  ( 4.599999999999938360, 2.500000000000000000, -0.7928203230275542301 ) ) ;
#56463 = ORIENTED_EDGE ( 'NONE', *, *, #35673, .T. ) ;
#56464 = DIRECTION ( 'NONE',  ( 0.000000000000000000, 0.000000000000000000, 1.000000000000000000 ) ) ;
#56465 = ORIENTED_EDGE ( 'NONE', *, *, #60048, .F. ) ;
#56466 = DIRECTION ( 'NONE',  ( 0.000000000000000000, 1.000000000000000000, 0.000000000000000000 ) ) ;
#56467 = CARTESIAN_POINT ( 'NONE',  ( 4.149999999999939959, 12.50000000000000000, 1.472243186433545459 ) ) ;
#56468 = FACE_OUTER_BOUND ( 'NONE', #49997, .T. ) ;
#56469 = ORIENTED_EDGE ( 'NONE', *, *, #68784, .T. ) ;
#56470 = VECTOR ( 'NONE', #6461, 1000.000000000000000 ) ;
#56471 = FACE_OUTER_BOUND ( 'NONE', #15577, .T. ) ;
#56472 = CIRCLE ( 'NONE', #47, 0.06509327318403745899 ) ;
#56473 = EDGE_CURVE ( 'NONE', #107710, #116926, #116539, .T. ) ;
#56474 = DIRECTION ( 'NONE',  ( -0.000000000000000000, 1.000000000000000000, -0.000000000000000000 ) ) ;
#56475 = EDGE_LOOP ( 'NONE', ( #62284, #8024, #10350, #35159 ) ) ;
#56476 = ORIENTED_EDGE ( 'NONE', *, *, #8216, .T. ) ;
#56477 = VECTOR ( 'NONE', #40559, 1000.000000000000000 ) ;
#56478 = CARTESIAN_POINT ( 'NONE',  ( -1.450000000000035039, 2.500000000000000000, -2.611473670974877592 ) ) ;
#56479 = EDGE_CURVE ( 'NONE', #23072, #94071, #41259, .T. ) ;
#56480 = VERTEX_POINT ( 'NONE', #31940 ) ;
#56481 = CARTESIAN_POINT ( 'NONE',  ( 187.5000000000000000, 0.000000000000000000, 0.000000000000000000 ) ) ;
#56482 = DIRECTION ( 'NONE',  ( -0.000000000000000000, -1.000000000000000000, -0.000000000000000000 ) ) ;
#56483 = ADVANCED_FACE ( 'NONE', ( #92123 ), #81040, .T. ) ;
#56484 = EDGE_LOOP ( 'NONE', ( #43300, #22670 ) ) ;
#56485 = EDGE_CURVE ( 'NONE', #108498, #41959, #20827, .T. ) ;
#56486 = VERTEX_POINT ( 'NONE', #40483 ) ;
#56487 = EDGE_CURVE ( 'NONE', #104378, #113501, #20316, .T. ) ;
#56489 = ADVANCED_FACE ( 'NONE', ( #71203 ), #114391, .T. ) ;
#56488 = CIRCLE ( 'NONE', #60640, 0.09999999999999999167 ) ;
#56490 = DIRECTION ( 'NONE',  ( 0.000000000000000000, 0.000000000000000000, 1.000000000000000000 ) ) ;
#56491 = DIRECTION ( 'NONE',  ( -0.000000000000000000, -1.000000000000000000, -0.000000000000000000 ) ) ;
#56492 = ORIENTED_EDGE ( 'NONE', *, *, #34230, .F. ) ;
#56494 = DIRECTION ( 'NONE',  ( 0.000000000000000000, 0.000000000000000000, 1.000000000000000000 ) ) ;
#56493 = AXIS2_PLACEMENT_3D ( 'NONE', #71413, #72092, #111332 ) ;
#56495 = LINE ( 'NONE', #96412, #43071 ) ;
#56496 = CONICAL_SURFACE ( 'NONE', #98350, 0.1000000000000002554, 0.003490658503988666988 ) ;
#56497 = EDGE_CURVE ( 'NONE', #121356, #33416, #57977, .T. ) ;
#56498 = DIRECTION ( 'NONE',  ( 0.000000000000000000, 1.000000000000000000, 0.000000000000000000 ) ) ;
#56499 = DIRECTION ( 'NONE',  ( 0.000000000000000000, 0.000000000000000000, 1.000000000000000000 ) ) ;
#56500 = EDGE_CURVE ( 'NONE', #24462, #6208, #120670, .T. ) ;
#56501 = DIRECTION ( 'NONE',  ( 0.000000000000000000, 1.000000000000000000, 0.000000000000000000 ) ) ;
#56502 = LINE ( 'NONE', #57156, #96398 ) ;
#56503 = EDGE_CURVE ( 'NONE', #40225, #92121, #126935, .T. ) ;
#56504 = AXIS2_PLACEMENT_3D ( 'NONE', #89652, #109943, #70016 ) ;
#56505 = ADVANCED_FACE ( 'NONE', ( #111786 ), #122896, .T. ) ;
#56506 = ADVANCED_FACE ( 'NONE', ( #61403 ), #101962, .T. ) ;
#56507 = EDGE_LOOP ( 'NONE', ( #94777, #119047, #126480, #87766 ) ) ;
#56508 = EDGE_LOOP ( 'NONE', ( #25913, #5093, #1097, #74051 ) ) ;
#56509 = EDGE_LOOP ( 'NONE', ( #95108, #105896, #31580, #112380 ) ) ;
#56510 = EDGE_LOOP ( 'NONE', ( #128945, #120750, #50255, #41568 ) ) ;
#56511 = VECTOR ( 'NONE', #74690, 1000.000000000000000 ) ;
#56512 = CARTESIAN_POINT ( 'NONE',  ( -11.69999999999999574, 2.500000000000000000, 4.330127018922196314 ) ) ;
#56513 = DIRECTION ( 'NONE',  ( 0.000000000000000000, 0.000000000000000000, 1.000000000000000000 ) ) ;
#56514 = CARTESIAN_POINT ( 'NONE',  ( -12.29999999999999716, 12.50000000000000000, 0.2813168883297402778 ) ) ;
#56515 = ORIENTED_EDGE ( 'NONE', *, *, #78521, .T. ) ;
#56516 = FACE_BOUND ( 'NONE', #113186, .T. ) ;
#56517 = ADVANCED_FACE ( 'NONE', ( #112435 ), #11642, .T. ) ;
#56518 = DIRECTION ( 'NONE',  ( 0.000000000000000000, -0.9999939076577903929, 0.003490651415223739937 ) ) ;
#56519 = CARTESIAN_POINT ( 'NONE',  ( -8.749999999999975131, 12.50000000000000000, 2.165063509461097713 ) ) ;
#56520 = DIRECTION ( 'NONE',  ( 0.000000000000000000, 1.000000000000000000, 0.000000000000000000 ) ) ;
#56521 = CARTESIAN_POINT ( 'NONE',  ( -5.000000000000022204, 12.50000000000000000, 3.637306695894644726 ) ) ;
#56522 = CARTESIAN_POINT ( 'NONE',  ( 15.83209681635555022, -2.500000000000000000, -5.404881881984138658 ) ) ;
#56523 = DIRECTION ( 'NONE',  ( 0.000000000000000000, 0.000000000000000000, 1.000000000000000000 ) ) ;
#56524 = DIRECTION ( 'NONE',  ( -0.000000000000000000, -1.000000000000000000, -0.000000000000000000 ) ) ;
#56525 = DIRECTION ( 'NONE',  ( -0.000000000000000000, -1.000000000000000000, -0.000000000000000000 ) ) ;
#56526 = CARTESIAN_POINT ( 'NONE',  ( 2.899999999999945732, 12.50000000000000000, -4.330127018922201643 ) ) ;
#56527 = DIRECTION ( 'NONE',  ( 0.000000000000000000, 0.000000000000000000, 1.000000000000000000 ) ) ;
#56528 = EDGE_LOOP ( 'NONE', ( #108999, #48155 ) ) ;
#56529 = ORIENTED_EDGE ( 'NONE', *, *, #72266, .F. ) ;
#56530 = EDGE_LOOP ( 'NONE', ( #88753, #11486 ) ) ;
#56531 = ORIENTED_EDGE ( 'NONE', *, *, #16182, .F. ) ;
#56532 = DIRECTION ( 'NONE',  ( -0.000000000000000000, -1.000000000000000000, -0.000000000000000000 ) ) ;
#56533 = VECTOR ( 'NONE', #50149, 1000.000000000000000 ) ;
#56534 = CARTESIAN_POINT ( 'NONE',  ( 9.149999999999920419, 2.500000000000000000, 1.472243186433545459 ) ) ;
#56536 = EDGE_CURVE ( 'NONE', #94526, #44317, #124871, .T. ) ;
#56535 = AXIS2_PLACEMENT_3D ( 'NONE', #73150, #113059, #33857 ) ;
#56537 = ORIENTED_EDGE ( 'NONE', *, *, #89485, .F. ) ;
#56538 = ORIENTED_EDGE ( 'NONE', *, *, #10269, .F. ) ;
#56539 = DIRECTION ( 'NONE',  ( 0.000000000000000000, 1.000000000000000000, 0.000000000000000000 ) ) ;
#56540 = CIRCLE ( 'NONE', #60676, 0.1000000000000002554 ) ;
#56541 = DIRECTION ( 'NONE',  ( 0.000000000000000000, 0.000000000000000000, 1.000000000000000000 ) ) ;
#56542 = DIRECTION ( 'NONE',  ( 0.000000000000000000, 0.000000000000000000, 1.000000000000000000 ) ) ;
#56543 = CARTESIAN_POINT ( 'NONE',  ( -12.04999999999999716, 2.500000000000000000, -2.265063509461097802 ) ) ;
#56544 = FACE_OUTER_BOUND ( 'NONE', #29392, .T. ) ;
#56545 = ORIENTED_EDGE ( 'NONE', *, *, #14656, .F. ) ;
#56546 = ORIENTED_EDGE ( 'NONE', *, *, #6883, .F. ) ;
#56547 = EDGE_CURVE ( 'NONE', #89132, #98092, #62692, .T. ) ;
#56548 = ORIENTED_EDGE ( 'NONE', *, *, #113132, .T. ) ;
#56549 = ORIENTED_EDGE ( 'NONE', *, *, #64205, .T. ) ;
#56550 = ADVANCED_FACE ( 'NONE', ( #100652 ), #39314, .T. ) ;
#56551 = CARTESIAN_POINT ( 'NONE',  ( -11.64999999999999680, 2.500000000000000000, 6.395190528383296602 ) ) ;
#56552 = EDGE_LOOP ( 'NONE', ( #114416, #28569 ) ) ;
#56553 = ORIENTED_EDGE ( 'NONE', *, *, #6504, .T. ) ;
#56554 = CARTESIAN_POINT ( 'NONE',  ( -4.800000000000022915, 2.500000000000000000, -0.4464101615137783252 ) ) ;
#56555 = EDGE_CURVE ( 'NONE', #2822, #74443, #10975, .T. ) ;
#56556 = DIRECTION ( 'NONE',  ( -0.000000000000000000, 1.000000000000000000, -0.000000000000000000 ) ) ;
#56557 = CARTESIAN_POINT ( 'NONE',  ( -4.600000000000024514, 2.500000000000000000, 3.537306695894645081 ) ) ;
#56558 = FACE_OUTER_BOUND ( 'NONE', #17782, .T. ) ;
#56559 = DIRECTION ( 'NONE',  ( 0.000000000000000000, -0.000000000000000000, 1.000000000000000000 ) ) ;
#56560 = ORIENTED_EDGE ( 'NONE', *, *, #56624, .T. ) ;
#56561 = LINE ( 'NONE', #93929, #44867 ) ;
#56562 = AXIS2_PLACEMENT_3D ( 'NONE', #119221, #127754, #38086 ) ;
#56563 = AXIS2_PLACEMENT_3D ( 'NONE', #44997, #84905, #113071 ) ;
#56564 = ORIENTED_EDGE ( 'NONE', *, *, #36495, .F. ) ;
#56565 = CARTESIAN_POINT ( 'NONE',  ( 8.349999999999923261, 12.50000000000000000, 2.857883832488649301 ) ) ;
#56566 = ORIENTED_EDGE ( 'NONE', *, *, #55778, .T. ) ;
#56567 = DIRECTION ( 'NONE',  ( -0.000000000000000000, 1.000000000000000000, -0.000000000000000000 ) ) ;
#56568 = FACE_OUTER_BOUND ( 'NONE', #77928, .T. ) ;
#56569 = ORIENTED_EDGE ( 'NONE', *, *, #56126, .F. ) ;
#56570 = DIRECTION ( 'NONE',  ( 0.000000000000000000, 0.000000000000000000, -1.000000000000000000 ) ) ;
#56571 = LINE ( 'NONE', #37608, #22962 ) ;
#56572 = ORIENTED_EDGE ( 'NONE', *, *, #83952, .T. ) ;
#56573 = CONICAL_SURFACE ( 'NONE', #60797, 0.09999999999999982514, 0.003490658503988666988 ) ;
#56574 = CARTESIAN_POINT ( 'NONE',  ( 0.6499999999999543920, 2.500000000000000000, 6.148780366869520897 ) ) ;
#56575 = VERTEX_POINT ( 'NONE', #111105 ) ;
#56576 = VERTEX_POINT ( 'NONE', #91491 ) ;
#56577 = DIRECTION ( 'NONE',  ( 0.000000000000000000, 1.000000000000000000, 0.000000000000000000 ) ) ;
#56578 = FACE_OUTER_BOUND ( 'NONE', #16622, .T. ) ;
#56579 = CARTESIAN_POINT ( 'NONE',  ( 185.7968750003414300, 8.734944146203032389, 5.348610694689227483E-16 ) ) ;
#56580 = FACE_OUTER_BOUND ( 'NONE', #1505, .T. ) ;
#56582 = ADVANCED_FACE ( 'NONE', ( #21463 ), #84891, .T. ) ;
#56581 = AXIS2_PLACEMENT_3D ( 'NONE', #68694, #60188, #28137 ) ;
#56583 = CIRCLE ( 'NONE', #81723, 0.06509327318403745899 ) ;
#56584 = CARTESIAN_POINT ( 'NONE',  ( 3.749999999999944045, 12.50000000000000000, -2.857883832488653741 ) ) ;
#56585 = CARTESIAN_POINT ( 'NONE',  ( -10.80000000000000071, 2.500000000000000000, 0.09999999999999772959 ) ) ;
#56586 = EDGE_CURVE ( 'NONE', #82277, #39657, #99923, .T. ) ;
#56587 = AXIS2_PLACEMENT_3D ( 'NONE', #94803, #105265, #46337 ) ;
#56588 = ORIENTED_EDGE ( 'NONE', *, *, #35487, .F. ) ;
#56589 = PLANE ( 'NONE',  #15062 ) ;
#56590 = VERTEX_POINT ( 'NONE', #105824 ) ;
#56591 = AXIS2_PLACEMENT_3D ( 'NONE', #112543, #91599, #1281 ) ;
#56592 = EDGE_CURVE ( 'NONE', #99284, #49008, #43499, .T. ) ;
#56593 = FACE_OUTER_BOUND ( 'NONE', #682, .T. ) ;
#56594 = DIRECTION ( 'NONE',  ( 0.000000000000000000, 1.000000000000000000, 0.000000000000000000 ) ) ;
#56595 = CARTESIAN_POINT ( 'NONE',  ( 4.599999999999938360, 12.50000000000000000, -0.6277270498435166823 ) ) ;
#56596 = EDGE_CURVE ( 'NONE', #119631, #30265, #3775, .T. ) ;
#56597 = DIRECTION ( 'NONE',  ( 0.000000000000000000, 1.000000000000000000, 0.000000000000000000 ) ) ;
#56598 = DIRECTION ( 'NONE',  ( 0.000000000000000000, 0.000000000000000000, 1.000000000000000000 ) ) ;
#56599 = ORIENTED_EDGE ( 'NONE', *, *, #61385, .F. ) ;
#56600 = DIRECTION ( 'NONE',  ( 0.000000000000000000, 1.000000000000000000, 0.000000000000000000 ) ) ;
#56601 = CARTESIAN_POINT ( 'NONE',  ( 2.899999999999946620, 12.50000000000000000, -0.6277270498435167934 ) ) ;
#56602 = EDGE_CURVE ( 'NONE', #120278, #33691, #76851, .T. ) ;
#56603 = ORIENTED_EDGE ( 'NONE', *, *, #107788, .T. ) ;
#56604 = DIRECTION ( 'NONE',  ( 0.000000000000000000, -0.000000000000000000, 1.000000000000000000 ) ) ;
#56605 = ORIENTED_EDGE ( 'NONE', *, *, #126109, .T. ) ;
#56606 = ORIENTED_EDGE ( 'NONE', *, *, #78843, .T. ) ;
#56607 = DIRECTION ( 'NONE',  ( 0.000000000000000000, 0.000000000000000000, -1.000000000000000000 ) ) ;
#56608 = AXIS2_PLACEMENT_3D ( 'NONE', #115466, #79294, #110036 ) ;
#56609 = CIRCLE ( 'NONE', #37847, 0.06509327318403745899 ) ;
#56610 = CIRCLE ( 'NONE', #186, 0.1000000000000002554 ) ;
#56611 = EDGE_LOOP ( 'NONE', ( #3424, #118367, #74026, #5015 ) ) ;
#56612 = FACE_OUTER_BOUND ( 'NONE', #18933, .T. ) ;
#56613 = DIRECTION ( 'NONE',  ( 0.000000000000000000, -0.9999939076577903929, 0.003490651415223739937 ) ) ;
#56614 = FACE_OUTER_BOUND ( 'NONE', #53744, .T. ) ;
#56615 = VERTEX_POINT ( 'NONE', #55436 ) ;
#56617 = FACE_BOUND ( 'NONE', #78064, .T. ) ;
#56616 = AXIS2_PLACEMENT_3D ( 'NONE', #57104, #78038, #25710 ) ;
#56619 = ORIENTED_EDGE ( 'NONE', *, *, #32582, .T. ) ;
#56618 = DIRECTION ( 'NONE',  ( 0.000000000000000000, 0.000000000000000000, -1.000000000000000000 ) ) ;
#56620 = CIRCLE ( 'NONE', #92148, 0.06509327318403745899 ) ;
#56621 = CARTESIAN_POINT ( 'NONE',  ( -8.750000000000012434, 2.500000000000000000, -5.802370205355744659 ) ) ;
#56622 = DIRECTION ( 'NONE',  ( 0.000000000000000000, 0.000000000000000000, -1.000000000000000000 ) ) ;
#56623 = ORIENTED_EDGE ( 'NONE', *, *, #63436, .F. ) ;
#56624 = EDGE_CURVE ( 'NONE', #23431, #10632, #26757, .T. ) ;
#56625 = EDGE_LOOP ( 'NONE', ( #21847, #49076, #115403, #79799 ) ) ;
#56626 = VERTEX_POINT ( 'NONE', #105172 ) ;
#56627 = CARTESIAN_POINT ( 'NONE',  ( -2.499999999999996003, 12.50000000000000000, -2.276824562219559311E-15 ) ) ;
#56628 = CARTESIAN_POINT ( 'NONE',  ( 4.349999999999939249, 2.500000000000000000, 2.611473670974873151 ) ) ;
#56629 = DIRECTION ( 'NONE',  ( 0.000000000000000000, 0.000000000000000000, 1.000000000000000000 ) ) ;
#56630 = ADVANCED_FACE ( 'NONE', ( #66533 ), #12082, .T. ) ;
#56631 = FACE_BOUND ( 'NONE', #24509, .T. ) ;
#56632 = ORIENTED_EDGE ( 'NONE', *, *, #71089, .T. ) ;
#56633 = EDGE_CURVE ( 'NONE', #125704, #11303, #72732, .T. ) ;
#56634 = DIRECTION ( 'NONE',  ( -0.000000000000000000, 1.000000000000000000, -0.000000000000000000 ) ) ;
#56635 = DIRECTION ( 'NONE',  ( 0.000000000000000000, 1.000000000000000000, 0.000000000000000000 ) ) ;
#56636 = CARTESIAN_POINT ( 'NONE',  ( -17.50000000000000000, 2.500000000000000000, 1.734723475976807094E-15 ) ) ;
#56637 = EDGE_CURVE ( 'NONE', #66216, #25385, #124828, .T. ) ;
#56638 = CARTESIAN_POINT ( 'NONE',  ( 129.5000000000000000, -1.500000000000000000, -2.598076211353316900 ) ) ;
#56639 = ADVANCED_FACE ( 'NONE', ( #75078 ), #44985, .T. ) ;
#56640 = DIRECTION ( 'NONE',  ( 1.000000000000000000, 0.000000000000000000, 0.000000000000000000 ) ) ;
#56641 = ADVANCED_FACE ( 'NONE', ( #123516 ), #30892, .T. ) ;
#56642 = DIRECTION ( 'NONE',  ( -0.000000000000000000, -1.000000000000000000, -0.000000000000000000 ) ) ;
#56643 = DIRECTION ( 'NONE',  ( 0.000000000000000000, 0.000000000000000000, -1.000000000000000000 ) ) ;
#56644 = CONICAL_SURFACE ( 'NONE', #75440, 0.09999999999999982514, 0.003490658503988666988 ) ;
#56645 = CIRCLE ( 'NONE', #119358, 0.06509327318403745899 ) ;
#56646 = EDGE_CURVE ( 'NONE', #111056, #49367, #37142, .T. ) ;
#56647 = ORIENTED_EDGE ( 'NONE', *, *, #91402, .F. ) ;
#56648 = VERTEX_POINT ( 'NONE', #95367 ) ;
#56649 = ORIENTED_EDGE ( 'NONE', *, *, #25808, .T. ) ;
#56650 = EDGE_LOOP ( 'NONE', ( #111093, #63795, #17089, #26949 ) ) ;
#56651 = ORIENTED_EDGE ( 'NONE', *, *, #76601, .T. ) ;
#56652 = CARTESIAN_POINT ( 'NONE',  ( 6.649999999999931966, 2.500000000000000000, -7.188010851410854052 ) ) ;
#56653 = DIRECTION ( 'NONE',  ( 0.000000000000000000, -0.9999939076577903929, 0.003490651415223739937 ) ) ;
#56654 = VERTEX_POINT ( 'NONE', #56064 ) ;
#56655 = FACE_BOUND ( 'NONE', #126432, .T. ) ;
#56657 = ADVANCED_FACE ( 'NONE', ( #5670 ), #54778, .T. ) ;
#56656 = AXIS2_PLACEMENT_3D ( 'NONE', #40831, #62391, #120013 ) ;
#56658 = DIRECTION ( 'NONE',  ( 0.000000000000000000, 0.000000000000000000, 1.000000000000000000 ) ) ;
#56659 = AXIS2_PLACEMENT_3D ( 'NONE', #38742, #78655, #118553 ) ;
#56660 = CARTESIAN_POINT ( 'NONE',  ( -8.350000000000013856, 2.500000000000000000, -7.288010851410849256 ) ) ;
#56661 = CARTESIAN_POINT ( 'NONE',  ( 5.849999999999934808, 2.500000000000000000, -5.702370205355749455 ) ) ;
#56662 = CARTESIAN_POINT ( 'NONE',  ( 186.7916666666667140, 4.445597072760099522, -7.700000000000035705 ) ) ;
#56663 = CARTESIAN_POINT ( 'NONE',  ( -1.850000000000033840, 2.500000000000000000, 6.148780366869520897 ) ) ;
#56664 = ORIENTED_EDGE ( 'NONE', *, *, #42449, .T. ) ;
#56665 = CARTESIAN_POINT ( 'NONE',  ( 6.899999999999926636, 12.50000000000000000, 0.2813168883297362810 ) ) ;
#56666 = AXIS2_PLACEMENT_3D ( 'NONE', #56133, #96696, #7021 ) ;
#56667 = VERTEX_POINT ( 'NONE', #113715 ) ;
#56668 = VECTOR ( 'NONE', #51999, 1000.000000000000000 ) ;
#56669 = EDGE_LOOP ( 'NONE', ( #14685, #101328, #123565, #22193 ) ) ;
#56670 = ORIENTED_EDGE ( 'NONE', *, *, #115489, .T. ) ;
#56671 = DIRECTION ( 'NONE',  ( 0.000000000000000000, 1.000000000000000000, 0.000000000000000000 ) ) ;
#56672 = LINE ( 'NONE', #64576, #124991 ) ;
#56673 = CARTESIAN_POINT ( 'NONE',  ( -7.950000000000012612, 2.500000000000000000, -2.265063509461101798 ) ) ;
#56674 = VERTEX_POINT ( 'NONE', #44318 ) ;
#56675 = FACE_OUTER_BOUND ( 'NONE', #81384, .T. ) ;
#56676 = CONICAL_SURFACE ( 'NONE', #4529, 0.1000000000000002554, 0.003490658503988666988 ) ;
#56677 = DIRECTION ( 'NONE',  ( 0.000000000000000000, 0.000000000000000000, -1.000000000000000000 ) ) ;
#56678 = CARTESIAN_POINT ( 'NONE',  ( 4.599999999999936584, 12.50000000000000000, 4.395220292106234439 ) ) ;
#56679 = AXIS2_PLACEMENT_3D ( 'NONE', #103272, #55451, #43723 ) ;
#56680 = CARTESIAN_POINT ( 'NONE',  ( 184.4895833340161460, -4.445597072760115509, -7.700000000000001954 ) ) ;
#56681 = CARTESIAN_POINT ( 'NONE',  ( 0.6499999999999561684, 2.500000000000000000, -1.818653347947325916 ) ) ;
#56682 = DIRECTION ( 'NONE',  ( 0.000000000000000000, -0.000000000000000000, 1.000000000000000000 ) ) ;
#56683 = LINE ( 'NONE', #117533, #9875 ) ;
#56684 = ORIENTED_EDGE ( 'NONE', *, *, #12323, .F. ) ;
#56685 = CARTESIAN_POINT ( 'NONE',  ( -8.100000000000013856, 2.500000000000000000, -4.576537180435977348 ) ) ;
#56686 = ORIENTED_EDGE ( 'NONE', *, *, #8550, .F. ) ;
#56687 = EDGE_CURVE ( 'NONE', #43527, #7618, #53862, .T. ) ;
#56688 = VERTEX_POINT ( 'NONE', #84237 ) ;
#56689 = FACE_OUTER_BOUND ( 'NONE', #111457, .T. ) ;
#56690 = FACE_OUTER_BOUND ( 'NONE', #44617, .T. ) ;
#56691 = LINE ( 'NONE', #65886, #98962 ) ;
#56692 = VERTEX_POINT ( 'NONE', #124174 ) ;
#56693 = ORIENTED_EDGE ( 'NONE', *, *, #14144, .F. ) ;
#56694 = ADVANCED_FACE ( 'NONE', ( #34529 ), #74438, .T. ) ;
#56695 = CARTESIAN_POINT ( 'NONE',  ( 10.39999999999991331, 2.500000000000000000, 0.09999999999999761857 ) ) ;
#56696 = CARTESIAN_POINT ( 'NONE',  ( 1.899999999999951283, 12.50000000000000000, -0.4115034346978156399 ) ) ;
#56698 = LINE ( 'NONE', #94076, #39848 ) ;
#56697 = AXIS2_PLACEMENT_3D ( 'NONE', #104698, #46429, #15013 ) ;
#56699 = EDGE_LOOP ( 'NONE', ( #81394, #113782 ) ) ;
#56700 = EDGE_LOOP ( 'NONE', ( #36895, #51802 ) ) ;
#56701 = AXIS2_PLACEMENT_3D ( 'NONE', #63363, #123551, #73814 ) ;
#56702 = CARTESIAN_POINT ( 'NONE',  ( 3.349999999999943689, 12.50000000000000000, 1.537336459617582918 ) ) ;
#56703 = VERTEX_POINT ( 'NONE', #35171 ) ;
#56704 = LINE ( 'NONE', #5040, #79222 ) ;
#56705 = AXIS2_PLACEMENT_3D ( 'NONE', #96214, #46474, #76592 ) ;
#56706 = DIRECTION ( 'NONE',  ( 0.000000000000000000, 1.000000000000000000, 0.000000000000000000 ) ) ;
#56707 = ORIENTED_EDGE ( 'NONE', *, *, #105380, .T. ) ;
#56708 = CARTESIAN_POINT ( 'NONE',  ( -7.900000000000014566, 2.500000000000000000, -0.6928203230275541413 ) ) ;
#56709 = DIRECTION ( 'NONE',  ( 0.000000000000000000, -0.000000000000000000, 1.000000000000000000 ) ) ;
#56710 = DIRECTION ( 'NONE',  ( 0.000000000000000000, 1.000000000000000000, 0.000000000000000000 ) ) ;
#56711 = CIRCLE ( 'NONE', #121471, 0.06509327318403745899 ) ;
#56712 = DIRECTION ( 'NONE',  ( 0.000000000000000000, 1.000000000000000000, 0.000000000000000000 ) ) ;
#56713 = EDGE_LOOP ( 'NONE', ( #77258, #103193, #40739, #120513 ) ) ;
#56714 = LINE ( 'NONE', #96645, #61354 ) ;
#56715 = FACE_OUTER_BOUND ( 'NONE', #122413, .T. ) ;
#56716 = VERTEX_POINT ( 'NONE', #68467 ) ;
#56717 = ORIENTED_EDGE ( 'NONE', *, *, #7040, .T. ) ;
#56718 = CARTESIAN_POINT ( 'NONE',  ( 184.9218750003414016, 0.000000000000000000, 7.564683531250000925 ) ) ;
#56719 = CARTESIAN_POINT ( 'NONE',  ( 9.349999999999919709, 12.50000000000000000, 1.818653347947321475 ) ) ;
#56720 = FACE_OUTER_BOUND ( 'NONE', #89989, .T. ) ;
#56721 = DIRECTION ( 'NONE',  ( -0.000000000000000000, -1.000000000000000000, -0.000000000000000000 ) ) ;
#56722 = DIRECTION ( 'NONE',  ( 0.000000000000000000, -0.000000000000000000, 1.000000000000000000 ) ) ;
#56723 = DIRECTION ( 'NONE',  ( -0.000000000000000000, -1.000000000000000000, -0.000000000000000000 ) ) ;
#56724 = EDGE_CURVE ( 'NONE', #49230, #114968, #118695, .T. ) ;
#56725 = DIRECTION ( 'NONE',  ( 0.000000000000000000, 1.000000000000000000, 0.000000000000000000 ) ) ;
#56726 = FACE_OUTER_BOUND ( 'NONE', #42472, .T. ) ;
#56727 = CARTESIAN_POINT ( 'NONE',  ( -9.550000000000006040, 2.500000000000000000, -2.065063509461102065 ) ) ;
#56728 = DIRECTION ( 'NONE',  ( 0.000000000000000000, 0.000000000000000000, 1.000000000000000000 ) ) ;
#56729 = CONICAL_SURFACE ( 'NONE', #94404, 0.09999999999999982514, 0.003490658503988666988 ) ;
#56730 = EDGE_CURVE ( 'NONE', #125196, #58516, #127027, .T. ) ;
#56731 = EDGE_LOOP ( 'NONE', ( #49561, #99073, #124685, #34815 ) ) ;
#56732 = CONICAL_SURFACE ( 'NONE', #35839, 0.09999999999999982514, 0.003490658503988666988 ) ;
#56733 = EDGE_LOOP ( 'NONE', ( #102897, #74228, #125797, #105288 ) ) ;
#56734 = CARTESIAN_POINT ( 'NONE',  ( 1.049999999999952971, 2.500000000000000000, 6.248780366869521430 ) ) ;
#56735 = EDGE_CURVE ( 'NONE', #79023, #118813, #104032, .T. ) ;
#56736 = ORIENTED_EDGE ( 'NONE', *, *, #92554, .T. ) ;
#56737 = CARTESIAN_POINT ( 'NONE',  ( 8.549999999999918998, 2.500000000000000000, 6.841600689897072485 ) ) ;
#56738 = ADVANCED_FACE ( 'NONE', ( #39051 ), #81059, .T. ) ;
#56739 = DIRECTION ( 'NONE',  ( 0.000000000000000000, 0.000000000000000000, 1.000000000000000000 ) ) ;
#56740 = DIRECTION ( 'NONE',  ( -1.000000000000000000, -0.000000000000000000, -0.000000000000000000 ) ) ;
#56741 = AXIS2_PLACEMENT_3D ( 'NONE', #108588, #118401, #57563 ) ;
#56742 = VERTEX_POINT ( 'NONE', #59331 ) ;
#56743 = DIRECTION ( 'NONE',  ( -4.274815082592931898E-19, -0.9999939076577903929, -0.003490651415223739937 ) ) ;
#56744 = AXIS2_PLACEMENT_3D ( 'NONE', #11528, #12160, #100552 ) ;
#56745 = EDGE_CURVE ( 'NONE', #109816, #26449, #33041, .T. ) ;
#56746 = DIRECTION ( 'NONE',  ( -0.000000000000000000, -1.000000000000000000, -0.000000000000000000 ) ) ;
#56748 = VERTEX_POINT ( 'NONE', #78317 ) ;
#56747 = DIRECTION ( 'NONE',  ( 0.000000000000000000, 0.000000000000000000, 1.000000000000000000 ) ) ;
#56749 = EDGE_CURVE ( 'NONE', #116833, #49349, #49505, .T. ) ;
#56750 = DIRECTION ( 'NONE',  ( 0.000000000000000000, 0.000000000000000000, -1.000000000000000000 ) ) ;
#56751 = CIRCLE ( 'NONE', #17025, 0.06509327318403745899 ) ;
#56752 = ORIENTED_EDGE ( 'NONE', *, *, #112971, .T. ) ;
#56753 = AXIS2_PLACEMENT_3D ( 'NONE', #4800, #45402, #44755 ) ;
#56754 = EDGE_LOOP ( 'NONE', ( #53971, #116149 ) ) ;
#56755 = VERTEX_POINT ( 'NONE', #18730 ) ;
#56757 = ORIENTED_EDGE ( 'NONE', *, *, #84103, .T. ) ;
#56756 = CIRCLE ( 'NONE', #48383, 0.1000000000000002554 ) ;
#56758 = DIRECTION ( 'NONE',  ( 0.000000000000000000, -0.000000000000000000, 1.000000000000000000 ) ) ;
#56759 = CIRCLE ( 'NONE', #35865, 0.06509327318403743123 ) ;
#56760 = CARTESIAN_POINT ( 'NONE',  ( 21.34481565588170682, 0.7053969147713127219, 2.184679923000720336 ) ) ;
#56761 = DIRECTION ( 'NONE',  ( -0.000000000000000000, -1.000000000000000000, -0.000000000000000000 ) ) ;
#56762 = LINE ( 'NONE', #96697, #64502 ) ;
#56763 = ORIENTED_EDGE ( 'NONE', *, *, #12195, .T. ) ;
#56764 = EDGE_CURVE ( 'NONE', #97882, #101949, #41356, .T. ) ;
#56765 = AXIS2_PLACEMENT_3D ( 'NONE', #9347, #47995, #49295 ) ;
#56766 = AXIS2_PLACEMENT_3D ( 'NONE', #2306, #42263, #74938 ) ;
#56767 = FACE_OUTER_BOUND ( 'NONE', #40160, .T. ) ;
#56768 = ORIENTED_EDGE ( 'NONE', *, *, #21666, .T. ) ;
#56769 = CARTESIAN_POINT ( 'NONE',  ( -3.550000000000030909, 2.500000000000000000, -6.941600689897078347 ) ) ;
#56770 = DIRECTION ( 'NONE',  ( -4.274815082592931898E-19, -0.9999939076577903929, -0.003490651415223739937 ) ) ;
#56771 = DIRECTION ( 'NONE',  ( 0.000000000000000000, 0.000000000000000000, 1.000000000000000000 ) ) ;
#56772 = DIRECTION ( 'NONE',  ( 0.000000000000000000, -0.000000000000000000, 1.000000000000000000 ) ) ;
#56773 = ORIENTED_EDGE ( 'NONE', *, *, #53163, .F. ) ;
#56774 = EDGE_CURVE ( 'NONE', #111073, #27457, #49767, .T. ) ;
#56775 = ORIENTED_EDGE ( 'NONE', *, *, #22584, .F. ) ;
#56776 = ORIENTED_EDGE ( 'NONE', *, *, #83692, .T. ) ;
#56777 = ORIENTED_EDGE ( 'NONE', *, *, #76762, .T. ) ;
#56778 = FACE_OUTER_BOUND ( 'NONE', #87081, .T. ) ;
#56779 = CARTESIAN_POINT ( 'NONE',  ( -11.64999999999999680, 12.50000000000000000, 7.253104124594885960 ) ) ;
#56780 = DIRECTION ( 'NONE',  ( 0.000000000000000000, 0.000000000000000000, 1.000000000000000000 ) ) ;
#56781 = FACE_BOUND ( 'NONE', #51010, .T. ) ;
#56782 = DIRECTION ( 'NONE',  ( 0.000000000000000000, 0.000000000000000000, 1.000000000000000000 ) ) ;
#56783 = CARTESIAN_POINT ( 'NONE',  ( -7.100000000000013856, 12.50000000000000000, 5.088040615133786027 ) ) ;
#56784 = ADVANCED_FACE ( 'NONE', ( #39694 ), #112454, .T. ) ;
#56785 = DIRECTION ( 'NONE',  ( 0.000000000000000000, 0.000000000000000000, 1.000000000000000000 ) ) ;
#56786 = DIRECTION ( 'NONE',  ( 0.000000000000000000, -0.9999939076577903929, 0.003490651415223739937 ) ) ;
#56787 = VECTOR ( 'NONE', #58273, 1000.000000000000000 ) ;
#56788 = AXIS2_PLACEMENT_3D ( 'NONE', #99916, #110368, #18114 ) ;
#56789 = EDGE_CURVE ( 'NONE', #106091, #110912, #6946, .T. ) ;
#56791 = CIRCLE ( 'NONE', #106976, 0.06509327318403745899 ) ;
#56790 = CARTESIAN_POINT ( 'NONE',  ( 184.7968750003414584, 8.734944146203032389, 5.348610694689227483E-16 ) ) ;
#56792 = CARTESIAN_POINT ( 'NONE',  ( 195.0000000000000000, 0.000000000000000000, -4.000000000000000000 ) ) ;
#56793 = EDGE_CURVE ( 'NONE', #8279, #120770, #72740, .T. ) ;
#56794 = DIRECTION ( 'NONE',  ( 0.000000000000000000, 0.000000000000000000, 1.000000000000000000 ) ) ;
#56795 = EDGE_CURVE ( 'NONE', #121408, #104331, #35091, .T. ) ;
#56796 = DIRECTION ( 'NONE',  ( 0.000000000000000000, -0.9999939076577903929, 0.003490651415223739937 ) ) ;
#56797 = CONICAL_SURFACE ( 'NONE', #372, 0.09999999999999982514, 0.003490658503988666988 ) ;
#56798 = EDGE_CURVE ( 'NONE', #111188, #93106, #74793, .T. ) ;
#56799 = ORIENTED_EDGE ( 'NONE', *, *, #24608, .T. ) ;
#56800 = ORIENTED_EDGE ( 'NONE', *, *, #36268, .T. ) ;
#56801 = ORIENTED_EDGE ( 'NONE', *, *, #24924, .T. ) ;
#56802 = ORIENTED_EDGE ( 'NONE', *, *, #77026, .T. ) ;
#56803 = AXIS2_PLACEMENT_3D ( 'NONE', #69083, #38363, #109001 ) ;
#56804 = CIRCLE ( 'NONE', #65222, 0.1000000000000000472 ) ;
#56805 = DIRECTION ( 'NONE',  ( 0.000000000000000000, 0.000000000000000000, 1.000000000000000000 ) ) ;
#56806 = FACE_BOUND ( 'NONE', #54568, .T. ) ;
#56807 = DIRECTION ( 'NONE',  ( -0.000000000000000000, 1.000000000000000000, -0.000000000000000000 ) ) ;
#56808 = EDGE_CURVE ( 'NONE', #43342, #42494, #91511, .T. ) ;
#56809 = CIRCLE ( 'NONE', #113265, 0.09999999999999982514 ) ;
#56810 = DIRECTION ( 'NONE',  ( 0.000000000000000000, 0.000000000000000000, 1.000000000000000000 ) ) ;
#56811 = EDGE_CURVE ( 'NONE', #124471, #40728, #51812, .T. ) ;
#56812 = VERTEX_POINT ( 'NONE', #67152 ) ;
#56813 = DIRECTION ( 'NONE',  ( 0.000000000000000000, 0.000000000000000000, 1.000000000000000000 ) ) ;
#56814 = FACE_BOUND ( 'NONE', #1131, .T. ) ;
#56815 = EDGE_LOOP ( 'NONE', ( #88509, #52403 ) ) ;
#56816 = DIRECTION ( 'NONE',  ( -0.000000000000000000, 1.000000000000000000, -0.000000000000000000 ) ) ;
#56817 = CARTESIAN_POINT ( 'NONE',  ( -9.150000000000009237, 2.500000000000000000, 2.957883832488649389 ) ) ;
#56818 = ORIENTED_EDGE ( 'NONE', *, *, #48529, .F. ) ;
#56819 = CARTESIAN_POINT ( 'NONE',  ( 6.049999999999934097, 12.50000000000000000, -6.148780366869526226 ) ) ;
#56820 = LINE ( 'NONE', #105949, #126952 ) ;
#56821 = CIRCLE ( 'NONE', #10853, 0.1000000000000000472 ) ;
#56822 = AXIS2_PLACEMENT_3D ( 'NONE', #13267, #81395, #112781 ) ;
#56823 = ORIENTED_EDGE ( 'NONE', *, *, #99245, .F. ) ;
#56824 = CARTESIAN_POINT ( 'NONE',  ( 3.549999999999942979, 2.500000000000000000, 1.718653347947321386 ) ) ;
#56825 = DIRECTION ( 'NONE',  ( 0.000000000000000000, -0.000000000000000000, 1.000000000000000000 ) ) ;
#56826 = VERTEX_POINT ( 'NONE', #47560 ) ;
#56827 = DIRECTION ( 'NONE',  ( 0.000000000000000000, -0.000000000000000000, 1.000000000000000000 ) ) ;
#56828 = ORIENTED_EDGE ( 'NONE', *, *, #84726, .F. ) ;
#56829 = EDGE_LOOP ( 'NONE', ( #60184, #37566 ) ) ;
#56830 = DIRECTION ( 'NONE',  ( 0.000000000000000000, 0.000000000000000000, -1.000000000000000000 ) ) ;
#56831 = CIRCLE ( 'NONE', #4592, 0.1000000000000002554 ) ;
#56832 = VERTEX_POINT ( 'NONE', #107097 ) ;
#56833 = DIRECTION ( 'NONE',  ( -4.274815082592931898E-19, -0.9999939076577903929, -0.003490651415223739937 ) ) ;
#56834 = AXIS2_PLACEMENT_3D ( 'NONE', #11489, #111627, #121433 ) ;
#56835 = FACE_OUTER_BOUND ( 'NONE', #25297, .T. ) ;
#56836 = AXIS2_PLACEMENT_3D ( 'NONE', #70766, #18443, #49856 ) ;
#56837 = EDGE_LOOP ( 'NONE', ( #116120, #87022, #104497, #86046 ) ) ;
#56838 = CONICAL_SURFACE ( 'NONE', #81999, 0.1000000000000002554, 0.003490658503988666988 ) ;
#56839 = EDGE_CURVE ( 'NONE', #72411, #82981, #22579, .T. ) ;
#56840 = CARTESIAN_POINT ( 'NONE',  ( 1.849999999999949019, 12.50000000000000000, 6.841600689897072485 ) ) ;
#56841 = VERTEX_POINT ( 'NONE', #18078 ) ;
#56842 = CARTESIAN_POINT ( 'NONE',  ( -3.350000000000028955, 12.50000000000000000, 5.802370205355744659 ) ) ;
#56843 = CARTESIAN_POINT ( 'NONE',  ( 3.549999999999943867, 2.500000000000000000, -1.818653347947326138 ) ) ;
#56844 = DIRECTION ( 'NONE',  ( -0.000000000000000000, -1.000000000000000000, -0.000000000000000000 ) ) ;
#56845 = CARTESIAN_POINT ( 'NONE',  ( -9.999999999999971578, 12.50000000000000000, -4.330127018922197202 ) ) ;
#56846 = DIRECTION ( 'NONE',  ( 0.000000000000000000, 1.000000000000000000, 0.000000000000000000 ) ) ;
#56847 = ORIENTED_EDGE ( 'NONE', *, *, #117105, .F. ) ;
#56848 = AXIS2_PLACEMENT_3D ( 'NONE', #73396, #94319, #113324 ) ;
#56849 = EDGE_CURVE ( 'NONE', #64010, #100714, #97933, .T. ) ;
#56850 = ORIENTED_EDGE ( 'NONE', *, *, #24840, .F. ) ;
#56851 = DIRECTION ( 'NONE',  ( 0.000000000000000000, 0.000000000000000000, 1.000000000000000000 ) ) ;
#56853 = AXIS2_PLACEMENT_3D ( 'NONE', #120580, #100924, #90456 ) ;
#56852 = CARTESIAN_POINT ( 'NONE',  ( -8.950000000000004619, 2.500000000000000000, 6.148780366869520897 ) ) ;
#56854 = VECTOR ( 'NONE', #83311, 1000.000000000000000 ) ;
#56855 = CIRCLE ( 'NONE', #67308, 0.06509327318403745899 ) ;
#56856 = DIRECTION ( 'NONE',  ( 0.000000000000000000, 0.000000000000000000, 1.000000000000000000 ) ) ;
#56858 = ORIENTED_EDGE ( 'NONE', *, *, #53226, .T. ) ;
#56857 = ORIENTED_EDGE ( 'NONE', *, *, #100470, .F. ) ;
#56859 = ORIENTED_EDGE ( 'NONE', *, *, #18128, .T. ) ;
#56860 = LINE ( 'NONE', #126923, #25016 ) ;
#56861 = CONICAL_SURFACE ( 'NONE', #98729, 0.1000000000000002554, 0.003490658503988666988 ) ;
#56862 = DIRECTION ( 'NONE',  ( 1.000000000000000000, 0.000000000000000000, 0.000000000000000000 ) ) ;
#56863 = CARTESIAN_POINT ( 'NONE',  ( 2.499999999999981792, 12.50000000000000000, 4.330127018922196314 ) ) ;
#56864 = PRODUCT_CONTEXT ( 'NONE', #17924, 'mechanical' ) ;
#56865 = CARTESIAN_POINT ( 'NONE',  ( -5.650000000000023448, 2.500000000000000000, -6.841600689897078702 ) ) ;
#56866 = AXIS2_PLACEMENT_3D ( 'NONE', #17707, #49138, #57654 ) ;
#56867 = DIRECTION ( 'NONE',  ( 0.000000000000000000, 1.000000000000000000, 0.000000000000000000 ) ) ;
#56868 = CARTESIAN_POINT ( 'NONE',  ( 0.8499999999999553468, 2.500000000000000000, -2.165063509461101710 ) ) ;
#56869 = LINE ( 'NONE', #47089, #26243 ) ;
#56870 = DIRECTION ( 'NONE',  ( 0.000000000000000000, 0.000000000000000000, 1.000000000000000000 ) ) ;
#56871 = CARTESIAN_POINT ( 'NONE',  ( 10.84999999999991260, 2.500000000000000000, -1.372243186433550033 ) ) ;
#56872 = ORIENTED_EDGE ( 'NONE', *, *, #1544, .F. ) ;
#56873 = FACE_OUTER_BOUND ( 'NONE', #29838, .T. ) ;
#56874 = ORIENTED_EDGE ( 'NONE', *, *, #104266, .F. ) ;
#56875 = EDGE_LOOP ( 'NONE', ( #116791, #33058, #74168, #33454 ) ) ;
#56876 = DIRECTION ( 'NONE',  ( 0.000000000000000000, 0.000000000000000000, 1.000000000000000000 ) ) ;
#56877 = DIRECTION ( 'NONE',  ( 0.000000000000000000, -0.9999939076577903929, 0.003490651415223739937 ) ) ;
#56878 = DIRECTION ( 'NONE',  ( 0.000000000000000000, 0.000000000000000000, -1.000000000000000000 ) ) ;
#56879 = LINE ( 'NONE', #4547, #94415 ) ;
#56880 = CARTESIAN_POINT ( 'NONE',  ( -8.100000000000010303, 12.50000000000000000, 3.918623584224383727 ) ) ;
#56881 = CARTESIAN_POINT ( 'NONE',  ( -10.45000000000000462, 12.50000000000000000, -6.495190528383298911 ) ) ;
#56882 = AXIS2_PLACEMENT_3D ( 'NONE', #112370, #43641, #123456 ) ;
#56883 = CARTESIAN_POINT ( 'NONE',  ( -8.750000000000010658, 2.500000000000000000, -1.472243186433550122 ) ) ;
#56884 = ORIENTED_EDGE ( 'NONE', *, *, #13971, .F. ) ;
#56885 = CARTESIAN_POINT ( 'NONE',  ( 8.549999999999924327, 12.50000000000000000, -6.841600689897077814 ) ) ;
#56886 = VECTOR ( 'NONE', #114, 1000.000000000000000 ) ;
#56887 = AXIS2_PLACEMENT_3D ( 'NONE', #11822, #72055, #111294 ) ;
#56888 = DIRECTION ( 'NONE',  ( 0.000000000000000000, 0.000000000000000000, 1.000000000000000000 ) ) ;
#56889 = ORIENTED_EDGE ( 'NONE', *, *, #112739, .T. ) ;
#56890 = EDGE_CURVE ( 'NONE', #33973, #110810, #123755, .T. ) ;
#56891 = ORIENTED_EDGE ( 'NONE', *, *, #33906, .T. ) ;
#56892 = CONICAL_SURFACE ( 'NONE', #10911, 0.1000000000000002554, 0.003490658503988666988 ) ;
#56893 = VERTEX_POINT ( 'NONE', #112282 ) ;
#56894 = CONICAL_SURFACE ( 'NONE', #65221, 0.1000000000000002554, 0.003490658503988666988 ) ;
#56895 = EDGE_CURVE ( 'NONE', #42690, #6759, #125801, .T. ) ;
#56896 = AXIS2_PLACEMENT_3D ( 'NONE', #30674, #68635, #40495 ) ;
#56897 = EDGE_CURVE ( 'NONE', #13178, #22580, #109066, .T. ) ;
#56898 = VERTEX_POINT ( 'NONE', #21975 ) ;
#56899 = EDGE_LOOP ( 'NONE', ( #62118, #96849 ) ) ;
#56900 = EDGE_CURVE ( 'NONE', #29791, #76636, #81525, .T. ) ;
#56901 = DIRECTION ( 'NONE',  ( -4.274815082592931898E-19, -0.9999939076577903929, -0.003490651415223739937 ) ) ;
#56902 = CARTESIAN_POINT ( 'NONE',  ( 11.84999999999990727, 2.500000000000000000, 6.148780366869520009 ) ) ;
#56903 = CONICAL_SURFACE ( 'NONE', #111283, 0.1000000000000000056, 0.003490658503988666988 ) ;
#56904 = EDGE_LOOP ( 'NONE', ( #36985, #98686 ) ) ;
#56905 = CARTESIAN_POINT ( 'NONE',  ( -13.29999999999999005, 12.50000000000000000, -4.330127018922198978 ) ) ;
#56906 = DIRECTION ( 'NONE',  ( 0.000000000000000000, 0.000000000000000000, -1.000000000000000000 ) ) ;
#56907 = ADVANCED_FACE ( 'NONE', ( #31152 ), #90695, .T. ) ;
#56908 = CARTESIAN_POINT ( 'NONE',  ( 3.949999999999938893, 2.500000000000000000, 6.048780366869520364 ) ) ;
#56910 = ORIENTED_EDGE ( 'NONE', *, *, #84789, .F. ) ;
#56909 = ADVANCED_FACE ( 'NONE', ( #1022 ), #2964, .T. ) ;
#56911 = ADVANCED_FACE ( 'NONE', ( #30513 ), #110958, .T. ) ;
#56912 = FACE_OUTER_BOUND ( 'NONE', #13779, .T. ) ;
#56913 = DIRECTION ( 'NONE',  ( -0.000000000000000000, -1.000000000000000000, -0.000000000000000000 ) ) ;
#56914 = EDGE_LOOP ( 'NONE', ( #100087, #96302 ) ) ;
#56915 = ORIENTED_EDGE ( 'NONE', *, *, #121216, .T. ) ;
#56916 = ORIENTED_EDGE ( 'NONE', *, *, #43954, .F. ) ;
#56917 = LINE ( 'NONE', #128937, #50952 ) ;
#56918 = AXIS2_PLACEMENT_3D ( 'NONE', #63211, #103136, #122781 ) ;
#56919 = CARTESIAN_POINT ( 'NONE',  ( 11.69999999999990870, 2.500000000000000000, -4.330127018922201643 ) ) ;
#56920 = CONICAL_SURFACE ( 'NONE', #65544, 0.1000000000000002554, 0.003490658503988666988 ) ;
#56921 = ORIENTED_EDGE ( 'NONE', *, *, #73083, .T. ) ;
#56922 = CARTESIAN_POINT ( 'NONE',  ( 8.299999999999922551, 12.50000000000000000, 4.265033745738159077 ) ) ;
#56923 = DIRECTION ( 'NONE',  ( 0.000000000000000000, 0.000000000000000000, 1.000000000000000000 ) ) ;
#56924 = DIRECTION ( 'NONE',  ( -0.000000000000000000, -1.000000000000000000, -0.000000000000000000 ) ) ;
#56925 = CARTESIAN_POINT ( 'NONE',  ( -13.34999999999999076, 2.500000000000000000, -2.165063509461099489 ) ) ;
#56926 = CIRCLE ( 'NONE', #44432, 0.06509327318403745899 ) ;
#56927 = STYLED_ITEM ( 'NONE', ( #60465 ), #57280 ) ;
#56928 = AXIS2_PLACEMENT_3D ( 'NONE', #62347, #104812, #123814 ) ;
#56929 = ORIENTED_EDGE ( 'NONE', *, *, #82081, .F. ) ;
#56930 = DIRECTION ( 'NONE',  ( -0.000000000000000000, 1.000000000000000000, -0.000000000000000000 ) ) ;
#56931 = CIRCLE ( 'NONE', #73670, 0.06509327318403741736 ) ;
#56932 = VERTEX_POINT ( 'NONE', #101812 ) ;
#56933 = ORIENTED_EDGE ( 'NONE', *, *, #81243, .T. ) ;
#56934 = ORIENTED_EDGE ( 'NONE', *, *, #35540, .T. ) ;
#56935 = CARTESIAN_POINT ( 'NONE',  ( 115.5000000000000000, 5.000000000000000000, -1.999999999999997335 ) ) ;
#56936 = FACE_BOUND ( 'NONE', #76034, .T. ) ;
#56937 = LINE ( 'NONE', #65486, #40905 ) ;
#56939 = PLANE ( 'NONE',  #92469 ) ;
#56938 = AXIS2_PLACEMENT_3D ( 'NONE', #113152, #92214, #13653 ) ;
#56941 = DIRECTION ( 'NONE',  ( 0.000000000000000000, 0.000000000000000000, -1.000000000000000000 ) ) ;
#56940 = VECTOR ( 'NONE', #96905, 1000.000000000000000 ) ;
#56942 = VECTOR ( 'NONE', #57543, 1000.000000000000000 ) ;
#56943 = CIRCLE ( 'NONE', #104977, 5.000000000000000000 ) ;
#56944 = AXIS2_PLACEMENT_3D ( 'NONE', #32097, #111931, #42565 ) ;
#56945 = ADVANCED_FACE ( 'NONE', ( #42248 ), #127962, .T. ) ;
#56946 = ORIENTED_EDGE ( 'NONE', *, *, #25474, .T. ) ;
#56947 = EDGE_CURVE ( 'NONE', #73847, #33436, #104874, .T. ) ;
#56948 = DIRECTION ( 'NONE',  ( 1.000000000000000000, 0.000000000000000000, 0.000000000000000000 ) ) ;
#56949 = FACE_OUTER_BOUND ( 'NONE', #128515, .T. ) ;
#56950 = DIRECTION ( 'NONE',  ( 0.000000000000000000, -0.000000000000000000, 1.000000000000000000 ) ) ;
#56951 = AXIS2_PLACEMENT_3D ( 'NONE', #6405, #57485, #116380 ) ;
#56952 = EDGE_CURVE ( 'NONE', #129059, #2089, #100758, .T. ) ;
#56953 = DIRECTION ( 'NONE',  ( -0.000000000000000000, -1.000000000000000000, -0.000000000000000000 ) ) ;
#56954 = ORIENTED_EDGE ( 'NONE', *, *, #50753, .F. ) ;
#56955 = DIRECTION ( 'NONE',  ( 0.000000000000000000, -0.000000000000000000, 1.000000000000000000 ) ) ;
#56956 = DIRECTION ( 'NONE',  ( 0.000000000000000000, 0.000000000000000000, -1.000000000000000000 ) ) ;
#56957 = CONICAL_SURFACE ( 'NONE', #4627, 0.09999999999999982514, 0.003490658503988666988 ) ;
#56958 = ADVANCED_FACE ( 'NONE', ( #80888 ), #14969, .T. ) ;
#56959 = ADVANCED_FACE ( 'NONE', ( #52072 ), #19188, .T. ) ;
#56960 = EDGE_LOOP ( 'NONE', ( #107975, #120594 ) ) ;
#56961 = DIRECTION ( 'NONE',  ( -0.000000000000000000, 1.000000000000000000, -0.000000000000000000 ) ) ;
#56962 = EDGE_CURVE ( 'NONE', #18946, #50137, #91983, .T. ) ;
#56963 = CARTESIAN_POINT ( 'NONE',  ( -10.20000000000000284, 2.500000000000000000, 3.983716857408420964 ) ) ;
#56964 = FACE_BOUND ( 'NONE', #39954, .T. ) ;
#56965 = DIRECTION ( 'NONE',  ( 0.000000000000000000, 0.000000000000000000, -1.000000000000000000 ) ) ;
#56966 = EDGE_CURVE ( 'NONE', #48345, #101934, #51436, .T. ) ;
#56967 = EDGE_CURVE ( 'NONE', #116425, #41491, #48454, .T. ) ;
#56968 = ORIENTED_EDGE ( 'NONE', *, *, #121219, .F. ) ;
#56969 = FACE_OUTER_BOUND ( 'NONE', #14278, .T. ) ;
#56970 = ORIENTED_EDGE ( 'NONE', *, *, #72212, .F. ) ;
#56971 = ORIENTED_EDGE ( 'NONE', *, *, #87871, .F. ) ;
#56973 = VECTOR ( 'NONE', #87814, 1000.000000000000000 ) ;
#56972 = CARTESIAN_POINT ( 'NONE',  ( 17.19804440726973382, 0.4677972980984265172, -5.492654682185373893 ) ) ;
#56974 = CARTESIAN_POINT ( 'NONE',  ( 187.4583333333333428, 4.445597072760117285, 7.699999999999999289 ) ) ;
#56975 = ADVANCED_FACE ( 'NONE', ( #71699 ), #358, .T. ) ;
#56976 = ORIENTED_EDGE ( 'NONE', *, *, #109463, .F. ) ;
#56977 = CARTESIAN_POINT ( 'NONE',  ( 185.8802083336747444, 4.367472073101515306, 7.564683531250000925 ) ) ;
#56978 = DIRECTION ( 'NONE',  ( 0.000000000000000000, 0.000000000000000000, 1.000000000000000000 ) ) ;
#56979 = CIRCLE ( 'NONE', #15104, 0.06509327318403745899 ) ;
#56980 = DIRECTION ( 'NONE',  ( 0.000000000000000000, 1.000000000000000000, 0.000000000000000000 ) ) ;
#56981 = CIRCLE ( 'NONE', #69505, 0.1000000000000000472 ) ;
#56982 = CIRCLE ( 'NONE', #27749, 0.06509327318403745899 ) ;
#56983 = DIRECTION ( 'NONE',  ( 0.000000000000000000, 0.000000000000000000, 1.000000000000000000 ) ) ;
#56984 = AXIS2_PLACEMENT_3D ( 'NONE', #45167, #63515, #15015 ) ;
#56986 = VERTEX_POINT ( 'NONE', #53357 ) ;
#56985 = CIRCLE ( 'NONE', #82041, 0.1000000000000002554 ) ;
#56987 = CIRCLE ( 'NONE', #123899, 0.1000000000000002554 ) ;
#56988 = DIRECTION ( 'NONE',  ( 0.000000000000000000, 0.000000000000000000, 1.000000000000000000 ) ) ;
#56989 = DIRECTION ( 'NONE',  ( 0.000000000000000000, 0.000000000000000000, 1.000000000000000000 ) ) ;
#56990 = DIRECTION ( 'NONE',  ( 0.000000000000000000, 0.000000000000000000, 1.000000000000000000 ) ) ;
#56991 = VECTOR ( 'NONE', #69253, 1000.000000000000000 ) ;
#56992 = CARTESIAN_POINT ( 'NONE',  ( 12.89999999999990266, 12.50000000000000000, -3.637306695894650055 ) ) ;
#56994 = VERTEX_POINT ( 'NONE', #105008 ) ;
#56993 = CIRCLE ( 'NONE', #23567, 0.06509327318403745899 ) ;
#56996 = VECTOR ( 'NONE', #119997, 1000.000000000000000 ) ;
#56995 = CARTESIAN_POINT ( 'NONE',  ( 8.549999999999922551, 12.50000000000000000, 2.511473670974873507 ) ) ;
#56997 = VERTEX_POINT ( 'NONE', #46106 ) ;
#56998 = PLANE ( 'NONE',  #3305 ) ;
#56999 = CARTESIAN_POINT ( 'NONE',  ( -5.850000000000021849, 2.500000000000000000, -2.757883832488654097 ) ) ;
#57000 = AXIS2_PLACEMENT_3D ( 'NONE', #62574, #121460, #93311 ) ;
#57001 = EDGE_LOOP ( 'NONE', ( #12076, #34516 ) ) ;
#57002 = FACE_OUTER_BOUND ( 'NONE', #109895, .T. ) ;
#57003 = DIRECTION ( 'NONE',  ( 0.000000000000000000, -0.9999939076577903929, 0.003490651415223739937 ) ) ;
#57004 = CARTESIAN_POINT ( 'NONE',  ( -11.25000000000000000, 2.500000000000000000, -2.957883832488649833 ) ) ;
#57005 = CARTESIAN_POINT ( 'NONE',  ( -5.400000000000020783, 12.50000000000000000, 0.6928203230275494784 ) ) ;
#57006 = EDGE_LOOP ( 'NONE', ( #78732, #8442, #114999, #124340 ) ) ;
#57007 = CARTESIAN_POINT ( 'NONE',  ( -5.400000000000019895, 2.500000000000000000, -0.1000000000000022815 ) ) ;
#57008 = CARTESIAN_POINT ( 'NONE',  ( 6.249999999999928946, 2.500000000000000000, 2.757883832488649656 ) ) ;
#57009 = DIRECTION ( 'NONE',  ( -4.274815082592931898E-19, -0.9999939076577903929, -0.003490651415223739937 ) ) ;
#57010 = PLANE ( 'NONE',  #73595 ) ;
#57011 = DIRECTION ( 'NONE',  ( 0.000000000000000000, 0.000000000000000000, -1.000000000000000000 ) ) ;
#57012 = CIRCLE ( 'NONE', #8896, 0.06509327318403745899 ) ;
#57013 = ORIENTED_EDGE ( 'NONE', *, *, #7006, .F. ) ;
#57014 = ADVANCED_FACE ( 'NONE', ( #34372 ), #31737, .T. ) ;
#57015 = ORIENTED_EDGE ( 'NONE', *, *, #118114, .F. ) ;
#57016 = DIRECTION ( 'NONE',  ( 0.000000000000000000, 1.000000000000000000, 0.000000000000000000 ) ) ;
#57017 = ORIENTED_EDGE ( 'NONE', *, *, #20753, .T. ) ;
#57018 = DIRECTION ( 'NONE',  ( -0.000000000000000000, -1.000000000000000000, -0.000000000000000000 ) ) ;
#57020 = ORIENTED_EDGE ( 'NONE', *, *, #75814, .T. ) ;
#57019 = ORIENTED_EDGE ( 'NONE', *, *, #73835, .T. ) ;
#57021 = ORIENTED_EDGE ( 'NONE', *, *, #77336, .F. ) ;
#57022 = CARTESIAN_POINT ( 'NONE',  ( 145.7653593504141725, 2.500000000000000000, -3.576063159858998475 ) ) ;
#57023 = CIRCLE ( 'NONE', #100934, 0.06509327318403745899 ) ;
#57024 = CIRCLE ( 'NONE', #100935, 0.1000000000000002554 ) ;
#57025 = PLANE ( 'NONE',  #94465 ) ;
#57026 = VECTOR ( 'NONE', #75997, 1000.000000000000000 ) ;
#57027 = PLANE ( 'NONE',  #94949 ) ;
#57028 = PRESENTATION_STYLE_ASSIGNMENT (( #77327 ) ) ;
#57029 = DIRECTION ( 'NONE',  ( 0.000000000000000000, 0.000000000000000000, 1.000000000000000000 ) ) ;
#57030 = CARTESIAN_POINT ( 'NONE',  ( -8.750000000000007105, 12.50000000000000000, 7.253104124594885960 ) ) ;
#57031 = LINE ( 'NONE', #87140, #99883 ) ;
#57032 = ORIENTED_EDGE ( 'NONE', *, *, #49298, .T. ) ;
#57033 = CIRCLE ( 'NONE', #103007, 0.1000000000000000472 ) ;
#57034 = DIRECTION ( 'NONE',  ( 0.000000000000000000, -0.000000000000000000, 1.000000000000000000 ) ) ;
#57035 = ORIENTED_EDGE ( 'NONE', *, *, #40530, .T. ) ;
#57036 = AXIS2_PLACEMENT_3D ( 'NONE', #26283, #106753, #38023 ) ;
#57037 = ORIENTED_EDGE ( 'NONE', *, *, #37887, .T. ) ;
#57038 = ORIENTED_EDGE ( 'NONE', *, *, #42782, .F. ) ;
#57039 = AXIS2_PLACEMENT_3D ( 'NONE', #116014, #26364, #19081 ) ;
#57040 = VERTEX_POINT ( 'NONE', #93921 ) ;
#57041 = CARTESIAN_POINT ( 'NONE',  ( 0.3999999999999628852, 2.500000000000000000, -0.7928203230275520097 ) ) ;
#57042 = EDGE_LOOP ( 'NONE', ( #68267, #82211, #83672, #28972 ) ) ;
#57043 = ORIENTED_EDGE ( 'NONE', *, *, #61264, .F. ) ;
#57044 = AXIS2_PLACEMENT_3D ( 'NONE', #7699, #15585, #47007 ) ;
#57045 = VECTOR ( 'NONE', #109059, 1000.000000000000000 ) ;
#57046 = DIRECTION ( 'NONE',  ( 0.000000000000000000, 1.000000000000000000, 0.000000000000000000 ) ) ;
#57047 = LINE ( 'NONE', #5377, #96055 ) ;
#57048 = CARTESIAN_POINT ( 'NONE',  ( 0.6499999999999566125, 12.50000000000000000, -6.148780366869526226 ) ) ;
#57049 = CIRCLE ( 'NONE', #115527, 0.06509327318403745899 ) ;
#57050 = DIRECTION ( 'NONE',  ( -0.000000000000000000, -1.000000000000000000, -0.000000000000000000 ) ) ;
#57051 = VECTOR ( 'NONE', #18897, 1000.000000000000000 ) ;
#57052 = AXIS2_PLACEMENT_3D ( 'NONE', #75219, #105331, #35942 ) ;
#57053 = CARTESIAN_POINT ( 'NONE',  ( 4.799999999999935874, 2.500000000000000000, 0.4464101615137735513 ) ) ;
#57054 = VERTEX_POINT ( 'NONE', #23232 ) ;
#57055 = CONICAL_SURFACE ( 'NONE', #59236, 0.09999999999999982514, 0.003490658503988666988 ) ;
#57056 = DIRECTION ( 'NONE',  ( 0.000000000000000000, -0.9999939076577903929, 0.003490651415223739937 ) ) ;
#57057 = ORIENTED_EDGE ( 'NONE', *, *, #123892, .T. ) ;
#57058 = CARTESIAN_POINT ( 'NONE',  ( 0.4499999999999569344, 12.50000000000000000, -2.165063509461101710 ) ) ;
#57059 = EDGE_CURVE ( 'NONE', #180, #95907, #63163, .T. ) ;
#57060 = ORIENTED_EDGE ( 'NONE', *, *, #87244, .F. ) ;
#57061 = CIRCLE ( 'NONE', #50818, 0.06509327318403745899 ) ;
#57062 = CARTESIAN_POINT ( 'NONE',  ( 187.5000000000000000, 0.000000000000000000, 0.000000000000000000 ) ) ;
#57063 = ORIENTED_EDGE ( 'NONE', *, *, #54461, .T. ) ;
#57064 = ADVANCED_FACE ( 'NONE', ( #105675 ), #90292, .T. ) ;
#57065 = ORIENTED_EDGE ( 'NONE', *, *, #104277, .F. ) ;
#57066 = EDGE_CURVE ( 'NONE', #102156, #114764, #13409, .T. ) ;
#57067 = DIRECTION ( 'NONE',  ( 0.000000000000000000, 1.000000000000000000, 0.000000000000000000 ) ) ;
#57068 = DIRECTION ( 'NONE',  ( 0.000000000000000000, 0.000000000000000000, 1.000000000000000000 ) ) ;
#57069 = CARTESIAN_POINT ( 'NONE',  ( -1.850000000000033840, 2.500000000000000000, 1.918653347947321564 ) ) ;
#57070 = FACE_OUTER_BOUND ( 'NONE', #25360, .T. ) ;
#57071 = EDGE_CURVE ( 'NONE', #22838, #7097, #35647, .T. ) ;
#57072 = DIRECTION ( 'NONE',  ( -0.000000000000000000, -1.000000000000000000, -0.000000000000000000 ) ) ;
#57074 = ORIENTED_EDGE ( 'NONE', *, *, #74654, .T. ) ;
#57073 = ADVANCED_FACE ( 'NONE', ( #73618 ), #43547, .T. ) ;
#57075 = DIRECTION ( 'NONE',  ( 0.000000000000000000, -0.9999939076577903929, 0.003490651415223739937 ) ) ;
#57077 = VECTOR ( 'NONE', #12446, 1000.000000000000000 ) ;
#57076 = DIRECTION ( 'NONE',  ( 0.000000000000000000, 1.000000000000000000, 0.000000000000000000 ) ) ;
#57078 = EDGE_CURVE ( 'NONE', #14684, #67886, #42207, .T. ) ;
#57079 = CARTESIAN_POINT ( 'NONE',  ( 5.399999999999933742, 2.500000000000000000, -2.385244779468109755E-15 ) ) ;
#57080 = EDGE_CURVE ( 'NONE', #39251, #25440, #121605, .T. ) ;
#57081 = EDGE_CURVE ( 'NONE', #2046, #92765, #27599, .T. ) ;
#57082 = CARTESIAN_POINT ( 'NONE',  ( -13.34999999999999076, 12.50000000000000000, 2.922977105672690534 ) ) ;
#57083 = CARTESIAN_POINT ( 'NONE',  ( 8.349999999999923261, 2.500000000000000000, 1.472243186433545459 ) ) ;
#57084 = VERTEX_POINT ( 'NONE', #112913 ) ;
#57085 = CIRCLE ( 'NONE', #36179, 0.06509327318403745899 ) ;
#57086 = AXIS2_PLACEMENT_3D ( 'NONE', #104321, #53303, #71640 ) ;
#57087 = ORIENTED_EDGE ( 'NONE', *, *, #20197, .T. ) ;
#57088 = CIRCLE ( 'NONE', #21588, 0.06509327318403745899 ) ;
#57089 = CONICAL_SURFACE ( 'NONE', #36183, 0.1000000000000002554, 0.003490658503988666988 ) ;
#57090 = FACE_OUTER_BOUND ( 'NONE', #73267, .T. ) ;
#57091 = EDGE_CURVE ( 'NONE', #123590, #20895, #50598, .T. ) ;
#57092 = ORIENTED_EDGE ( 'NONE', *, *, #20632, .T. ) ;
#57093 = DIRECTION ( 'NONE',  ( 0.000000000000000000, -0.000000000000000000, 1.000000000000000000 ) ) ;
#57094 = DIRECTION ( 'NONE',  ( 0.000000000000000000, 0.000000000000000000, 1.000000000000000000 ) ) ;
#57095 = ADVANCED_FACE ( 'NONE', ( #95855 ), #123741, .T. ) ;
#57096 = AXIS2_PLACEMENT_3D ( 'NONE', #20722, #90082, #119546 ) ;
#57097 = AXIS2_PLACEMENT_3D ( 'NONE', #31717, #91923, #112212 ) ;
#57098 = AXIS2_PLACEMENT_3D ( 'NONE', #33236, #31932, #53508 ) ;
#57099 = AXIS2_PLACEMENT_3D ( 'NONE', #68166, #126462, #36799 ) ;
#57100 = ORIENTED_EDGE ( 'NONE', *, *, #26242, .F. ) ;
#57101 = CARTESIAN_POINT ( 'NONE',  ( 186.7083333333333428, -4.445597072760115509, -7.700000000000001954 ) ) ;
#57102 = CARTESIAN_POINT ( 'NONE',  ( -3.950000000000029932, 12.50000000000000000, -6.148780366869526226 ) ) ;
#57103 = CARTESIAN_POINT ( 'NONE',  ( -0.4000000000000401013, 12.50000000000000000, -3.702399969078687292 ) ) ;
#57104 = CARTESIAN_POINT ( 'NONE',  ( 2.099999999999950351, 2.500000000000000000, -0.6928203230275541413 ) ) ;
#57105 = CARTESIAN_POINT ( 'NONE',  ( -7.900000000000011013, 2.500000000000000000, 3.737306695894644371 ) ) ;
#57106 = ORIENTED_EDGE ( 'NONE', *, *, #811, .F. ) ;
#57107 = CIRCLE ( 'NONE', #101027, 0.06509327318403741736 ) ;
#57108 = CARTESIAN_POINT ( 'NONE',  ( 4.999999999999938716, 12.50000000000000000, -5.022947341949754119 ) ) ;
#57109 = LINE ( 'NONE', #47302, #51890 ) ;
#57110 = ORIENTED_EDGE ( 'NONE', *, *, #74520, .F. ) ;
#57111 = PLANE ( 'NONE',  #123787 ) ;
#57112 = DIRECTION ( 'NONE',  ( 0.000000000000000000, -0.000000000000000000, 1.000000000000000000 ) ) ;
#57113 = PLANE ( 'NONE',  #124319 ) ;
#57114 = AXIS2_PLACEMENT_3D ( 'NONE', #122648, #52610, #42832 ) ;
#57115 = ORIENTED_EDGE ( 'NONE', *, *, #117922, .T. ) ;
#57116 = CARTESIAN_POINT ( 'NONE',  ( 6.849999999999929479, 12.50000000000000000, 6.841600689897072485 ) ) ;
#57117 = ORIENTED_EDGE ( 'NONE', *, *, #43195, .T. ) ;
#57118 = ADVANCED_FACE ( 'NONE', ( #55285 ), #115325, .T. ) ;
#57119 = LINE ( 'NONE', #108150, #48027 ) ;
#57120 = CARTESIAN_POINT ( 'NONE',  ( -7.700000000000014388, 2.500000000000000000, -0.3464101615137782364 ) ) ;
#57121 = CARTESIAN_POINT ( 'NONE',  ( 9.799999999999913669, 12.50000000000000000, -4.048810130592463530 ) ) ;
#57122 = CIRCLE ( 'NONE', #100834, 2.000000000000000000 ) ;
#57123 = ADVANCED_FACE ( 'NONE', ( #44830 ), #2467, .T. ) ;
#57124 = ORIENTED_EDGE ( 'NONE', *, *, #10403, .F. ) ;
#57125 = CARTESIAN_POINT ( 'NONE',  ( -10.85000000000000142, 2.500000000000000000, 2.165063509461097713 ) ) ;
#57126 = ADVANCED_FACE ( 'NONE', ( #65078 ), #5516, .T. ) ;
#57127 = CARTESIAN_POINT ( 'NONE',  ( 185.3645833340161175, -6.668395609140180369, 3.849999999999994760 ) ) ;
#57128 = VERTEX_POINT ( 'NONE', #83471 ) ;
#57129 = DIRECTION ( 'NONE',  ( 0.000000000000000000, 1.000000000000000000, 0.000000000000000000 ) ) ;
#57130 = EDGE_CURVE ( 'NONE', #63832, #83854, #69375, .T. ) ;
#57131 = AXIS2_PLACEMENT_3D ( 'NONE', #90948, #59586, #20918 ) ;
#57132 = ORIENTED_EDGE ( 'NONE', *, *, #24549, .F. ) ;
#57133 = AXIS2_PLACEMENT_3D ( 'NONE', #122278, #60772, #61433 ) ;
#57134 = CARTESIAN_POINT ( 'NONE',  ( 3.149999999999946176, 12.50000000000000000, -6.776507416713039689 ) ) ;
#57135 = EDGE_CURVE ( 'NONE', #35861, #129348, #54690, .T. ) ;
#57136 = AXIS2_PLACEMENT_3D ( 'NONE', #27890, #48179, #18711 ) ;
#57137 = AXIS2_PLACEMENT_3D ( 'NONE', #122477, #23618, #111331 ) ;
#57138 = EDGE_CURVE ( 'NONE', #96874, #21203, #67667, .T. ) ;
#57139 = ORIENTED_EDGE ( 'NONE', *, *, #78096, .T. ) ;
#57140 = DIRECTION ( 'NONE',  ( 0.000000000000000000, 0.000000000000000000, 1.000000000000000000 ) ) ;
#57141 = CARTESIAN_POINT ( 'NONE',  ( 8.349999999999919709, 2.500000000000000000, -2.957883832488653830 ) ) ;
#57142 = EDGE_LOOP ( 'NONE', ( #82712, #27211, #21899, #79030 ) ) ;
#57143 = ORIENTED_EDGE ( 'NONE', *, *, #102644, .F. ) ;
#57144 = AXIS2_PLACEMENT_3D ( 'NONE', #49788, #113035, #74407 ) ;
#57145 = CARTESIAN_POINT ( 'NONE',  ( 2.699999999999947331, 12.50000000000000000, -4.676537180435978769 ) ) ;
#57146 = DIRECTION ( 'NONE',  ( 0.000000000000000000, 0.000000000000000000, 1.000000000000000000 ) ) ;
#57147 = VERTEX_POINT ( 'NONE', #27113 ) ;
#57148 = EDGE_CURVE ( 'NONE', #126044, #46262, #116125, .T. ) ;
#57149 = DIRECTION ( 'NONE',  ( 0.000000000000000000, 0.000000000000000000, -1.000000000000000000 ) ) ;
#57150 = DIRECTION ( 'NONE',  ( 0.000000000000000000, 0.000000000000000000, -1.000000000000000000 ) ) ;
#57151 = AXIS2_PLACEMENT_3D ( 'NONE', #128662, #10753, #31095 ) ;
#57152 = AXIS2_PLACEMENT_3D ( 'NONE', #86688, #126630, #14703 ) ;
#57153 = DIRECTION ( 'NONE',  ( 0.000000000000000000, 0.000000000000000000, 1.000000000000000000 ) ) ;
#57154 = CARTESIAN_POINT ( 'NONE',  ( -11.64999999999999680, 2.500000000000000000, 2.857883832488649301 ) ) ;
#57155 = CARTESIAN_POINT ( 'NONE',  ( 179.5000000000000000, -1.375000000000002442, -7.576237522675751457 ) ) ;
#57156 = CARTESIAN_POINT ( 'NONE',  ( -1.650000000000034328, 2.500000000000000000, -6.395190528383301931 ) ) ;
#57157 = ORIENTED_EDGE ( 'NONE', *, *, #75378, .F. ) ;
#57158 = ORIENTED_EDGE ( 'NONE', *, *, #25963, .F. ) ;
#57159 = EDGE_LOOP ( 'NONE', ( #31790, #46166 ) ) ;
#57160 = ORIENTED_EDGE ( 'NONE', *, *, #11190, .T. ) ;
#57161 = CARTESIAN_POINT ( 'NONE',  ( -4.400000000000025224, 2.500000000000000000, 4.676537180435972552 ) ) ;
#57162 = DIRECTION ( 'NONE',  ( 0.000000000000000000, 0.000000000000000000, -1.000000000000000000 ) ) ;
#57163 = DIRECTION ( 'NONE',  ( 0.000000000000000000, 0.000000000000000000, -1.000000000000000000 ) ) ;
#57164 = ORIENTED_EDGE ( 'NONE', *, *, #102136, .F. ) ;
#57165 = FACE_BOUND ( 'NONE', #100321, .T. ) ;
#57166 = EDGE_CURVE ( 'NONE', #125289, #118069, #63124, .T. ) ;
#57167 = CARTESIAN_POINT ( 'NONE',  ( 2.299999999999949640, 12.50000000000000000, -0.2813168883297408329 ) ) ;
#57168 = DIRECTION ( 'NONE',  ( 0.000000000000000000, 0.000000000000000000, 1.000000000000000000 ) ) ;
#57169 = CARTESIAN_POINT ( 'NONE',  ( 1.849999999999950573, 12.50000000000000000, 2.576566944158910744 ) ) ;
#57170 = CARTESIAN_POINT ( 'NONE',  ( 11.04999999999991189, 2.500000000000000000, -2.411473670974877859 ) ) ;
#57171 = CARTESIAN_POINT ( 'NONE',  ( 127.5000000000000000, 0.000000000000000000, 0.000000000000000000 ) ) ;
#57172 = FACE_OUTER_BOUND ( 'NONE', #104861, .T. ) ;
#57173 = FACE_OUTER_BOUND ( 'NONE', #95159, .T. ) ;
#57174 = CARTESIAN_POINT ( 'NONE',  ( -13.94999999999998685, 2.500000000000000000, 1.818653347947325472 ) ) ;
#57175 = CIRCLE ( 'NONE', #38313, 0.06509327318403745899 ) ;
#57176 = CONICAL_SURFACE ( 'NONE', #90617, 0.1000000000000002554, 0.003490658503988666988 ) ;
#57177 = DIRECTION ( 'NONE',  ( -0.000000000000000000, 1.000000000000000000, -0.000000000000000000 ) ) ;
#57178 = DIRECTION ( 'NONE',  ( 0.000000000000000000, -0.9999939076577903929, 0.003490651415223739937 ) ) ;
#57179 = CIRCLE ( 'NONE', #59262, 0.1000000000000002554 ) ;
#57181 = ORIENTED_EDGE ( 'NONE', *, *, #551, .T. ) ;
#57180 = CIRCLE ( 'NONE', #73905, 0.09999999999999982514 ) ;
#57182 = ORIENTED_EDGE ( 'NONE', *, *, #47335, .F. ) ;
#57183 = EDGE_CURVE ( 'NONE', #125596, #68600, #46384, .T. ) ;
#57184 = ORIENTED_EDGE ( 'NONE', *, *, #62911, .T. ) ;
#57185 = CIRCLE ( 'NONE', #124077, 0.09999999999999982514 ) ;
#57186 = VERTEX_POINT ( 'NONE', #57871 ) ;
#57188 = CIRCLE ( 'NONE', #73907, 0.1000000000000002554 ) ;
#57187 = CARTESIAN_POINT ( 'NONE',  ( 17.50000000000010658, -2.362777783881773175, -3.757134105505308685 ) ) ;
#57189 = AXIS2_PLACEMENT_3D ( 'NONE', #117413, #38256, #89279 ) ;
#57190 = CARTESIAN_POINT ( 'NONE',  ( -2.100000000000034728, 2.500000000000000000, 4.330127018922196314 ) ) ;
#57192 = ORIENTED_EDGE ( 'NONE', *, *, #62469, .T. ) ;
#57191 = EDGE_LOOP ( 'NONE', ( #35283, #81760 ) ) ;
#57193 = ORIENTED_EDGE ( 'NONE', *, *, #124165, .F. ) ;
#57194 = DIRECTION ( 'NONE',  ( -0.000000000000000000, 1.000000000000000000, -0.000000000000000000 ) ) ;
#57195 = AXIS2_PLACEMENT_3D ( 'NONE', #55003, #126335, #53717 ) ;
#57196 = VECTOR ( 'NONE', #78793, 1000.000000000000000 ) ;
#57197 = AXIS2_PLACEMENT_3D ( 'NONE', #122668, #33023, #23170 ) ;
#57198 = CARTESIAN_POINT ( 'NONE',  ( 8.549999999999918998, 2.500000000000000000, -1.818653347947326138 ) ) ;
#57199 = FACE_OUTER_BOUND ( 'NONE', #848, .T. ) ;
#57200 = LINE ( 'NONE', #116114, #124462 ) ;
#57201 = CARTESIAN_POINT ( 'NONE',  ( 187.2812500006828031, 0.000000000000000000, 7.700000000000000178 ) ) ;
#57202 = AXIS2_PLACEMENT_3D ( 'NONE', #84442, #34056, #113911 ) ;
#57203 = EDGE_CURVE ( 'NONE', #45959, #90163, #87940, .T. ) ;
#57204 = ORIENTED_EDGE ( 'NONE', *, *, #115021, .F. ) ;
#57205 = DIRECTION ( 'NONE',  ( 0.000000000000000000, 0.000000000000000000, 1.000000000000000000 ) ) ;
#57206 = EDGE_LOOP ( 'NONE', ( #3580, #124623, #1484, #85299 ) ) ;
#57207 = EDGE_LOOP ( 'NONE', ( #90059, #24343, #118054, #3441 ) ) ;
#57208 = ORIENTED_EDGE ( 'NONE', *, *, #24356, .F. ) ;
#57209 = DIRECTION ( 'NONE',  ( 0.000000000000000000, 1.000000000000000000, 0.000000000000000000 ) ) ;
#57210 = ORIENTED_EDGE ( 'NONE', *, *, #125522, .F. ) ;
#57211 = ORIENTED_EDGE ( 'NONE', *, *, #112117, .F. ) ;
#57212 = CIRCLE ( 'NONE', #111593, 0.09999999999999982514 ) ;
#57213 = CARTESIAN_POINT ( 'NONE',  ( -4.800000000000024691, 12.50000000000000000, 4.741630453620009789 ) ) ;
#57214 = DIRECTION ( 'NONE',  ( -0.000000000000000000, 1.000000000000000000, -0.000000000000000000 ) ) ;
#57215 = DIRECTION ( 'NONE',  ( -0.000000000000000000, 1.000000000000000000, -0.000000000000000000 ) ) ;
#57216 = CARTESIAN_POINT ( 'NONE',  ( -3.350000000000028955, 2.500000000000000000, -2.065063509461102065 ) ) ;
#57217 = DIRECTION ( 'NONE',  ( -0.000000000000000000, -1.000000000000000000, -0.000000000000000000 ) ) ;
#57219 = VERTEX_POINT ( 'NONE', #127888 ) ;
#57218 = VECTOR ( 'NONE', #17329, 1000.000000000000000 ) ;
#57220 = LINE ( 'NONE', #7465, #51217 ) ;
#57221 = AXIS2_PLACEMENT_3D ( 'NONE', #92404, #20460, #42701 ) ;
#57222 = CIRCLE ( 'NONE', #44717, 0.06509327318403745899 ) ;
#57223 = ORIENTED_EDGE ( 'NONE', *, *, #10316, .T. ) ;
#57224 = ADVANCED_FACE ( 'NONE', ( #37590 ), #10954, .T. ) ;
#57225 = ORIENTED_EDGE ( 'NONE', *, *, #54864, .T. ) ;
#57226 = CARTESIAN_POINT ( 'NONE',  ( -6.071532165918824830E-15, 12.50000000000000000, -4.265033745738164406 ) ) ;
#57227 = FACE_OUTER_BOUND ( 'NONE', #4863, .T. ) ;
#57228 = ORIENTED_EDGE ( 'NONE', *, *, #8312, .T. ) ;
#57229 = FACE_BOUND ( 'NONE', #91684, .T. ) ;
#57231 = CIRCLE ( 'NONE', #30055, 0.06509327318403745899 ) ;
#57230 = DIRECTION ( 'NONE',  ( 0.000000000000000000, 0.000000000000000000, 1.000000000000000000 ) ) ;
#57232 = ORIENTED_EDGE ( 'NONE', *, *, #30386, .T. ) ;
#57233 = AXIS2_PLACEMENT_3D ( 'NONE', #29866, #69785, #77662 ) ;
#57235 = EDGE_CURVE ( 'NONE', #59940, #80507, #100855, .T. ) ;
#57234 = AXIS2_PLACEMENT_3D ( 'NONE', #36928, #8090, #48677 ) ;
#57236 = AXIS2_PLACEMENT_3D ( 'NONE', #99938, #11541, #60664 ) ;
#57237 = CARTESIAN_POINT ( 'NONE',  ( -6.900000000000015454, 2.500000000000000000, 4.676537180435972552 ) ) ;
#57238 = ORIENTED_EDGE ( 'NONE', *, *, #52833, .T. ) ;
#57239 = EDGE_CURVE ( 'NONE', #98343, #71326, #69464, .T. ) ;
#57241 = VERTEX_POINT ( 'NONE', #108244 ) ;
#57240 = EDGE_CURVE ( 'NONE', #47265, #55655, #92457, .T. ) ;
#57242 = CARTESIAN_POINT ( 'NONE',  ( -9.400000000000007461, 12.50000000000000000, 0.4115034346978109769 ) ) ;
#57243 = DIRECTION ( 'NONE',  ( 0.000000000000000000, 0.000000000000000000, 1.000000000000000000 ) ) ;
#57244 = ADVANCED_FACE ( 'NONE', ( #46760 ), #44434, .T. ) ;
#57245 = CARTESIAN_POINT ( 'NONE',  ( 185.2552083336747444, 6.551208109652275624, -3.782341765624998686 ) ) ;
#57247 = EDGE_CURVE ( 'NONE', #11699, #104109, #59163, .T. ) ;
#57246 = CONICAL_SURFACE ( 'NONE', #119937, 0.1000000000000002554, 0.003490658503988666988 ) ;
#57248 = DIRECTION ( 'NONE',  ( -4.274815082592931898E-19, -0.9999939076577903929, -0.003490651415223739937 ) ) ;
#57249 = DIRECTION ( 'NONE',  ( 0.000000000000000000, 1.000000000000000000, 0.000000000000000000 ) ) ;
#57251 = ADVANCED_FACE ( 'NONE', ( #6788 ), #61161, .T. ) ;
#57250 = AXIS2_PLACEMENT_3D ( 'NONE', #59071, #89170, #59736 ) ;
#57252 = CONICAL_SURFACE ( 'NONE', #103217, 0.1000000000000002554, 0.003490658503988666988 ) ;
#57253 = AXIS2_PLACEMENT_3D ( 'NONE', #97284, #18071, #39046 ) ;
#57254 = CARTESIAN_POINT ( 'NONE',  ( 0.1999999999999636513, 2.500000000000000000, -0.4464101615137760493 ) ) ;
#57255 = EDGE_CURVE ( 'NONE', #126313, #92073, #113385, .T. ) ;
#57256 = EDGE_CURVE ( 'NONE', #112457, #52060, #71617, .T. ) ;
#57257 = EDGE_LOOP ( 'NONE', ( #27046, #518 ) ) ;
#57258 = CIRCLE ( 'NONE', #53059, 0.06509327318403745899 ) ;
#57259 = EDGE_CURVE ( 'NONE', #105130, #27833, #104960, .T. ) ;
#57260 = LINE ( 'NONE', #55956, #52747 ) ;
#57261 = PLANE ( 'NONE',  #47933 ) ;
#57262 = ADVANCED_FACE ( 'NONE', ( #125939 ), #26472, .T. ) ;
#57263 = ORIENTED_EDGE ( 'NONE', *, *, #72734, .F. ) ;
#57264 = FACE_OUTER_BOUND ( 'NONE', #91831, .T. ) ;
#57265 = CARTESIAN_POINT ( 'NONE',  ( -7.950000000000009059, 2.500000000000000000, 6.395190528383296602 ) ) ;
#57266 = FACE_OUTER_BOUND ( 'NONE', #72575, .T. ) ;
#57267 = FACE_OUTER_BOUND ( 'NONE', #129309, .T. ) ;
#57268 = EDGE_CURVE ( 'NONE', #91341, #96622, #16624, .T. ) ;
#57269 = LINE ( 'NONE', #62749, #76698 ) ;
#57270 = VERTEX_POINT ( 'NONE', #116769 ) ;
#57271 = CARTESIAN_POINT ( 'NONE',  ( 11.64999999999990443, 2.500000000000000000, -7.188010851410854052 ) ) ;
#57272 = CARTESIAN_POINT ( 'NONE',  ( -13.54999999999998828, 12.50000000000000000, -2.446380397790838046 ) ) ;
#57273 = VECTOR ( 'NONE', #24174, 1000.000000000000000 ) ;
#57274 = VERTEX_POINT ( 'NONE', #106942 ) ;
#57275 = DIRECTION ( 'NONE',  ( 0.000000000000000000, 0.000000000000000000, 1.000000000000000000 ) ) ;
#57276 = CONICAL_SURFACE ( 'NONE', #122137, 0.1000000000000002554, 0.003490658503988666988 ) ;
#57277 = VERTEX_POINT ( 'NONE', #57213 ) ;
#57278 = CONICAL_SURFACE ( 'NONE', #117906, 0.09999999999999982514, 0.003490658503988666988 ) ;
#57279 = ORIENTED_EDGE ( 'NONE', *, *, #40319, .T. ) ;
#57280 = MANIFOLD_SOLID_BREP ( 'Boss-Extrude2', #89605 ) ;
#57281 = DIRECTION ( 'NONE',  ( 0.000000000000000000, 0.000000000000000000, -1.000000000000000000 ) ) ;
#57282 = AXIS2_PLACEMENT_3D ( 'NONE', #71053, #43542, #22616 ) ;
#57283 = VERTEX_POINT ( 'NONE', #89253 ) ;
#57284 = DIRECTION ( 'NONE',  ( 0.000000000000000000, 0.000000000000000000, 1.000000000000000000 ) ) ;
#57285 = CARTESIAN_POINT ( 'NONE',  ( -5.850000000000019185, 12.50000000000000000, 2.099970236277060032 ) ) ;
#57286 = DIRECTION ( 'NONE',  ( -0.000000000000000000, 1.000000000000000000, -0.000000000000000000 ) ) ;
#57288 = ORIENTED_EDGE ( 'NONE', *, *, #10980, .T. ) ;
#57287 = AXIS2_PLACEMENT_3D ( 'NONE', #22196, #51011, #1245 ) ;
#57289 = VECTOR ( 'NONE', #115963, 1000.000000000000000 ) ;
#57290 = AXIS2_PLACEMENT_3D ( 'NONE', #104163, #24956, #84521 ) ;
#57291 = FACE_BOUND ( 'NONE', #32962, .T. ) ;
#57293 = VERTEX_POINT ( 'NONE', #101661 ) ;
#57292 = DIRECTION ( 'NONE',  ( 0.000000000000000000, 0.000000000000000000, 1.000000000000000000 ) ) ;
#57294 = VECTOR ( 'NONE', #87646, 1000.000000000000000 ) ;
#57295 = CARTESIAN_POINT ( 'NONE',  ( 87.50000000000001421, 0.000000000000000000, 0.000000000000000000 ) ) ;
#57296 = DIRECTION ( 'NONE',  ( 0.000000000000000000, 1.000000000000000000, 0.000000000000000000 ) ) ;
#57297 = EDGE_LOOP ( 'NONE', ( #47398, #24611 ) ) ;
#57298 = EDGE_CURVE ( 'NONE', #112590, #79702, #38180, .T. ) ;
#57299 = VERTEX_POINT ( 'NONE', #82006 ) ;
#57300 = EDGE_CURVE ( 'NONE', #113115, #86732, #8815, .T. ) ;
#57301 = ORIENTED_EDGE ( 'NONE', *, *, #96216, .T. ) ;
#57303 = AXIS2_PLACEMENT_3D ( 'NONE', #68954, #117376, #67656 ) ;
#57302 = CARTESIAN_POINT ( 'NONE',  ( 4.399999999999939071, 2.500000000000000000, 0.4464101615137736623 ) ) ;
#57304 = DIRECTION ( 'NONE',  ( 0.000000000000000000, 1.000000000000000000, 0.000000000000000000 ) ) ;
#57305 = DIRECTION ( 'NONE',  ( 0.000000000000000000, 0.000000000000000000, 1.000000000000000000 ) ) ;
#57306 = FACE_BOUND ( 'NONE', #93087, .T. ) ;
#57307 = ORIENTED_EDGE ( 'NONE', *, *, #55536, .T. ) ;
#57308 = CARTESIAN_POINT ( 'NONE',  ( -3.100000000000028511, 12.50000000000000000, -0.2813168883297408329 ) ) ;
#57309 = DIRECTION ( 'NONE',  ( 0.000000000000000000, 0.000000000000000000, 1.000000000000000000 ) ) ;
#57310 = CONICAL_SURFACE ( 'NONE', #115790, 0.1000000000000002554, 0.003490658503988666988 ) ;
#57311 = ORIENTED_EDGE ( 'NONE', *, *, #3181, .F. ) ;
#57312 = ADVANCED_FACE ( 'NONE', ( #39545 ), #42294, .T. ) ;
#57313 = PLANE ( 'NONE',  #126488 ) ;
#57314 = CARTESIAN_POINT ( 'NONE',  ( 2.899999999999944844, 2.500000000000000000, 4.922947341949748257 ) ) ;
#57315 = CARTESIAN_POINT ( 'NONE',  ( 9.549999999999918998, 2.500000000000000000, -6.495190528383302464 ) ) ;
#57316 = CARTESIAN_POINT ( 'NONE',  ( 8.949999999999919353, 2.500000000000000000, 2.511473670974873507 ) ) ;
#57317 = DIRECTION ( 'NONE',  ( -0.000000000000000000, -1.000000000000000000, -0.000000000000000000 ) ) ;
#57318 = AXIS2_PLACEMENT_3D ( 'NONE', #50895, #118982, #47189 ) ;
#57319 = VECTOR ( 'NONE', #6539, 1000.000000000000000 ) ;
#57320 = ORIENTED_EDGE ( 'NONE', *, *, #36725, .T. ) ;
#57321 = ORIENTED_EDGE ( 'NONE', *, *, #56900, .F. ) ;
#57322 = ORIENTED_EDGE ( 'NONE', *, *, #89431, .T. ) ;
#57323 = EDGE_LOOP ( 'NONE', ( #70707, #39486, #123254, #19577 ) ) ;
#57324 = ORIENTED_EDGE ( 'NONE', *, *, #74667, .T. ) ;
#57325 = LINE ( 'NONE', #7561, #38062 ) ;
#57326 = DIRECTION ( 'NONE',  ( 0.000000000000000000, 1.000000000000000000, 0.000000000000000000 ) ) ;
#57327 = ORIENTED_EDGE ( 'NONE', *, *, #2846, .T. ) ;
#57328 = FACE_BOUND ( 'NONE', #25307, .T. ) ;
#57329 = DIRECTION ( 'NONE',  ( -0.000000000000000000, 1.000000000000000000, -0.000000000000000000 ) ) ;
#57330 = AXIS2_PLACEMENT_3D ( 'NONE', #90591, #33619, #83985 ) ;
#57331 = CARTESIAN_POINT ( 'NONE',  ( -0.8000000000000315747, 2.500000000000000000, 0.000000000000000000 ) ) ;
#57332 = DIRECTION ( 'NONE',  ( 0.000000000000000000, 0.000000000000000000, -1.000000000000000000 ) ) ;
#57333 = FACE_OUTER_BOUND ( 'NONE', #64727, .T. ) ;
#57334 = CARTESIAN_POINT ( 'NONE',  ( -8.350000000000013856, 12.50000000000000000, -7.188010851410848723 ) ) ;
#57335 = EDGE_LOOP ( 'NONE', ( #123642, #85581 ) ) ;
#57336 = DIRECTION ( 'NONE',  ( 0.000000000000000000, 0.000000000000000000, 1.000000000000000000 ) ) ;
#57337 = ORIENTED_EDGE ( 'NONE', *, *, #22342, .T. ) ;
#57338 = CIRCLE ( 'NONE', #99117, 0.06509327318403745899 ) ;
#57339 = VECTOR ( 'NONE', #10805, 1000.000000000000000 ) ;
#57340 = EDGE_LOOP ( 'NONE', ( #74193, #85607, #127744, #108154 ) ) ;
#57341 = ORIENTED_EDGE ( 'NONE', *, *, #126225, .T. ) ;
#57342 = DIRECTION ( 'NONE',  ( -4.274815082592931898E-19, -0.9999939076577903929, -0.003490651415223739937 ) ) ;
#57343 = CARTESIAN_POINT ( 'NONE',  ( 108.0000000000000142, 8.500000000000000000, -0.2500000000000000000 ) ) ;
#57344 = DIRECTION ( 'NONE',  ( -0.000000000000000000, 1.000000000000000000, -0.000000000000000000 ) ) ;
#57345 = ORIENTED_EDGE ( 'NONE', *, *, #5051, .F. ) ;
#57346 = CARTESIAN_POINT ( 'NONE',  ( 14.69205215096538097, 2.499999999999999556, -6.336420066640663151 ) ) ;
#57347 = AXIS2_PLACEMENT_3D ( 'NONE', #110422, #72442, #51516 ) ;
#57348 = DIRECTION ( 'NONE',  ( -0.000000000000000000, -1.000000000000000000, -0.000000000000000000 ) ) ;
#57349 = DIRECTION ( 'NONE',  ( 0.000000000000000000, 1.000000000000000000, 0.000000000000000000 ) ) ;
#57350 = CARTESIAN_POINT ( 'NONE',  ( 186.4427083336747160, -6.551208109652278289, 3.782341765624995134 ) ) ;
#57351 = FACE_OUTER_BOUND ( 'NONE', #116668, .T. ) ;
#57352 = LINE ( 'NONE', #118206, #119838 ) ;
#57353 = EDGE_CURVE ( 'NONE', #113894, #79929, #2154, .T. ) ;
#57354 = LINE ( 'NONE', #75689, #11916 ) ;
#57355 = EDGE_CURVE ( 'NONE', #123793, #17546, #110190, .T. ) ;
#57356 = ORIENTED_EDGE ( 'NONE', *, *, #127579, .F. ) ;
#57357 = CARTESIAN_POINT ( 'NONE',  ( -12.94999999999999218, 2.500000000000000000, -2.065063509461099844 ) ) ;
#57358 = ORIENTED_EDGE ( 'NONE', *, *, #55916, .F. ) ;
#57360 = ORIENTED_EDGE ( 'NONE', *, *, #48303, .T. ) ;
#57359 = AXIS2_PLACEMENT_3D ( 'NONE', #106172, #116621, #66874 ) ;
#57361 = DIRECTION ( 'NONE',  ( 0.000000000000000000, 1.000000000000000000, 0.000000000000000000 ) ) ;
#57362 = CIRCLE ( 'NONE', #80356, 0.06509327318403745899 ) ;
#57363 = VECTOR ( 'NONE', #50158, 1000.000000000000000 ) ;
#57364 = LINE ( 'NONE', #19354, #32142 ) ;
#57365 = AXIS2_PLACEMENT_3D ( 'NONE', #110462, #20801, #111082 ) ;
#57367 = EDGE_CURVE ( 'NONE', #75768, #7162, #94593, .T. ) ;
#57366 = CARTESIAN_POINT ( 'NONE',  ( -4.600000000000028955, 12.50000000000000000, -4.330127018922201643 ) ) ;
#57368 = ORIENTED_EDGE ( 'NONE', *, *, #100305, .T. ) ;
#57369 = ORIENTED_EDGE ( 'NONE', *, *, #32344, .T. ) ;
#57370 = DIRECTION ( 'NONE',  ( -0.000000000000000000, 1.000000000000000000, -0.000000000000000000 ) ) ;
#57371 = CONICAL_SURFACE ( 'NONE', #51036, 0.09999999999999982514, 0.003490658503988666988 ) ;
#57372 = CIRCLE ( 'NONE', #934, 0.1000000000000002554 ) ;
#57373 = CIRCLE ( 'NONE', #53184, 0.1000000000000000472 ) ;
#57374 = CARTESIAN_POINT ( 'NONE',  ( -12.09999999999999609, 2.500000000000000000, 1.734723475976807094E-15 ) ) ;
#57375 = DIRECTION ( 'NONE',  ( 0.000000000000000000, 0.000000000000000000, 1.000000000000000000 ) ) ;
#57376 = ORIENTED_EDGE ( 'NONE', *, *, #13824, .F. ) ;
#57377 = EDGE_LOOP ( 'NONE', ( #86063, #34550 ) ) ;
#57378 = CARTESIAN_POINT ( 'NONE',  ( -1.450000000000035483, 12.50000000000000000, 6.148780366869520897 ) ) ;
#57379 = EDGE_LOOP ( 'NONE', ( #106761, #98619, #95180, #41784 ) ) ;
#57380 = CARTESIAN_POINT ( 'NONE',  ( 1.699999999999950218, 12.50000000000000000, 4.330127018922196314 ) ) ;
#57381 = CIRCLE ( 'NONE', #78328, 0.06509327318403745899 ) ;
#57382 = AXIS2_PLACEMENT_3D ( 'NONE', #94833, #35912, #124939 ) ;
#57383 = CARTESIAN_POINT ( 'NONE',  ( 4.149999999999938183, 2.500000000000000000, 7.188010851410848723 ) ) ;
#57384 = EDGE_LOOP ( 'NONE', ( #116473, #77846 ) ) ;
#57385 = DIRECTION ( 'NONE',  ( -0.000000000000000000, 1.000000000000000000, -0.000000000000000000 ) ) ;
#57386 = EDGE_CURVE ( 'NONE', #3394, #111598, #54892, .T. ) ;
#57387 = CARTESIAN_POINT ( 'NONE',  ( 2.099999999999950351, 2.500000000000000000, 0.09999999999999772959 ) ) ;
#57388 = DIRECTION ( 'NONE',  ( -0.000000000000000000, -1.000000000000000000, -0.000000000000000000 ) ) ;
#57389 = AXIS2_PLACEMENT_3D ( 'NONE', #36498, #126796, #106503 ) ;
#57390 = DIRECTION ( 'NONE',  ( -0.000000000000000000, -1.000000000000000000, -0.000000000000000000 ) ) ;
#57391 = EDGE_LOOP ( 'NONE', ( #22489, #52946 ) ) ;
#57392 = ADVANCED_FACE ( 'NONE', ( #109546 ), #125895, .T. ) ;
#57393 = FACE_OUTER_BOUND ( 'NONE', #77959, .T. ) ;
#57394 = CARTESIAN_POINT ( 'NONE',  ( -3.150000000000029221, 2.500000000000000000, 2.611473670974873151 ) ) ;
#57395 = ORIENTED_EDGE ( 'NONE', *, *, #52681, .F. ) ;
#57396 = VERTEX_POINT ( 'NONE', #30357 ) ;
#57397 = EDGE_CURVE ( 'NONE', #15907, #92009, #29763, .T. ) ;
#57398 = EDGE_CURVE ( 'NONE', #24838, #7948, #71528, .T. ) ;
#57399 = CARTESIAN_POINT ( 'NONE',  ( 4.799999999999937650, 12.50000000000000000, -4.048810130592463530 ) ) ;
#57400 = CARTESIAN_POINT ( 'NONE',  ( -4.600000000000025402, 12.50000000000000000, -2.385244779468109755E-15 ) ) ;
#57401 = CARTESIAN_POINT ( 'NONE',  ( 12.04999999999990834, 12.50000000000000000, -2.165063509461101710 ) ) ;
#57402 = EDGE_CURVE ( 'NONE', #47269, #109878, #119636, .T. ) ;
#57403 = FACE_OUTER_BOUND ( 'NONE', #116969, .T. ) ;
#57404 = ADVANCED_FACE ( 'NONE', ( #50609 ), #88224, .T. ) ;
#57405 = AXIS2_PLACEMENT_3D ( 'NONE', #57816, #27690, #57162 ) ;
#57406 = DIRECTION ( 'NONE',  ( 0.000000000000000000, 1.000000000000000000, 0.000000000000000000 ) ) ;
#57407 = DIRECTION ( 'NONE',  ( 0.000000000000000000, 0.000000000000000000, 1.000000000000000000 ) ) ;
#57408 = DIRECTION ( 'NONE',  ( -0.000000000000000000, -1.000000000000000000, -0.000000000000000000 ) ) ;
#57409 = CARTESIAN_POINT ( 'NONE',  ( 9.549999999999918998, 2.500000000000000000, 2.165063509461097713 ) ) ;
#57410 = CARTESIAN_POINT ( 'NONE',  ( -5.200000000000022382, 2.500000000000000000, 4.676537180435972552 ) ) ;
#57411 = EDGE_CURVE ( 'NONE', #101516, #42047, #121699, .T. ) ;
#57412 = EDGE_CURVE ( 'NONE', #123389, #62648, #81994, .T. ) ;
#57414 = CIRCLE ( 'NONE', #969, 0.09999999999999982514 ) ;
#57413 = CARTESIAN_POINT ( 'NONE',  ( -3.350000000000028511, 12.50000000000000000, 2.792790559304612064 ) ) ;
#57415 = VECTOR ( 'NONE', #107202, 1000.000000000000000 ) ;
#57416 = ADVANCED_FACE ( 'NONE', ( #53211 ), #21545, .T. ) ;
#57417 = EDGE_CURVE ( 'NONE', #8747, #36304, #75818, .T. ) ;
#57418 = ORIENTED_EDGE ( 'NONE', *, *, #19203, .F. ) ;
#57419 = CARTESIAN_POINT ( 'NONE',  ( 11.64999999999990798, 12.50000000000000000, 7.188010851410848723 ) ) ;
#57420 = ADVANCED_FACE ( 'NONE', ( #115301 ), #109272, .T. ) ;
#57421 = CARTESIAN_POINT ( 'NONE',  ( 10.84999999999990905, 12.50000000000000000, -5.802370205355749988 ) ) ;
#57422 = DIRECTION ( 'NONE',  ( 0.000000000000000000, 1.000000000000000000, 0.000000000000000000 ) ) ;
#57423 = CARTESIAN_POINT ( 'NONE',  ( -9.200000000000006395, 2.500000000000000000, 4.330127018922196314 ) ) ;
#57424 = ADVANCED_FACE ( 'NONE', ( #65586 ), #13251, .T. ) ;
#57425 = ORIENTED_EDGE ( 'NONE', *, *, #91988, .T. ) ;
#57426 = CARTESIAN_POINT ( 'NONE',  ( -4.600000000000025402, 2.500000000000000000, 4.330127018922196314 ) ) ;
#57427 = AXIS2_PLACEMENT_3D ( 'NONE', #124577, #66921, #8637 ) ;
#57428 = AXIS2_PLACEMENT_3D ( 'NONE', #47188, #15103, #45896 ) ;
#57429 = CARTESIAN_POINT ( 'NONE',  ( 6.049999999999934097, 12.50000000000000000, 6.213873640053559022 ) ) ;
#57431 = ORIENTED_EDGE ( 'NONE', *, *, #70681, .F. ) ;
#57430 = CARTESIAN_POINT ( 'NONE',  ( 2.899999999999945732, 12.50000000000000000, -4.265033745738164406 ) ) ;
#57432 = ORIENTED_EDGE ( 'NONE', *, *, #127000, .T. ) ;
#57433 = AXIS2_PLACEMENT_3D ( 'NONE', #64544, #51044, #41865 ) ;
#57434 = CIRCLE ( 'NONE', #21856, 0.06509327318403745899 ) ;
#57435 = ORIENTED_EDGE ( 'NONE', *, *, #57256, .F. ) ;
#57436 = EDGE_LOOP ( 'NONE', ( #62211, #63799 ) ) ;
#57437 = ORIENTED_EDGE ( 'NONE', *, *, #101185, .F. ) ;
#57438 = DIRECTION ( 'NONE',  ( 0.000000000000000000, 1.000000000000000000, 0.000000000000000000 ) ) ;
#57439 = AXIS2_PLACEMENT_3D ( 'NONE', #73120, #73743, #113692 ) ;
#57440 = DIRECTION ( 'NONE',  ( -0.000000000000000000, -1.000000000000000000, -0.000000000000000000 ) ) ;
#57441 = FACE_OUTER_BOUND ( 'NONE', #83759, .T. ) ;
#57442 = AXIS2_PLACEMENT_3D ( 'NONE', #19961, #59907, #103016 ) ;
#57443 = DIRECTION ( 'NONE',  ( 0.000000000000000000, 0.000000000000000000, -1.000000000000000000 ) ) ;
#57444 = VERTEX_POINT ( 'NONE', #75400 ) ;
#57445 = CARTESIAN_POINT ( 'NONE',  ( 5.799999999999934985, 12.50000000000000000, -4.395220292106239768 ) ) ;
#57446 = EDGE_LOOP ( 'NONE', ( #76840, #64291 ) ) ;
#57447 = CARTESIAN_POINT ( 'NONE',  ( 48.84100846713599253, -2.320798421931173028, -5.300800859552192712 ) ) ;
#57448 = DIRECTION ( 'NONE',  ( -0.000000000000000000, -1.000000000000000000, -0.000000000000000000 ) ) ;
#57449 = CARTESIAN_POINT ( 'NONE',  ( 0.1999999999999576006, 2.500000000000000000, -4.576537180435978236 ) ) ;
#57450 = DIRECTION ( 'NONE',  ( 0.000000000000000000, 1.000000000000000000, 0.000000000000000000 ) ) ;
#57451 = DIRECTION ( 'NONE',  ( -0.000000000000000000, -1.000000000000000000, -0.000000000000000000 ) ) ;
#57452 = ORIENTED_EDGE ( 'NONE', *, *, #40132, .F. ) ;
#57453 = ADVANCED_FACE ( 'NONE', ( #93133 ), #93768, .T. ) ;
#57454 = CONICAL_SURFACE ( 'NONE', #3080, 0.09999999999999982514, 0.003490658503988666988 ) ;
#57455 = ORIENTED_EDGE ( 'NONE', *, *, #74826, .T. ) ;
#57456 = VERTEX_POINT ( 'NONE', #112770 ) ;
#57457 = AXIS2_PLACEMENT_3D ( 'NONE', #75110, #16156, #115011 ) ;
#57458 = EDGE_CURVE ( 'NONE', #52047, #114100, #90482, .T. ) ;
#57459 = ORIENTED_EDGE ( 'NONE', *, *, #95088, .F. ) ;
#57460 = DIRECTION ( 'NONE',  ( -4.274815082592931898E-19, -0.9999939076577903929, -0.003490651415223739937 ) ) ;
#57462 = AXIS2_PLACEMENT_3D ( 'NONE', #45494, #15348, #94565 ) ;
#57461 = DIRECTION ( 'NONE',  ( 0.000000000000000000, -0.9999939076577903929, 0.003490651415223739937 ) ) ;
#57463 = VECTOR ( 'NONE', #75679, 1000.000000000000000 ) ;
#57464 = DIRECTION ( 'NONE',  ( 0.000000000000000000, 1.000000000000000000, 0.000000000000000000 ) ) ;
#57465 = FACE_BOUND ( 'NONE', #71512, .T. ) ;
#57466 = DIRECTION ( 'NONE',  ( -4.274815082592931898E-19, -0.9999939076577903929, -0.003490651415223739937 ) ) ;
#57467 = DIRECTION ( 'NONE',  ( 0.000000000000000000, -0.000000000000000000, 1.000000000000000000 ) ) ;
#57468 = CARTESIAN_POINT ( 'NONE',  ( 13.74999999999989697, 2.500000000000000000, 2.857883832488649301 ) ) ;
#57469 = DIRECTION ( 'NONE',  ( 0.000000000000000000, 1.000000000000000000, 0.000000000000000000 ) ) ;
#57470 = CONICAL_SURFACE ( 'NONE', #128596, 0.1000000000000002554, 0.003490658503988666988 ) ;
#57471 = AXIS2_PLACEMENT_3D ( 'NONE', #71331, #111245, #101458 ) ;
#57472 = AXIS2_PLACEMENT_3D ( 'NONE', #47414, #48058, #69616 ) ;
#57473 = CARTESIAN_POINT ( 'NONE',  ( 183.9635416670080872, -4.367472073101520635, 7.564683531249999149 ) ) ;
#57474 = CIRCLE ( 'NONE', #118096, 0.06509327318403745899 ) ;
#57475 = DIRECTION ( 'NONE',  ( -0.000000000000000000, -1.000000000000000000, -0.000000000000000000 ) ) ;
#57476 = FACE_OUTER_BOUND ( 'NONE', #12937, .T. ) ;
#57477 = AXIS2_PLACEMENT_3D ( 'NONE', #78987, #27932, #47585 ) ;
#57478 = AXIS2_PLACEMENT_3D ( 'NONE', #123969, #42877, #44131 ) ;
#57479 = DIRECTION ( 'NONE',  ( -0.000000000000000000, -1.000000000000000000, -0.000000000000000000 ) ) ;
#57480 = ORIENTED_EDGE ( 'NONE', *, *, #7505, .F. ) ;
#57481 = ORIENTED_EDGE ( 'NONE', *, *, #44276, .T. ) ;
#57482 = VERTEX_POINT ( 'NONE', #24382 ) ;
#57483 = EDGE_LOOP ( 'NONE', ( #123594, #12009 ) ) ;
#57484 = CIRCLE ( 'NONE', #55424, 1.388921157871087386 ) ;
#57485 = DIRECTION ( 'NONE',  ( 0.000000000000000000, 1.000000000000000000, 0.000000000000000000 ) ) ;
#57486 = FACE_BOUND ( 'NONE', #123012, .T. ) ;
#57487 = CARTESIAN_POINT ( 'NONE',  ( -6.700000000000019718, 12.50000000000000000, -2.385244779468109755E-15 ) ) ;
#57488 = DIRECTION ( 'NONE',  ( 0.000000000000000000, 0.000000000000000000, -1.000000000000000000 ) ) ;
#57489 = ORIENTED_EDGE ( 'NONE', *, *, #10574, .T. ) ;
#57490 = CARTESIAN_POINT ( 'NONE',  ( -8.550000000000007816, 2.500000000000000000, 6.048780366869520364 ) ) ;
#57491 = DIRECTION ( 'NONE',  ( -0.000000000000000000, 1.000000000000000000, -0.000000000000000000 ) ) ;
#57492 = DIRECTION ( 'NONE',  ( 0.000000000000000000, 1.000000000000000000, 0.000000000000000000 ) ) ;
#57494 = ORIENTED_EDGE ( 'NONE', *, *, #104305, .F. ) ;
#57493 = AXIS2_PLACEMENT_3D ( 'NONE', #30946, #108829, #19148 ) ;
#57495 = CARTESIAN_POINT ( 'NONE',  ( 10.64999999999990976, 12.50000000000000000, 2.576566944158910744 ) ) ;
#57496 = CARTESIAN_POINT ( 'NONE',  ( -12.49999999999999289, 2.500000000000000000, -0.6928203230275500335 ) ) ;
#57497 = EDGE_CURVE ( 'NONE', #44808, #93899, #44670, .T. ) ;
#57498 = PRODUCT ( 'Waterproof Outer Handle Shell', 'Waterproof Outer Handle Shell', '', ( #88257 ) ) ;
#57499 = MANIFOLD_SOLID_BREP ( 'Cut-Extrude-Thin1', #79159 ) ;
#57500 = EDGE_LOOP ( 'NONE', ( #36276, #89612, #10431, #101732 ) ) ;
#57501 = LINE ( 'NONE', #126236, #27817 ) ;
#57502 = DIRECTION ( 'NONE',  ( 0.000000000000000000, -0.000000000000000000, 1.000000000000000000 ) ) ;
#57503 = CIRCLE ( 'NONE', #90952, 0.06509327318403745899 ) ;
#57504 = CIRCLE ( 'NONE', #28258, 0.09999999999999982514 ) ;
#57505 = ORIENTED_EDGE ( 'NONE', *, *, #80339, .T. ) ;
#57506 = DIRECTION ( 'NONE',  ( -0.000000000000000000, 1.000000000000000000, -0.000000000000000000 ) ) ;
#57507 = CARTESIAN_POINT ( 'NONE',  ( -8.350000000000008527, 12.50000000000000000, 7.188010851410848723 ) ) ;
#57508 = VERTEX_POINT ( 'NONE', #95062 ) ;
#57509 = DIRECTION ( 'NONE',  ( -4.274815082592931898E-19, -0.9999939076577903929, -0.003490651415223739937 ) ) ;
#57510 = ORIENTED_EDGE ( 'NONE', *, *, #127819, .T. ) ;
#57511 = EDGE_CURVE ( 'NONE', #46085, #11888, #46575, .T. ) ;
#57512 = ORIENTED_EDGE ( 'NONE', *, *, #60044, .T. ) ;
#57513 = ADVANCED_FACE ( 'NONE', ( #4709 ), #34867, .T. ) ;
#57514 = DIRECTION ( 'NONE',  ( -0.000000000000000000, -1.000000000000000000, -0.000000000000000000 ) ) ;
#57515 = ORIENTED_EDGE ( 'NONE', *, *, #106421, .T. ) ;
#57516 = FACE_OUTER_BOUND ( 'NONE', #29565, .T. ) ;
#57517 = FACE_BOUND ( 'NONE', #126167, .T. ) ;
#57518 = AXIS2_PLACEMENT_3D ( 'NONE', #49252, #119252, #51182 ) ;
#57519 = VERTEX_POINT ( 'NONE', #83315 ) ;
#57521 = CARTESIAN_POINT ( 'NONE',  ( 110.2425064135121744, 6.264065668498300710, -4.480648340451071299 ) ) ;
#57520 = AXIS2_PLACEMENT_3D ( 'NONE', #18197, #37843, #49622 ) ;
#57522 = VERTEX_POINT ( 'NONE', #33568 ) ;
#57523 = LINE ( 'NONE', #16273, #100564 ) ;
#57524 = PLANE ( 'NONE',  #90425 ) ;
#57525 = FACE_OUTER_BOUND ( 'NONE', #74535, .T. ) ;
#57527 = EDGE_CURVE ( 'NONE', #26026, #81857, #73759, .T. ) ;
#57526 = DIRECTION ( 'NONE',  ( -0.000000000000000000, 1.000000000000000000, -0.000000000000000000 ) ) ;
#57528 = CARTESIAN_POINT ( 'NONE',  ( -3.550000000000028244, 12.50000000000000000, 2.511473670974873507 ) ) ;
#57529 = ORIENTED_EDGE ( 'NONE', *, *, #5098, .F. ) ;
#57530 = VERTEX_POINT ( 'NONE', #10377 ) ;
#57531 = CARTESIAN_POINT ( 'NONE',  ( 4.599999999999938360, 12.50000000000000000, -2.276824562219559311E-15 ) ) ;
#57532 = CONICAL_SURFACE ( 'NONE', #84708, 0.1000000000000002554, 0.003490658503988666988 ) ;
#57533 = DIRECTION ( 'NONE',  ( 0.000000000000000000, 0.000000000000000000, -1.000000000000000000 ) ) ;
#57534 = CARTESIAN_POINT ( 'NONE',  ( 5.199999999999935341, 2.500000000000000000, -3.983716857408426293 ) ) ;
#57536 = VERTEX_POINT ( 'NONE', #30684 ) ;
#57535 = ORIENTED_EDGE ( 'NONE', *, *, #105946, .T. ) ;
#57537 = ORIENTED_EDGE ( 'NONE', *, *, #18951, .F. ) ;
#57538 = DIRECTION ( 'NONE',  ( 0.000000000000000000, 1.000000000000000000, 0.000000000000000000 ) ) ;
#57539 = DIRECTION ( 'NONE',  ( 0.000000000000000000, 1.000000000000000000, 0.000000000000000000 ) ) ;
#57540 = DIRECTION ( 'NONE',  ( 0.000000000000000000, -0.9999939076577903929, 0.003490651415223739937 ) ) ;
#57541 = DIRECTION ( 'NONE',  ( 0.000000000000000000, 0.000000000000000000, 1.000000000000000000 ) ) ;
#57542 = FACE_OUTER_BOUND ( 'NONE', #98511, .T. ) ;
#57543 = DIRECTION ( 'NONE',  ( -0.000000000000000000, -1.000000000000000000, -0.000000000000000000 ) ) ;
#57544 = DIRECTION ( 'NONE',  ( 0.000000000000000000, 0.000000000000000000, 1.000000000000000000 ) ) ;
#57545 = DIRECTION ( 'NONE',  ( -0.000000000000000000, -1.000000000000000000, -0.000000000000000000 ) ) ;
#57546 = CONICAL_SURFACE ( 'NONE', #28298, 0.1000000000000002554, 0.003490658503988666988 ) ;
#57547 = DIRECTION ( 'NONE',  ( 0.000000000000000000, 1.000000000000000000, 0.000000000000000000 ) ) ;
#57548 = EDGE_LOOP ( 'NONE', ( #33922, #54819, #26933, #51459 ) ) ;
#57549 = ORIENTED_EDGE ( 'NONE', *, *, #82126, .T. ) ;
#57550 = EDGE_CURVE ( 'NONE', #45421, #92599, #113474, .T. ) ;
#57551 = AXIS2_PLACEMENT_3D ( 'NONE', #59934, #12091, #10170 ) ;
#57552 = VECTOR ( 'NONE', #74957, 1000.000000000000000 ) ;
#57553 = DIRECTION ( 'NONE',  ( -0.000000000000000000, -1.000000000000000000, -0.000000000000000000 ) ) ;
#57554 = CIRCLE ( 'NONE', #3178, 0.06509327318403745899 ) ;
#57555 = EDGE_LOOP ( 'NONE', ( #96576, #93504, #42002, #47399 ) ) ;
#57556 = ORIENTED_EDGE ( 'NONE', *, *, #44828, .F. ) ;
#57557 = EDGE_CURVE ( 'NONE', #42124, #46460, #57033, .T. ) ;
#57558 = DIRECTION ( 'NONE',  ( 0.000000000000000000, 0.000000000000000000, 1.000000000000000000 ) ) ;
#57559 = CARTESIAN_POINT ( 'NONE',  ( 2.299999999999946976, 2.500000000000000000, 4.676537180435972552 ) ) ;
#57560 = DIRECTION ( 'NONE',  ( -4.274815082592931898E-19, -0.9999939076577903929, -0.003490651415223739937 ) ) ;
#57561 = EDGE_CURVE ( 'NONE', #18141, #26625, #107217, .T. ) ;
#57562 = CONICAL_SURFACE ( 'NONE', #55498, 0.1000000000000002554, 0.003490658503988666988 ) ;
#57563 = DIRECTION ( 'NONE',  ( 0.000000000000000000, 0.000000000000000000, 1.000000000000000000 ) ) ;
#57564 = CIRCLE ( 'NONE', #124453, 0.06509327318403745899 ) ;
#57566 = CARTESIAN_POINT ( 'NONE',  ( 2.899999999999943956, 2.500000000000000000, 4.330127018922196314 ) ) ;
#57565 = CIRCLE ( 'NONE', #74287, 5.000000000000000000 ) ;
#57567 = CARTESIAN_POINT ( 'NONE',  ( -1.450000000000036371, 2.500000000000000000, 2.511473670974873507 ) ) ;
#57568 = DIRECTION ( 'NONE',  ( 0.000000000000000000, 0.000000000000000000, -1.000000000000000000 ) ) ;
#57569 = ORIENTED_EDGE ( 'NONE', *, *, #109997, .F. ) ;
#57570 = DIRECTION ( 'NONE',  ( 0.000000000000000000, 0.000000000000000000, 1.000000000000000000 ) ) ;
#57571 = ADVANCED_FACE ( 'NONE', ( #30035 ), #50307, .T. ) ;
#57572 = CIRCLE ( 'NONE', #1114, 0.09999999999999999167 ) ;
#57573 = EDGE_CURVE ( 'NONE', #97417, #56205, #40509, .T. ) ;
#57574 = EDGE_CURVE ( 'NONE', #19384, #99701, #120338, .T. ) ;
#57575 = EDGE_CURVE ( 'NONE', #115572, #120080, #118391, .T. ) ;
#57576 = CARTESIAN_POINT ( 'NONE',  ( -12.89999999999999147, 12.50000000000000000, 5.088040615133786027 ) ) ;
#57577 = AXIS2_PLACEMENT_3D ( 'NONE', #14717, #35676, #124045 ) ;
#57578 = CIRCLE ( 'NONE', #84754, 0.06509327318403745899 ) ;
#57579 = ORIENTED_EDGE ( 'NONE', *, *, #27853, .T. ) ;
#57580 = EDGE_CURVE ( 'NONE', #88147, #102605, #50794, .T. ) ;
#57581 = ORIENTED_EDGE ( 'NONE', *, *, #118544, .F. ) ;
#57582 = AXIS2_PLACEMENT_3D ( 'NONE', #34247, #104877, #34891 ) ;
#57583 = ORIENTED_EDGE ( 'NONE', *, *, #87990, .F. ) ;
#57584 = VERTEX_POINT ( 'NONE', #69278 ) ;
#57585 = DIRECTION ( 'NONE',  ( 0.000000000000000000, 1.000000000000000000, 0.000000000000000000 ) ) ;
#57586 = DIRECTION ( 'NONE',  ( -0.000000000000000000, 1.000000000000000000, -0.000000000000000000 ) ) ;
#57587 = EDGE_CURVE ( 'NONE', #17997, #81742, #32029, .T. ) ;
#57588 = ORIENTED_EDGE ( 'NONE', *, *, #105380, .F. ) ;
#57589 = CARTESIAN_POINT ( 'NONE',  ( -10.60000000000000142, 12.50000000000000000, -0.4115034346978156399 ) ) ;
#57590 = CARTESIAN_POINT ( 'NONE',  ( 17.50000000000000000, -2.750000000000000000, -9.999999999999998224 ) ) ;
#57591 = DIRECTION ( 'NONE',  ( -0.000000000000000000, -1.000000000000000000, -0.000000000000000000 ) ) ;
#57592 = ORIENTED_EDGE ( 'NONE', *, *, #119762, .T. ) ;
#57593 = DIRECTION ( 'NONE',  ( 0.000000000000000000, 1.000000000000000000, 0.000000000000000000 ) ) ;
#57594 = AXIS2_PLACEMENT_3D ( 'NONE', #101612, #83261, #4654 ) ;
#57595 = CARTESIAN_POINT ( 'NONE',  ( -13.74999999999995381, 2.500000000000000000, -2.265063509461099578 ) ) ;
#57596 = EDGE_LOOP ( 'NONE', ( #39827, #6277 ) ) ;
#57597 = VERTEX_POINT ( 'NONE', #109207 ) ;
#57598 = EDGE_LOOP ( 'NONE', ( #44855, #1990 ) ) ;
#57599 = DIRECTION ( 'NONE',  ( 0.000000000000000000, 1.000000000000000000, 0.000000000000000000 ) ) ;
#57600 = CONICAL_SURFACE ( 'NONE', #9470, 0.09999999999999982514, 0.003490658503988666988 ) ;
#57601 = AXIS2_PLACEMENT_3D ( 'NONE', #78116, #117349, #38189 ) ;
#57602 = DIRECTION ( 'NONE',  ( 0.000000000000000000, -0.000000000000000000, 1.000000000000000000 ) ) ;
#57603 = CONICAL_SURFACE ( 'NONE', #99368, 0.09999999999999982514, 0.003490658503988666988 ) ;
#57604 = EDGE_LOOP ( 'NONE', ( #65261, #82338, #99304, #22774 ) ) ;
#57605 = CARTESIAN_POINT ( 'NONE',  ( 186.0312500006828031, 9.429780353434619030E-16, -7.700000000000000178 ) ) ;
#57606 = CARTESIAN_POINT ( 'NONE',  ( -15.79999999999998117, 2.500000000000000000, -0.1000000000000000056 ) ) ;
#57607 = CARTESIAN_POINT ( 'NONE',  ( 105.5000000000000142, 0.000000000000000000, 2.000000000000000000 ) ) ;
#57608 = DIRECTION ( 'NONE',  ( 0.000000000000000000, 1.000000000000000000, 0.000000000000000000 ) ) ;
#57609 = AXIS2_PLACEMENT_3D ( 'NONE', #39297, #107992, #118454 ) ;
#57610 = EDGE_LOOP ( 'NONE', ( #72832, #83902 ) ) ;
#57611 = CARTESIAN_POINT ( 'NONE',  ( 0.1999999999999627909, 2.500000000000000000, 0.4464101615137758272 ) ) ;
#57612 = EDGE_CURVE ( 'NONE', #15438, #48671, #542, .T. ) ;
#57613 = VECTOR ( 'NONE', #32567, 1000.000000000000000 ) ;
#57614 = ORIENTED_EDGE ( 'NONE', *, *, #103539, .F. ) ;
#57615 = ORIENTED_EDGE ( 'NONE', *, *, #25914, .T. ) ;
#57616 = CARTESIAN_POINT ( 'NONE',  ( -10.80000000000000249, 2.500000000000000000, -4.230127018922197557 ) ) ;
#57617 = DIRECTION ( 'NONE',  ( 0.000000000000000000, 1.000000000000000000, 0.000000000000000000 ) ) ;
#57618 = FACE_BOUND ( 'NONE', #126576, .T. ) ;
#57619 = DIRECTION ( 'NONE',  ( 0.000000000000000000, -0.9999939076577903929, 0.003490651415223739937 ) ) ;
#57620 = CYLINDRICAL_SURFACE ( 'NONE', #8828, 5.000000000000000000 ) ;
#57621 = CARTESIAN_POINT ( 'NONE',  ( 3.949999999999940670, 12.50000000000000000, 1.818653347947321475 ) ) ;
#57622 = EDGE_CURVE ( 'NONE', #103182, #36921, #70588, .T. ) ;
#57623 = AXIS2_PLACEMENT_3D ( 'NONE', #34955, #66950, #35591 ) ;
#57624 = AXIS2_PLACEMENT_3D ( 'NONE', #106906, #99691, #18536 ) ;
#57625 = ORIENTED_EDGE ( 'NONE', *, *, #90949, .F. ) ;
#57626 = DIRECTION ( 'NONE',  ( 0.000000000000000000, 0.000000000000000000, 1.000000000000000000 ) ) ;
#57627 = DIRECTION ( 'NONE',  ( 0.000000000000000000, 0.000000000000000000, 1.000000000000000000 ) ) ;
#57628 = CARTESIAN_POINT ( 'NONE',  ( 9.349999999999919709, 12.50000000000000000, -6.841600689897078702 ) ) ;
#57629 = DIRECTION ( 'NONE',  ( 0.000000000000000000, -0.000000000000000000, -1.000000000000000000 ) ) ;
#57630 = ORIENTED_EDGE ( 'NONE', *, *, #39381, .T. ) ;
#57631 = CARTESIAN_POINT ( 'NONE',  ( -3.350000000000028511, 2.500000000000000000, 2.857883832488649301 ) ) ;
#57632 = FACE_OUTER_BOUND ( 'NONE', #75578, .T. ) ;
#57633 = ORIENTED_EDGE ( 'NONE', *, *, #76588, .F. ) ;
#57634 = ORIENTED_EDGE ( 'NONE', *, *, #39582, .F. ) ;
#57635 = DIRECTION ( 'NONE',  ( 0.000000000000000000, -0.000000000000000000, 1.000000000000000000 ) ) ;
#57636 = CARTESIAN_POINT ( 'NONE',  ( 13.94999999999989271, 2.500000000000000000, -1.818653347947326138 ) ) ;
#57637 = VECTOR ( 'NONE', #31958, 1000.000000000000000 ) ;
#57638 = FACE_BOUND ( 'NONE', #51299, .T. ) ;
#57639 = CARTESIAN_POINT ( 'NONE',  ( -4.550000000000022915, 12.50000000000000000, -2.230156782645139391 ) ) ;
#57640 = CIRCLE ( 'NONE', #38893, 0.1000000000000002554 ) ;
#57641 = EDGE_LOOP ( 'NONE', ( #8917, #50694, #115690, #45636 ) ) ;
#57642 = DIRECTION ( 'NONE',  ( 0.000000000000000000, 1.000000000000000000, 0.000000000000000000 ) ) ;
#57643 = AXIS2_PLACEMENT_3D ( 'NONE', #111493, #101688, #120683 ) ;
#57644 = ORIENTED_EDGE ( 'NONE', *, *, #13874, .T. ) ;
#57645 = ORIENTED_EDGE ( 'NONE', *, *, #61562, .F. ) ;
#57646 = DIRECTION ( 'NONE',  ( -4.274815082592931898E-19, -0.9999939076577903929, -0.003490651415223739937 ) ) ;
#57647 = CARTESIAN_POINT ( 'NONE',  ( 184.3385416670080872, 6.551208109652274736, 3.782341765625001351 ) ) ;
#57648 = ORIENTED_EDGE ( 'NONE', *, *, #73601, .F. ) ;
#57649 = DIRECTION ( 'NONE',  ( 0.000000000000000000, 0.000000000000000000, 1.000000000000000000 ) ) ;
#57650 = DIRECTION ( 'NONE',  ( 0.000000000000000000, -0.9999939076577903929, 0.003490651415223739937 ) ) ;
#57651 = AXIS2_PLACEMENT_3D ( 'NONE', #115153, #73318, #62237 ) ;
#57652 = ADVANCED_FACE ( 'NONE', ( #128237 ), #6010, .T. ) ;
#57653 = CIRCLE ( 'NONE', #89042, 0.1000000000000000056 ) ;
#57654 = DIRECTION ( 'NONE',  ( 0.000000000000000000, 0.000000000000000000, 1.000000000000000000 ) ) ;
#57655 = DIRECTION ( 'NONE',  ( 0.000000000000000000, 1.000000000000000000, 0.000000000000000000 ) ) ;
#57656 = AXIS2_PLACEMENT_3D ( 'NONE', #116793, #127917, #78184 ) ;
#57658 = ADVANCED_FACE ( 'NONE', ( #98742 ), #25645, .T. ) ;
#57657 = CIRCLE ( 'NONE', #107546, 0.1000000000000000472 ) ;
#57659 = ORIENTED_EDGE ( 'NONE', *, *, #105051, .T. ) ;
#57660 = AXIS2_PLACEMENT_3D ( 'NONE', #100988, #110803, #9397 ) ;
#57661 = CARTESIAN_POINT ( 'NONE',  ( -3.750000000000026201, 2.500000000000000000, 5.902370205355745192 ) ) ;
#57662 = CARTESIAN_POINT ( 'NONE',  ( 11.04999999999990834, 2.500000000000000000, -6.841600689897077814 ) ) ;
#57663 = AXIS2_PLACEMENT_3D ( 'NONE', #112637, #30224, #62254 ) ;
#57664 = DIRECTION ( 'NONE',  ( 0.000000000000000000, 0.000000000000000000, -1.000000000000000000 ) ) ;
#57665 = EDGE_LOOP ( 'NONE', ( #109635, #83328 ) ) ;
#57666 = ADVANCED_FACE ( 'NONE', ( #127575 ), #42389, .T. ) ;
#57667 = CARTESIAN_POINT ( 'NONE',  ( -5.200000000000020606, 2.500000000000000000, -0.3464101615137782364 ) ) ;
#57668 = ORIENTED_EDGE ( 'NONE', *, *, #18972, .T. ) ;
#57669 = ADVANCED_FACE ( 'NONE', ( #77816 ), #107929, .T. ) ;
#57670 = DIRECTION ( 'NONE',  ( 0.000000000000000000, -0.000000000000000000, 1.000000000000000000 ) ) ;
#57671 = ORIENTED_EDGE ( 'NONE', *, *, #12725, .F. ) ;
#57672 = FACE_OUTER_BOUND ( 'NONE', #3239, .T. ) ;
#57673 = CARTESIAN_POINT ( 'NONE',  ( 17.50000000000000000, -2.499999999999999556, 3.333333333333336146 ) ) ;
#57674 = CARTESIAN_POINT ( 'NONE',  ( -0.2000000000000404232, 2.500000000000000000, 3.983716857408420964 ) ) ;
#57675 = CARTESIAN_POINT ( 'NONE',  ( -0.8500000000000386136, 2.500000000000000000, 1.472243186433545459 ) ) ;
#57676 = ORIENTED_EDGE ( 'NONE', *, *, #6553, .T. ) ;
#57677 = EDGE_CURVE ( 'NONE', #27768, #5489, #123931, .T. ) ;
#57678 = CARTESIAN_POINT ( 'NONE',  ( 11.04999999999991189, 2.500000000000000000, -2.511473670974877948 ) ) ;
#57679 = CARTESIAN_POINT ( 'NONE',  ( 12.69999999999990159, 12.50000000000000000, 4.741630453620009789 ) ) ;
#57680 = CARTESIAN_POINT ( 'NONE',  ( 184.5138397154228187, -7.190708303082583797, -2.674694939153578588 ) ) ;
#57681 = LINE ( 'NONE', #78622, #27614 ) ;
#57682 = ADVANCED_FACE ( 'NONE', ( #48368 ), #44524, .T. ) ;
#57683 = AXIS2_PLACEMENT_3D ( 'NONE', #124311, #17562, #34664 ) ;
#57684 = DIRECTION ( 'NONE',  ( 1.000000000000000000, 0.000000000000000000, -0.000000000000000000 ) ) ;
#57685 = ORIENTED_EDGE ( 'NONE', *, *, #10603, .F. ) ;
#57686 = ORIENTED_EDGE ( 'NONE', *, *, #44828, .T. ) ;
#57687 = DIRECTION ( 'NONE',  ( 0.000000000000000000, 0.000000000000000000, -1.000000000000000000 ) ) ;
#57688 = ORIENTED_EDGE ( 'NONE', *, *, #126289, .T. ) ;
#57689 = CARTESIAN_POINT ( 'NONE',  ( 3.149999999999946176, 2.500000000000000000, -1.718653347947325827 ) ) ;
#57691 = VERTEX_POINT ( 'NONE', #92819 ) ;
#57690 = ORIENTED_EDGE ( 'NONE', *, *, #55918, .T. ) ;
#57692 = CIRCLE ( 'NONE', #80675, 0.09999999999999982514 ) ;
#57693 = ORIENTED_EDGE ( 'NONE', *, *, #2418, .F. ) ;
#57694 = DIRECTION ( 'NONE',  ( 0.000000000000000000, 0.000000000000000000, 1.000000000000000000 ) ) ;
#57695 = AXIS2_PLACEMENT_3D ( 'NONE', #69541, #78752, #8041 ) ;
#57696 = CONICAL_SURFACE ( 'NONE', #118318, 0.1000000000000000056, 0.003490658503988666988 ) ;
#57697 = DIRECTION ( 'NONE',  ( 0.000000000000000000, 1.000000000000000000, 0.000000000000000000 ) ) ;
#57698 = LINE ( 'NONE', #30178, #99910 ) ;
#57699 = CIRCLE ( 'NONE', #84871, 0.06509327318403745899 ) ;
#57700 =( LENGTH_UNIT ( ) NAMED_UNIT ( * ) SI_UNIT ( .MILLI., .METRE. ) );
#57701 = CARTESIAN_POINT ( 'NONE',  ( 7.499999999999923617, 2.500000000000000000, 0.5928203230275495006 ) ) ;
#57702 = CARTESIAN_POINT ( 'NONE',  ( 3.549999999999940314, 12.50000000000000000, 6.841600689897072485 ) ) ;
#57703 = DIRECTION ( 'NONE',  ( 0.000000000000000000, 1.000000000000000000, 0.000000000000000000 ) ) ;
#57704 = DIRECTION ( 'NONE',  ( 0.000000000000000000, -0.9999939076577903929, 0.003490651415223739937 ) ) ;
#57705 = ORIENTED_EDGE ( 'NONE', *, *, #75077, .T. ) ;
#57706 = DIRECTION ( 'NONE',  ( 0.000000000000000000, 0.000000000000000000, 1.000000000000000000 ) ) ;
#57707 = ORIENTED_EDGE ( 'NONE', *, *, #30435, .F. ) ;
#57708 = VECTOR ( 'NONE', #124272, 1000.000000000000000 ) ;
#57709 = EDGE_LOOP ( 'NONE', ( #16392, #99441, #63774, #119075 ) ) ;
#57710 = ORIENTED_EDGE ( 'NONE', *, *, #105582, .F. ) ;
#57711 = EDGE_LOOP ( 'NONE', ( #23239, #12223, #82674, #118300 ) ) ;
#57713 = VECTOR ( 'NONE', #75046, 1000.000000000000000 ) ;
#57712 = VECTOR ( 'NONE', #13059, 1000.000000000000000 ) ;
#57714 = DIRECTION ( 'NONE',  ( 0.000000000000000000, 0.000000000000000000, -1.000000000000000000 ) ) ;
#57715 = ORIENTED_EDGE ( 'NONE', *, *, #64887, .T. ) ;
#57716 = ORIENTED_EDGE ( 'NONE', *, *, #78799, .T. ) ;
#57717 = EDGE_CURVE ( 'NONE', #75979, #105778, #3780, .T. ) ;
#57718 = DIRECTION ( 'NONE',  ( 0.000000000000000000, 0.000000000000000000, 1.000000000000000000 ) ) ;
#57719 = FACE_OUTER_BOUND ( 'NONE', #121775, .T. ) ;
#57720 = CIRCLE ( 'NONE', #1272, 0.06509327318403745899 ) ;
#57721 = CARTESIAN_POINT ( 'NONE',  ( 4.799999999999939426, 2.500000000000000000, -4.676537180435977881 ) ) ;
#57722 = DIRECTION ( 'NONE',  ( 0.000000000000000000, 0.000000000000000000, 1.000000000000000000 ) ) ;
#57723 = EDGE_CURVE ( 'NONE', #53300, #1004, #77974, .T. ) ;
#57724 = CARTESIAN_POINT ( 'NONE',  ( -4.550000000000026468, 2.500000000000000000, -6.595190528383302109 ) ) ;
#57725 = EDGE_LOOP ( 'NONE', ( #16606, #118016 ) ) ;
#57726 = ADVANCED_FACE ( 'NONE', ( #43090 ), #8913, .T. ) ;
#57727 = EDGE_CURVE ( 'NONE', #4806, #24998, #121607, .T. ) ;
#57728 = CARTESIAN_POINT ( 'NONE',  ( -1.050000000000038680, 12.50000000000000000, 2.511473670974873507 ) ) ;
#57729 = EDGE_CURVE ( 'NONE', #107800, #48300, #100954, .T. ) ;
#57730 = ORIENTED_EDGE ( 'NONE', *, *, #107661, .T. ) ;
#57731 = FACE_OUTER_BOUND ( 'NONE', #127079, .T. ) ;
#57732 = ORIENTED_EDGE ( 'NONE', *, *, #87960, .F. ) ;
#57733 = LINE ( 'NONE', #17783, #67157 ) ;
#57734 = ADVANCED_FACE ( 'NONE', ( #81689 ), #1837, .T. ) ;
#57735 = EDGE_LOOP ( 'NONE', ( #87726, #50526 ) ) ;
#57736 = ORIENTED_EDGE ( 'NONE', *, *, #53436, .F. ) ;
#57737 = DIRECTION ( 'NONE',  ( 0.000000000000000000, -0.9999939076577903929, 0.003490651415223739937 ) ) ;
#57738 = CARTESIAN_POINT ( 'NONE',  ( 3.349999999999941025, 12.50000000000000000, 7.122917578226811486 ) ) ;
#57739 = EDGE_CURVE ( 'NONE', #85338, #116689, #117755, .T. ) ;
#57740 = EDGE_CURVE ( 'NONE', #112785, #67757, #63346, .T. ) ;
#57741 = CARTESIAN_POINT ( 'NONE',  ( 186.0833333333333144, -6.668395609140180369, 3.849999999999994760 ) ) ;
#57743 = DIRECTION ( 'NONE',  ( 0.000000000000000000, -0.000000000000000000, 1.000000000000000000 ) ) ;
#57742 = CIRCLE ( 'NONE', #9607, 0.06509327318403745899 ) ;
#57744 = LINE ( 'NONE', #117261, #34513 ) ;
#57745 = EDGE_LOOP ( 'NONE', ( #128280, #119178 ) ) ;
#57746 = CARTESIAN_POINT ( 'NONE',  ( 10.59999999999990905, 2.500000000000000000, -4.776537180435978414 ) ) ;
#57747 = LINE ( 'NONE', #125810, #86985 ) ;
#57748 = CARTESIAN_POINT ( 'NONE',  ( 3.149999999999946176, 2.500000000000000000, -1.818653347947325916 ) ) ;
#57749 = DIRECTION ( 'NONE',  ( 0.000000000000000000, 0.000000000000000000, 1.000000000000000000 ) ) ;
#57751 = AXIS2_PLACEMENT_3D ( 'NONE', #42348, #50240, #90127 ) ;
#57750 = CIRCLE ( 'NONE', #99792, 0.06509327318403745899 ) ;
#57752 = DIRECTION ( 'NONE',  ( 0.000000000000000000, 1.000000000000000000, 0.000000000000000000 ) ) ;
#57753 = ORIENTED_EDGE ( 'NONE', *, *, #121427, .T. ) ;
#57754 = VERTEX_POINT ( 'NONE', #110510 ) ;
#57755 = DIRECTION ( 'NONE',  ( -0.000000000000000000, 1.000000000000000000, -0.000000000000000000 ) ) ;
#57756 = VERTEX_POINT ( 'NONE', #102613 ) ;
#57758 = CONICAL_SURFACE ( 'NONE', #26457, 0.09999999999999999167, 0.003490658503988666988 ) ;
#57757 = AXIS2_PLACEMENT_3D ( 'NONE', #65614, #17795, #28278 ) ;
#57759 = CARTESIAN_POINT ( 'NONE',  ( 12.69999999999989981, 2.500000000000000000, -0.3464101615137783474 ) ) ;
#57760 = DIRECTION ( 'NONE',  ( -0.000000000000000000, 1.000000000000000000, -0.000000000000000000 ) ) ;
#57761 = AXIS2_PLACEMENT_3D ( 'NONE', #3431, #82654, #72826 ) ;
#57762 = VERTEX_POINT ( 'NONE', #111812 ) ;
#57763 = CARTESIAN_POINT ( 'NONE',  ( 186.4583333333333144, 4.445597072760117285, 7.699999999999999289 ) ) ;
#57764 = CARTESIAN_POINT ( 'NONE',  ( 0.8499999999999536815, 12.50000000000000000, 6.560283801567334372 ) ) ;
#57765 = CARTESIAN_POINT ( 'NONE',  ( -10.20000000000000462, 2.500000000000000000, 4.676537180435972552 ) ) ;
#57766 = PLANE ( 'NONE',  #60172 ) ;
#57767 = ORIENTED_EDGE ( 'NONE', *, *, #54538, .T. ) ;
#57768 = CARTESIAN_POINT ( 'NONE',  ( -1.450000000000036371, 12.50000000000000000, 2.446380397790835826 ) ) ;
#57769 = DIRECTION ( 'NONE',  ( 0.000000000000000000, 1.000000000000000000, 0.000000000000000000 ) ) ;
#57770 = ORIENTED_EDGE ( 'NONE', *, *, #13825, .T. ) ;
#57771 = DIRECTION ( 'NONE',  ( -0.000000000000000000, -1.000000000000000000, -0.000000000000000000 ) ) ;
#57772 = AXIS2_PLACEMENT_3D ( 'NONE', #2426, #33219, #101943 ) ;
#57773 = LINE ( 'NONE', #6689, #68520 ) ;
#57774 = FACE_OUTER_BOUND ( 'NONE', #25903, .T. ) ;
#57775 = EDGE_CURVE ( 'NONE', #3528, #47378, #71224, .T. ) ;
#57776 = ORIENTED_EDGE ( 'NONE', *, *, #117775, .T. ) ;
#57777 = CIRCLE ( 'NONE', #103746, 0.06509327318403745899 ) ;
#57778 = DIRECTION ( 'NONE',  ( 0.000000000000000000, 0.000000000000000000, -1.000000000000000000 ) ) ;
#57779 = AXIS2_PLACEMENT_3D ( 'NONE', #118351, #28701, #48995 ) ;
#57780 = ORIENTED_EDGE ( 'NONE', *, *, #39476, .T. ) ;
#57781 = CARTESIAN_POINT ( 'NONE',  ( 12.09999999999990195, 2.500000000000000000, -0.6928203230275541413 ) ) ;
#57782 = CARTESIAN_POINT ( 'NONE',  ( -5.200000000000020606, 2.500000000000000000, 4.083716857408421497 ) ) ;
#57783 = DIRECTION ( 'NONE',  ( 0.000000000000000000, 1.000000000000000000, 0.000000000000000000 ) ) ;
#57784 = CONICAL_SURFACE ( 'NONE', #1334, 0.1000000000000002554, 0.003490658503988666988 ) ;
#57785 = ORIENTED_EDGE ( 'NONE', *, *, #125232, .T. ) ;
#57786 = DIRECTION ( 'NONE',  ( -4.274815082592931898E-19, -0.9999939076577903929, -0.003490651415223739937 ) ) ;
#57787 = CONICAL_SURFACE ( 'NONE', #128912, 0.1000000000000000472, 0.003490658503988666988 ) ;
#57788 = DIRECTION ( 'NONE',  ( 0.000000000000000000, 0.000000000000000000, -1.000000000000000000 ) ) ;
#57789 = VERTEX_POINT ( 'NONE', #22155 ) ;
#57790 = FACE_OUTER_BOUND ( 'NONE', #114409, .T. ) ;
#57791 = ORIENTED_EDGE ( 'NONE', *, *, #111451, .T. ) ;
#57793 = CIRCLE ( 'NONE', #47427, 0.09999999999999982514 ) ;
#57792 = CARTESIAN_POINT ( 'NONE',  ( 14.14999999999989377, 12.50000000000000000, -1.407149913249512663 ) ) ;
#57795 = CIRCLE ( 'NONE', #16007, 0.06509327318403743123 ) ;
#57794 = AXIS2_PLACEMENT_3D ( 'NONE', #79741, #80400, #88924 ) ;
#57796 = ORIENTED_EDGE ( 'NONE', *, *, #100243, .F. ) ;
#57797 = FACE_OUTER_BOUND ( 'NONE', #11758, .T. ) ;
#57798 = PLANE ( 'NONE',  #112769 ) ;
#57799 = VERTEX_POINT ( 'NONE', #50964 ) ;
#57800 = ORIENTED_EDGE ( 'NONE', *, *, #70827, .F. ) ;
#57801 = CARTESIAN_POINT ( 'NONE',  ( 11.89999999999990798, 12.50000000000000000, -4.676537180435977881 ) ) ;
#57802 = LINE ( 'NONE', #97711, #25465 ) ;
#57803 = ORIENTED_EDGE ( 'NONE', *, *, #52766, .F. ) ;
#57804 = DIRECTION ( 'NONE',  ( -0.000000000000000000, -1.000000000000000000, -0.000000000000000000 ) ) ;
#57805 = DIRECTION ( 'NONE',  ( 0.000000000000000000, 1.000000000000000000, 0.000000000000000000 ) ) ;
#57806 = CARTESIAN_POINT ( 'NONE',  ( 107.3288114731349197, 7.143999412540020799, -4.965851468055219264 ) ) ;
#57807 = DIRECTION ( 'NONE',  ( -0.000000000000000000, -1.000000000000000000, -0.000000000000000000 ) ) ;
#57808 = CARTESIAN_POINT ( 'NONE',  ( 12.89999999999990266, 2.500000000000000000, 3.637306695894644726 ) ) ;
#57809 = DIRECTION ( 'NONE',  ( 0.000000000000000000, 0.000000000000000000, -1.000000000000000000 ) ) ;
#57810 = EDGE_CURVE ( 'NONE', #69451, #38111, #111130, .T. ) ;
#57811 = ORIENTED_EDGE ( 'NONE', *, *, #42342, .F. ) ;
#57812 = ORIENTED_EDGE ( 'NONE', *, *, #37728, .T. ) ;
#57813 = ORIENTED_EDGE ( 'NONE', *, *, #75242, .T. ) ;
#57814 = ORIENTED_EDGE ( 'NONE', *, *, #1233, .F. ) ;
#57815 = FACE_OUTER_BOUND ( 'NONE', #120021, .T. ) ;
#57816 = CARTESIAN_POINT ( 'NONE',  ( -9.150000000000009237, 2.500000000000000000, -7.188010851410848723 ) ) ;
#57817 = CARTESIAN_POINT ( 'NONE',  ( 3.749999999999944045, 2.500000000000000000, -2.857883832488653741 ) ) ;
#57818 = ORIENTED_EDGE ( 'NONE', *, *, #69952, .F. ) ;
#57819 = EDGE_CURVE ( 'NONE', #42358, #25877, #15352, .T. ) ;
#57820 = FACE_BOUND ( 'NONE', #58376, .T. ) ;
#57821 = ORIENTED_EDGE ( 'NONE', *, *, #102339, .T. ) ;
#57822 = EDGE_CURVE ( 'NONE', #70467, #5264, #34167, .T. ) ;
#57823 = DIRECTION ( 'NONE',  ( 0.000000000000000000, 1.000000000000000000, 0.000000000000000000 ) ) ;
#57824 = DIRECTION ( 'NONE',  ( 0.000000000000000000, 0.000000000000000000, -1.000000000000000000 ) ) ;
#57825 = DIRECTION ( 'NONE',  ( -0.000000000000000000, 1.000000000000000000, -0.000000000000000000 ) ) ;
#57826 = CONICAL_SURFACE ( 'NONE', #1369, 0.1000000000000002554, 0.003490658503988666988 ) ;
#57827 = CARTESIAN_POINT ( 'NONE',  ( 1.649999999999951950, 12.50000000000000000, -5.737276932171712751 ) ) ;
#57828 = CONICAL_SURFACE ( 'NONE', #49425, 0.09999999999999982514, 0.003490658503988666988 ) ;
#57829 = DIRECTION ( 'NONE',  ( 0.000000000000000000, -0.9999939076577903929, 0.003490651415223739937 ) ) ;
#57830 = EDGE_CURVE ( 'NONE', #129204, #75499, #48746, .T. ) ;
#57831 = CARTESIAN_POINT ( 'NONE',  ( -12.49999999999999467, 12.50000000000000000, -3.637306695894647390 ) ) ;
#57832 = EDGE_CURVE ( 'NONE', #81547, #109936, #82188, .T. ) ;
#57833 = FACE_OUTER_BOUND ( 'NONE', #110326, .T. ) ;
#57834 = DIRECTION ( 'NONE',  ( 0.000000000000000000, 0.000000000000000000, 1.000000000000000000 ) ) ;
#57835 = ADVANCED_FACE ( 'NONE', ( #101987 ), #52243, .T. ) ;
#57836 = LINE ( 'NONE', #118670, #93652 ) ;
#57837 = EDGE_CURVE ( 'NONE', #21550, #110285, #100674, .T. ) ;
#57838 = EDGE_CURVE ( 'NONE', #107047, #97855, #55087, .T. ) ;
#57839 = DIRECTION ( 'NONE',  ( 0.000000000000000000, 0.000000000000000000, 1.000000000000000000 ) ) ;
#57841 = AXIS2_PLACEMENT_3D ( 'NONE', #59758, #118644, #86105 ) ;
#57840 = VECTOR ( 'NONE', #11859, 1000.000000000000000 ) ;
#57842 = ORIENTED_EDGE ( 'NONE', *, *, #53884, .T. ) ;
#57843 = EDGE_LOOP ( 'NONE', ( #48190, #1073 ) ) ;
#57844 = VERTEX_POINT ( 'NONE', #2469 ) ;
#57845 = ORIENTED_EDGE ( 'NONE', *, *, #52733, .F. ) ;
#57846 = CARTESIAN_POINT ( 'NONE',  ( -10.40000000000000213, 12.50000000000000000, -0.6928203230275541413 ) ) ;
#57847 = PLANE ( 'NONE',  #77840 ) ;
#57849 = ORIENTED_EDGE ( 'NONE', *, *, #5778, .T. ) ;
#57848 = ORIENTED_EDGE ( 'NONE', *, *, #75548, .T. ) ;
#57850 = EDGE_CURVE ( 'NONE', #124869, #35293, #12932, .T. ) ;
#57851 = ORIENTED_EDGE ( 'NONE', *, *, #43401, .F. ) ;
#57852 = DIRECTION ( 'NONE',  ( 0.000000000000000000, 0.000000000000000000, -1.000000000000000000 ) ) ;
#57854 = AXIS2_PLACEMENT_3D ( 'NONE', #34782, #94979, #36057 ) ;
#57853 = CONICAL_SURFACE ( 'NONE', #45333, 0.1000000000000000472, 0.003490658503988666988 ) ;
#57855 = AXIS2_PLACEMENT_3D ( 'NONE', #102755, #33405, #63494 ) ;
#57856 = PLANE ( 'NONE',  #99901 ) ;
#57857 = DIRECTION ( 'NONE',  ( 0.000000000000000000, 0.000000000000000000, -1.000000000000000000 ) ) ;
#57858 = DIRECTION ( 'NONE',  ( -0.000000000000000000, -1.000000000000000000, -0.000000000000000000 ) ) ;
#57859 = DIRECTION ( 'NONE',  ( 0.000000000000000000, 1.000000000000000000, 0.000000000000000000 ) ) ;
#57860 = DIRECTION ( 'NONE',  ( 0.000000000000000000, 0.000000000000000000, 1.000000000000000000 ) ) ;
#57861 = EDGE_LOOP ( 'NONE', ( #8726, #58171, #21946, #75520 ) ) ;
#57862 = LINE ( 'NONE', #109537, #49706 ) ;
#57863 = EDGE_LOOP ( 'NONE', ( #66650, #105037, #61818, #46182 ) ) ;
#57864 = ORIENTED_EDGE ( 'NONE', *, *, #86189, .T. ) ;
#57865 = ORIENTED_EDGE ( 'NONE', *, *, #94612, .T. ) ;
#57866 = DIRECTION ( 'NONE',  ( 0.000000000000000000, 0.000000000000000000, -1.000000000000000000 ) ) ;
#57867 = VERTEX_POINT ( 'NONE', #115001 ) ;
#57868 = CIRCLE ( 'NONE', #11869, 0.06509327318403745899 ) ;
#57869 = EDGE_LOOP ( 'NONE', ( #68891, #79809, #123205, #81519 ) ) ;
#57871 = CARTESIAN_POINT ( 'NONE',  ( 187.5000000000000000, 1.065442715258197248E-15, -8.699999999999999289 ) ) ;
#57870 = CIRCLE ( 'NONE', #14212, 0.1000000000000002554 ) ;
#57872 = CARTESIAN_POINT ( 'NONE',  ( -0.6500000000000389910, 2.500000000000000000, -1.818653347947326138 ) ) ;
#57874 = AXIS2_PLACEMENT_3D ( 'NONE', #1578, #41539, #42163 ) ;
#57873 = CARTESIAN_POINT ( 'NONE',  ( 7.899999999999924860, 12.50000000000000000, 4.330127018922196314 ) ) ;
#57875 = DIRECTION ( 'NONE',  ( 0.000000000000000000, -0.9999939076577903929, 0.003490651415223739937 ) ) ;
#57876 = CARTESIAN_POINT ( 'NONE',  ( -4.350000000000023626, 12.50000000000000000, 6.148780366869520897 ) ) ;
#57877 = EDGE_CURVE ( 'NONE', #14270, #93574, #32123, .T. ) ;
#57878 = VECTOR ( 'NONE', #63933, 1000.000000000000000 ) ;
#57879 = VERTEX_POINT ( 'NONE', #116291 ) ;
#57880 = ADVANCED_FACE ( 'NONE', ( #25335 ), #125480, .T. ) ;
#57882 = CONICAL_SURFACE ( 'NONE', #11886, 0.1000000000000002554, 0.003490658503988666988 ) ;
#57881 = CARTESIAN_POINT ( 'NONE',  ( 2.499999999999948930, 2.500000000000000000, -5.122947341949753763 ) ) ;
#57883 = ORIENTED_EDGE ( 'NONE', *, *, #16981, .T. ) ;
#57884 = AXIS2_PLACEMENT_3D ( 'NONE', #83202, #3975, #82562 ) ;
#57886 = ADVANCED_FACE ( 'NONE', ( #14224 ), #128263, .T. ) ;
#57885 = PLANE ( 'NONE',  #60962 ) ;
#57887 = ORIENTED_EDGE ( 'NONE', *, *, #120084, .T. ) ;
#57888 = CARTESIAN_POINT ( 'NONE',  ( 9.549999999999918998, 2.500000000000000000, 2.165063509461097713 ) ) ;
#57889 = DIRECTION ( 'NONE',  ( 0.000000000000000000, 0.000000000000000000, 1.000000000000000000 ) ) ;
#57890 = ORIENTED_EDGE ( 'NONE', *, *, #115148, .T. ) ;
#57891 = DIRECTION ( 'NONE',  ( 0.000000000000000000, 0.000000000000000000, 1.000000000000000000 ) ) ;
#57892 = CONICAL_SURFACE ( 'NONE', #5624, 0.09999999999999982514, 0.003490658503988666988 ) ;
#57893 = EDGE_CURVE ( 'NONE', #47267, #30241, #103916, .T. ) ;
#57894 = DIRECTION ( 'NONE',  ( -4.274815082592931898E-19, -0.9999939076577903929, -0.003490651415223739937 ) ) ;
#57895 = ORIENTED_EDGE ( 'NONE', *, *, #10814, .F. ) ;
#57896 = VECTOR ( 'NONE', #104153, 1000.000000000000000 ) ;
#57897 = EDGE_CURVE ( 'NONE', #109253, #4262, #40440, .T. ) ;
#57898 = ADVANCED_FACE ( 'NONE', ( #94093 ), #699, .T. ) ;
#57900 = ADVANCED_FACE ( 'NONE', ( #96024 ), #107311, .T. ) ;
#57899 = CIRCLE ( 'NONE', #66188, 0.1000000000000000472 ) ;
#57901 = DIRECTION ( 'NONE',  ( 0.000000000000000000, 0.000000000000000000, 1.000000000000000000 ) ) ;
#57902 = ORIENTED_EDGE ( 'NONE', *, *, #30941, .T. ) ;
#57903 = VERTEX_POINT ( 'NONE', #5053 ) ;
#57904 = DIRECTION ( 'NONE',  ( 0.000000000000000000, 1.000000000000000000, 0.000000000000000000 ) ) ;
#57905 = CARTESIAN_POINT ( 'NONE',  ( 7.299999999999927880, 12.50000000000000000, 3.983716857408420964 ) ) ;
#57906 = CARTESIAN_POINT ( 'NONE',  ( 186.4635416670080872, -4.367472073101519747, 7.564683531249999149 ) ) ;
#57907 = LINE ( 'NONE', #59857, #65852 ) ;
#57908 = EDGE_CURVE ( 'NONE', #73467, #128960, #17409, .T. ) ;
#57909 = DIRECTION ( 'NONE',  ( 0.000000000000000000, 1.000000000000000000, 0.000000000000000000 ) ) ;
#57910 = DIRECTION ( 'NONE',  ( 0.000000000000000000, 0.000000000000000000, -1.000000000000000000 ) ) ;
#57911 = AXIS2_PLACEMENT_3D ( 'NONE', #119000, #71848, #41111 ) ;
#57912 = VERTEX_POINT ( 'NONE', #15516 ) ;
#57913 = DIRECTION ( 'NONE',  ( 0.000000000000000000, -0.9999939076577903929, 0.003490651415223739937 ) ) ;
#57914 = PLANE ( 'NONE',  #104352 ) ;
#57915 = EDGE_LOOP ( 'NONE', ( #37862, #4844, #33525, #101911 ) ) ;
#57916 = PLANE ( 'NONE',  #41318 ) ;
#57918 = ADVANCED_FACE ( 'NONE', ( #115649 ), #54798, .T. ) ;
#57917 = DIRECTION ( 'NONE',  ( -0.000000000000000000, 1.000000000000000000, -0.000000000000000000 ) ) ;
#57919 = CARTESIAN_POINT ( 'NONE',  ( -7.100000000000017408, 12.50000000000000000, -4.957854068765716882 ) ) ;
#57920 = FACE_OUTER_BOUND ( 'NONE', #26284, .T. ) ;
#57921 = DIRECTION ( 'NONE',  ( 0.000000000000000000, 0.000000000000000000, -1.000000000000000000 ) ) ;
#57922 = ORIENTED_EDGE ( 'NONE', *, *, #50184, .T. ) ;
#57923 = AXIS2_PLACEMENT_3D ( 'NONE', #62107, #47449, #87350 ) ;
#57924 = CARTESIAN_POINT ( 'NONE',  ( -8.950000000000009948, 2.500000000000000000, -1.918653347947326004 ) ) ;
#57925 = CARTESIAN_POINT ( 'NONE',  ( -3.350000000000028955, 12.50000000000000000, -2.165063509461101710 ) ) ;
#57926 = ORIENTED_EDGE ( 'NONE', *, *, #26190, .T. ) ;
#57928 = CIRCLE ( 'NONE', #110240, 0.06509327318403745899 ) ;
#57927 = CONICAL_SURFACE ( 'NONE', #80914, 0.09999999999999982514, 0.003490658503988666988 ) ;
#57929 = DIRECTION ( 'NONE',  ( -4.274815082592931898E-19, -0.9999939076577903929, -0.003490651415223739937 ) ) ;
#57930 = EDGE_CURVE ( 'NONE', #77488, #49848, #56714, .T. ) ;
#57931 = VERTEX_POINT ( 'NONE', #73796 ) ;
#57932 = ORIENTED_EDGE ( 'NONE', *, *, #42465, .F. ) ;
#57933 = DIRECTION ( 'NONE',  ( 0.05223670945016072042, -0.9986347311133434435, 0.000000000000000000 ) ) ;
#57934 = EDGE_LOOP ( 'NONE', ( #52600, #21038 ) ) ;
#57935 = FACE_OUTER_BOUND ( 'NONE', #66862, .T. ) ;
#57936 = DIRECTION ( 'NONE',  ( 0.000000000000000000, 0.000000000000000000, 1.000000000000000000 ) ) ;
#57938 = CONICAL_SURFACE ( 'NONE', #43378, 0.09999999999999982514, 0.003490658503988666988 ) ;
#57937 = VECTOR ( 'NONE', #118909, 1000.000000000000000 ) ;
#57939 = DIRECTION ( 'NONE',  ( 0.000000000000000000, -0.000000000000000000, 1.000000000000000000 ) ) ;
#57940 = VERTEX_POINT ( 'NONE', #113744 ) ;
#57941 = CONICAL_SURFACE ( 'NONE', #103906, 0.09999999999999999167, 0.003490658503988666988 ) ;
#57942 = DIRECTION ( 'NONE',  ( 0.000000000000000000, 1.000000000000000000, 0.000000000000000000 ) ) ;
#57944 = ORIENTED_EDGE ( 'NONE', *, *, #78204, .F. ) ;
#57943 = DIRECTION ( 'NONE',  ( 0.000000000000000000, 0.000000000000000000, 1.000000000000000000 ) ) ;
#57945 = DIRECTION ( 'NONE',  ( 0.000000000000000000, -0.000000000000000000, 1.000000000000000000 ) ) ;
#57946 = ADVANCED_FACE ( 'NONE', ( #74454 ), #105156, .T. ) ;
#57947 = CARTESIAN_POINT ( 'NONE',  ( 0.8499999999999545697, 12.50000000000000000, 2.857883832488649301 ) ) ;
#57948 = ORIENTED_EDGE ( 'NONE', *, *, #26495, .T. ) ;
#57949 = ORIENTED_EDGE ( 'NONE', *, *, #8308, .F. ) ;
#57950 = ORIENTED_EDGE ( 'NONE', *, *, #64956, .F. ) ;
#57951 = CARTESIAN_POINT ( 'NONE',  ( -1.050000000000037348, 2.500000000000000000, -6.841600689897078702 ) ) ;
#57952 = DIRECTION ( 'NONE',  ( -0.000000000000000000, -1.000000000000000000, -0.000000000000000000 ) ) ;
#57953 = FACE_OUTER_BOUND ( 'NONE', #124550, .T. ) ;
#57954 = FACE_BOUND ( 'NONE', #125229, .T. ) ;
#57955 = ORIENTED_EDGE ( 'NONE', *, *, #24710, .T. ) ;
#57956 = CIRCLE ( 'NONE', #22470, 0.1000000000000002554 ) ;
#57957 = CARTESIAN_POINT ( 'NONE',  ( 1.249999999999952038, 2.500000000000000000, 5.802370205355744659 ) ) ;
#57958 = DIRECTION ( 'NONE',  ( -0.000000000000000000, -1.000000000000000000, -0.000000000000000000 ) ) ;
#57959 = VECTOR ( 'NONE', #60430, 1000.000000000000000 ) ;
#57960 = ORIENTED_EDGE ( 'NONE', *, *, #7664, .F. ) ;
#57961 = DIRECTION ( 'NONE',  ( -4.274815082592931898E-19, -0.9999939076577903929, -0.003490651415223739937 ) ) ;
#57962 = AXIS2_PLACEMENT_3D ( 'NONE', #35572, #24455, #115377 ) ;
#57963 = CARTESIAN_POINT ( 'NONE',  ( 5.849999999999932143, 2.500000000000000000, 2.165063509461097713 ) ) ;
#57964 = CARTESIAN_POINT ( 'NONE',  ( -1.850000000000033396, 2.500000000000000000, -6.941600689897077459 ) ) ;
#57965 = LINE ( 'NONE', #89355, #34726 ) ;
#57966 = CARTESIAN_POINT ( 'NONE',  ( 7.299999999999927880, 12.50000000000000000, -4.676537180435977881 ) ) ;
#57967 = AXIS2_PLACEMENT_3D ( 'NONE', #85503, #104494, #76334 ) ;
#57968 = AXIS2_PLACEMENT_3D ( 'NONE', #118441, #38626, #106050 ) ;
#57969 = EDGE_CURVE ( 'NONE', #65424, #81764, #126125, .T. ) ;
#57970 = ORIENTED_EDGE ( 'NONE', *, *, #128199, .T. ) ;
#57971 = ORIENTED_EDGE ( 'NONE', *, *, #96224, .T. ) ;
#57972 = ORIENTED_EDGE ( 'NONE', *, *, #65789, .T. ) ;
#57973 = EDGE_LOOP ( 'NONE', ( #66358, #16946, #87283, #75909 ) ) ;
#57974 = ORIENTED_EDGE ( 'NONE', *, *, #83799, .T. ) ;
#57975 = CARTESIAN_POINT ( 'NONE',  ( 14.79999999999989413, 12.50000000000000000, -0.3464101615137782364 ) ) ;
#57976 = CARTESIAN_POINT ( 'NONE',  ( -1.900000000000035438, 2.500000000000000000, 3.983716857408420076 ) ) ;
#57977 = CIRCLE ( 'NONE', #45468, 3.000000000000000000 ) ;
#57978 = ORIENTED_EDGE ( 'NONE', *, *, #99415, .F. ) ;
#57979 = FACE_BOUND ( 'NONE', #100572, .T. ) ;
#57980 = ADVANCED_FACE ( 'NONE', ( #34553 ), #92648, .T. ) ;
#57981 = CARTESIAN_POINT ( 'NONE',  ( 2.499999999999947153, 2.500000000000000000, 3.637306695894644726 ) ) ;
#57983 = CIRCLE ( 'NONE', #91418, 0.06509327318403745899 ) ;
#57982 = AXIS2_PLACEMENT_3D ( 'NONE', #127260, #107606, #17931 ) ;
#57984 = PLANE ( 'NONE',  #17801 ) ;
#57985 = EDGE_CURVE ( 'NONE', #102525, #62269, #94728, .T. ) ;
#57986 = CARTESIAN_POINT ( 'NONE',  ( 6.699999999999928235, 2.500000000000000000, -2.276824562219559311E-15 ) ) ;
#57987 = ADVANCED_FACE ( 'NONE', ( #65257 ), #36222, .T. ) ;
#57988 = PLANE ( 'NONE',  #124305 ) ;
#57989 = ADVANCED_FACE ( 'NONE', ( #35817 ), #21641, .T. ) ;
#57990 = DIRECTION ( 'NONE',  ( 0.000000000000000000, 1.000000000000000000, 0.000000000000000000 ) ) ;
#57991 = EDGE_CURVE ( 'NONE', #99644, #73222, #38383, .T. ) ;
#57992 = ORIENTED_EDGE ( 'NONE', *, *, #81200, .T. ) ;
#57993 = CARTESIAN_POINT ( 'NONE',  ( 11.04999999999991189, 2.500000000000000000, 6.048780366869521252 ) ) ;
#57994 = ORIENTED_EDGE ( 'NONE', *, *, #60092, .T. ) ;
#57995 = ORIENTED_EDGE ( 'NONE', *, *, #75595, .F. ) ;
#57996 = ORIENTED_EDGE ( 'NONE', *, *, #20241, .T. ) ;
#57997 = CARTESIAN_POINT ( 'NONE',  ( 5.199999999999933564, 2.500000000000000000, 3.983716857408420076 ) ) ;
#57998 = DIRECTION ( 'NONE',  ( -0.000000000000000000, 1.000000000000000000, -0.000000000000000000 ) ) ;
#57999 = DIRECTION ( 'NONE',  ( 0.000000000000000000, 0.000000000000000000, 1.000000000000000000 ) ) ;
#58000 = ORIENTED_EDGE ( 'NONE', *, *, #15098, .T. ) ;
#58002 = EDGE_CURVE ( 'NONE', #7162, #75768, #69658, .T. ) ;
#58001 = CONICAL_SURFACE ( 'NONE', #32971, 0.09999999999999982514, 0.003490658503988666988 ) ;
#58003 = CARTESIAN_POINT ( 'NONE',  ( -13.14999999999999147, 12.50000000000000000, 1.883746621131362931 ) ) ;
#58004 = EDGE_CURVE ( 'NONE', #122177, #54834, #58045, .T. ) ;
#58005 = DIRECTION ( 'NONE',  ( -0.000000000000000000, -1.000000000000000000, -0.000000000000000000 ) ) ;
#58006 = EDGE_CURVE ( 'NONE', #102543, #29350, #52944, .T. ) ;
#58007 = CARTESIAN_POINT ( 'NONE',  ( -2.700000000000030820, 2.500000000000000000, -3.983716857408426293 ) ) ;
#58008 = CARTESIAN_POINT ( 'NONE',  ( 185.4010416670080588, -4.367472073101519747, 7.564683531249999149 ) ) ;
#58009 = DIRECTION ( 'NONE',  ( -0.000000000000000000, -1.000000000000000000, -0.000000000000000000 ) ) ;
#58010 = PLANE ( 'NONE',  #121993 ) ;
#58011 = DIRECTION ( 'NONE',  ( 0.000000000000000000, 0.000000000000000000, 1.000000000000000000 ) ) ;
#58012 = ORIENTED_EDGE ( 'NONE', *, *, #82559, .F. ) ;
#58013 = CARTESIAN_POINT ( 'NONE',  ( -2.500000000000032419, 12.50000000000000000, -3.702399969078687292 ) ) ;
#58014 = CIRCLE ( 'NONE', #18283, 0.06509327318403745899 ) ;
#58015 = ORIENTED_EDGE ( 'NONE', *, *, #34946, .T. ) ;
#58016 = TOROIDAL_SURFACE ( 'NONE', #37086, 7.541925104783893552, 0.5000000000000000000 ) ;
#58017 = VERTEX_POINT ( 'NONE', #99899 ) ;
#58018 = LINE ( 'NONE', #27246, #13350 ) ;
#58019 = DIRECTION ( 'NONE',  ( 0.000000000000000000, -0.000000000000000000, 1.000000000000000000 ) ) ;
#58020 = DIRECTION ( 'NONE',  ( 0.000000000000000000, 1.000000000000000000, 0.000000000000000000 ) ) ;
#58021 = B_SPLINE_CURVE_WITH_KNOTS ( 'NONE', 3,
 ( #72800, #52499, #34166, #122545, #24340, #92428, #2754, #64252 ),
 .UNSPECIFIED., .F., .F.,
 ( 4, 2, 2, 4 ),
 ( 0.000000000000000000, 0.001904977314309959542, 0.002857465971464944084, 0.003809954628619929059 ),
 .UNSPECIFIED. ) ;
#58022 = ORIENTED_EDGE ( 'NONE', *, *, #119899, .T. ) ;
#58025 = EDGE_LOOP ( 'NONE', ( #69262, #68972, #65726, #71350 ) ) ;
#58024 = CONICAL_SURFACE ( 'NONE', #103990, 0.09999999999999982514, 0.003490658503988666988 ) ;
#58023 = AXIS2_PLACEMENT_3D ( 'NONE', #14904, #71944, #122335 ) ;
#58026 = DIRECTION ( 'NONE',  ( 0.000000000000000000, 0.000000000000000000, 1.000000000000000000 ) ) ;
#58027 = CIRCLE ( 'NONE', #18297, 0.06509327318403745899 ) ;
#58028 = DIRECTION ( 'NONE',  ( 0.000000000000000000, 0.000000000000000000, -1.000000000000000000 ) ) ;
#58029 = DIRECTION ( 'NONE',  ( -0.000000000000000000, 1.000000000000000000, -0.000000000000000000 ) ) ;
#58030 = ORIENTED_EDGE ( 'NONE', *, *, #75599, .F. ) ;
#58031 = EDGE_LOOP ( 'NONE', ( #99148, #75082 ) ) ;
#58032 = DIRECTION ( 'NONE',  ( 0.000000000000000000, 0.000000000000000000, 1.000000000000000000 ) ) ;
#58033 = AXIS2_PLACEMENT_3D ( 'NONE', #6203, #112957, #85427 ) ;
#58034 = VERTEX_POINT ( 'NONE', #116935 ) ;
#58035 = CARTESIAN_POINT ( 'NONE',  ( 11.24999999999994493, 12.50000000000000000, -2.099970236277064473 ) ) ;
#58036 = CARTESIAN_POINT ( 'NONE',  ( -5.200000000000022382, 12.50000000000000000, 4.676537180435972552 ) ) ;
#58037 = EDGE_LOOP ( 'NONE', ( #100076, #866, #112697, #9312 ) ) ;
#58038 = CARTESIAN_POINT ( 'NONE',  ( 6.049999999999930544, 2.500000000000000000, 2.511473670974873507 ) ) ;
#58039 = CARTESIAN_POINT ( 'NONE',  ( -12.04999999999999538, 2.500000000000000000, 2.265063509461097357 ) ) ;
#58040 = FACE_BOUND ( 'NONE', #83926, .T. ) ;
#58041 = EDGE_CURVE ( 'NONE', #53470, #118758, #86376, .T. ) ;
#58042 = DIRECTION ( 'NONE',  ( -0.000000000000000000, -1.000000000000000000, -0.000000000000000000 ) ) ;
#58043 = ORIENTED_EDGE ( 'NONE', *, *, #16829, .F. ) ;
#58044 = EDGE_CURVE ( 'NONE', #67250, #122182, #29964, .T. ) ;
#58046 = AXIS2_PLACEMENT_3D ( 'NONE', #45436, #23865, #46715 ) ;
#58045 = LINE ( 'NONE', #48213, #94796 ) ;
#58047 = B_SPLINE_CURVE_WITH_KNOTS ( 'NONE', 3,
 ( #21374, #18788, #109094, #11548 ),
 .UNSPECIFIED., .F., .F.,
 ( 4, 4 ),
 ( 0.0001556283592081808000, 0.002283789722394648485 ),
 .UNSPECIFIED. ) ;
#58048 = EDGE_CURVE ( 'NONE', #53017, #18181, #6562, .T. ) ;
#58049 = ORIENTED_EDGE ( 'NONE', *, *, #35822, .F. ) ;
#58050 = ORIENTED_EDGE ( 'NONE', *, *, #62963, .T. ) ;
#58051 = CARTESIAN_POINT ( 'NONE',  ( -2.900000000000029665, 2.500000000000000000, 4.330127018922196314 ) ) ;
#58052 = DIRECTION ( 'NONE',  ( 0.000000000000000000, -0.000000000000000000, 1.000000000000000000 ) ) ;
#58053 = DIRECTION ( 'NONE',  ( 0.000000000000000000, 0.000000000000000000, 1.000000000000000000 ) ) ;
#58054 = CARTESIAN_POINT ( 'NONE',  ( 9.999999999999912959, 12.50000000000000000, -4.957854068765716882 ) ) ;
#58055 = VECTOR ( 'NONE', #15634, 1000.000000000000000 ) ;
#58057 = CIRCLE ( 'NONE', #112331, 0.06509327318403745899 ) ;
#58056 = DIRECTION ( 'NONE',  ( 0.000000000000000000, 1.000000000000000000, 0.000000000000000000 ) ) ;
#58058 = ADVANCED_FACE ( 'NONE', ( #88784 ), #50683, .T. ) ;
#58059 = CARTESIAN_POINT ( 'NONE',  ( 5.849999999999932143, 12.50000000000000000, 1.407149913249508000 ) ) ;
#58060 = COLOUR_RGB ( '', 0.66274510, 0.83137255, 0.94901961) ;
#58061 = CARTESIAN_POINT ( 'NONE',  ( 17.46224641143689382, 2.499999999999373834, -5.244174873149315630 ) ) ;
#58062 = DIRECTION ( 'NONE',  ( -0.000000000000000000, -1.000000000000000000, -0.000000000000000000 ) ) ;
#58063 = FACE_OUTER_BOUND ( 'NONE', #51571, .T. ) ;
#58064 = CIRCLE ( 'NONE', #20501, 0.09999999999999982514 ) ;
#58065 = CIRCLE ( 'NONE', #1604, 0.06509327318403745899 ) ;
#58066 = DIRECTION ( 'NONE',  ( -0.000000000000000000, 1.000000000000000000, -0.000000000000000000 ) ) ;
#58067 = ORIENTED_EDGE ( 'NONE', *, *, #5113, .F. ) ;
#58068 = DIRECTION ( 'NONE',  ( 0.000000000000000000, -0.9999939076577903929, 0.003490651415223739937 ) ) ;
#58069 = AXIS2_PLACEMENT_3D ( 'NONE', #58665, #98554, #27908 ) ;
#58070 = PLANE ( 'NONE',  #14455 ) ;
#58071 = LINE ( 'NONE', #39088, #51682 ) ;
#58072 = EDGE_CURVE ( 'NONE', #126604, #11408, #80132, .T. ) ;
#58073 = DIRECTION ( 'NONE',  ( 0.000000000000000000, 0.000000000000000000, 1.000000000000000000 ) ) ;
#58074 = CARTESIAN_POINT ( 'NONE',  ( 13.74999999999993427, 2.500000000000000000, 2.265063509461097357 ) ) ;
#58075 = ORIENTED_EDGE ( 'NONE', *, *, #40574, .F. ) ;
#58076 = DIRECTION ( 'NONE',  ( 0.000000000000000000, -0.9999939076577903929, 0.003490651415223739937 ) ) ;
#58078 = CONICAL_SURFACE ( 'NONE', #74799, 0.1000000000000002554, 0.003490658503988666988 ) ;
#58077 = AXIS2_PLACEMENT_3D ( 'NONE', #3454, #72207, #21152 ) ;
#58079 = DIRECTION ( 'NONE',  ( 0.000000000000000000, 0.000000000000000000, 1.000000000000000000 ) ) ;
#58081 = ORIENTED_EDGE ( 'NONE', *, *, #12865, .F. ) ;
#58080 = DIRECTION ( 'NONE',  ( 0.000000000000000000, 1.000000000000000000, 0.000000000000000000 ) ) ;
#58082 = APPLICATION_CONTEXT ( 'automotive_design' ) ;
#58083 = EDGE_LOOP ( 'NONE', ( #102778, #34731 ) ) ;
#58084 = DIRECTION ( 'NONE',  ( -0.000000000000000000, 1.000000000000000000, -0.000000000000000000 ) ) ;
#58086 = ORIENTED_EDGE ( 'NONE', *, *, #85265, .T. ) ;
#58085 = EDGE_CURVE ( 'NONE', #129486, #108759, #23793, .T. ) ;
#58087 = VERTEX_POINT ( 'NONE', #67848 ) ;
#58088 = ORIENTED_EDGE ( 'NONE', *, *, #117794, .T. ) ;
#58089 = DIRECTION ( 'NONE',  ( 0.000000000000000000, 0.000000000000000000, 1.000000000000000000 ) ) ;
#58090 = CARTESIAN_POINT ( 'NONE',  ( -13.74999999999998934, 2.500000000000000000, 2.757883832488653209 ) ) ;
#58091 = LINE ( 'NONE', #29916, #115232 ) ;
#58092 = DIRECTION ( 'NONE',  ( 0.000000000000000000, 0.000000000000000000, 1.000000000000000000 ) ) ;
#58093 = VERTEX_POINT ( 'NONE', #118889 ) ;
#58094 = DIRECTION ( 'NONE',  ( 0.000000000000000000, 0.000000000000000000, 1.000000000000000000 ) ) ;
#58095 = ORIENTED_EDGE ( 'NONE', *, *, #23719, .F. ) ;
#58096 = DIRECTION ( 'NONE',  ( 0.000000000000000000, -0.9999939076577903929, 0.003490651415223739937 ) ) ;
#58097 = FACE_OUTER_BOUND ( 'NONE', #50203, .T. ) ;
#58098 = CONICAL_SURFACE ( 'NONE', #68542, 0.1000000000000000056, 0.003490658503988666988 ) ;
#58099 = CARTESIAN_POINT ( 'NONE',  ( 20.25366426269097886, 2.573118374675824604, 4.179292740213257140 ) ) ;
#58100 = CARTESIAN_POINT ( 'NONE',  ( 184.5000000000000000, 0.000000000000000000, 0.000000000000000000 ) ) ;
#58101 = EDGE_CURVE ( 'NONE', #66180, #997, #67689, .T. ) ;
#58102 = CARTESIAN_POINT ( 'NONE',  ( 3.549999999999943867, 2.500000000000000000, -1.918653347947326004 ) ) ;
#58103 = EDGE_LOOP ( 'NONE', ( #59768, #41682 ) ) ;
#58104 = AXIS2_PLACEMENT_3D ( 'NONE', #34202, #65575, #13890 ) ;
#58105 = AXIS2_PLACEMENT_3D ( 'NONE', #87843, #110081, #108137 ) ;
#58106 = ORIENTED_EDGE ( 'NONE', *, *, #112521, .T. ) ;
#58107 = ORIENTED_EDGE ( 'NONE', *, *, #101753, .T. ) ;
#58108 = ORIENTED_EDGE ( 'NONE', *, *, #39988, .T. ) ;
#58109 = ORIENTED_EDGE ( 'NONE', *, *, #5843, .T. ) ;
#58110 = CARTESIAN_POINT ( 'NONE',  ( 4.999999999999935163, 2.500000000000000000, 0.6928203230275494784 ) ) ;
#58111 = CARTESIAN_POINT ( 'NONE',  ( -12.89999999999999147, 12.50000000000000000, 3.637306695894644726 ) ) ;
#58112 = EDGE_CURVE ( 'NONE', #72972, #70798, #78337, .T. ) ;
#58113 = DIRECTION ( 'NONE',  ( 0.000000000000000000, -0.000000000000000000, 1.000000000000000000 ) ) ;
#58114 = FACE_BOUND ( 'NONE', #19421, .T. ) ;
#58115 = DIRECTION ( 'NONE',  ( 0.000000000000000000, 1.000000000000000000, 0.000000000000000000 ) ) ;
#58116 = CARTESIAN_POINT ( 'NONE',  ( 186.6979166673494603, 6.668395609140176816, 3.850000000000000977 ) ) ;
#58117 = CONICAL_SURFACE ( 'NONE', #74830, 0.09999999999999982514, 0.003490658503988666988 ) ;
#58118 = PLANE ( 'NONE',  #108293 ) ;
#58119 = PLANE ( 'NONE',  #129558 ) ;
#58120 = AXIS2_PLACEMENT_3D ( 'NONE', #29528, #19707, #59663 ) ;
#58121 = CIRCLE ( 'NONE', #95760, 0.1000000000000000472 ) ;
#58122 = CARTESIAN_POINT ( 'NONE',  ( 185.0468750003414300, -8.734944146203032389, -1.604583208406767949E-15 ) ) ;
#58123 = CARTESIAN_POINT ( 'NONE',  ( 3.549999999999944755, 12.50000000000000000, -2.511473670974877948 ) ) ;
#58124 = CARTESIAN_POINT ( 'NONE',  ( 0.3999999999999628852, 12.50000000000000000, 0.7579135962115892688 ) ) ;
#58125 = AXIS2_PLACEMENT_3D ( 'NONE', #104174, #46529, #98212 ) ;
#58126 = FACE_OUTER_BOUND ( 'NONE', #12059, .T. ) ;
#58127 = EDGE_CURVE ( 'NONE', #118142, #137, #87476, .T. ) ;
#58128 = VERTEX_POINT ( 'NONE', #90056 ) ;
#58129 = ORIENTED_EDGE ( 'NONE', *, *, #39529, .F. ) ;
#58130 = ORIENTED_EDGE ( 'NONE', *, *, #94195, .F. ) ;
#58131 = ORIENTED_EDGE ( 'NONE', *, *, #21714, .T. ) ;
#58132 = CONICAL_SURFACE ( 'NONE', #55958, 0.09999999999999982514, 0.003490658503988666988 ) ;
#58133 = CARTESIAN_POINT ( 'NONE',  ( -2.700000000000029932, 2.500000000000000000, -0.3464101615137782364 ) ) ;
#58134 = FACE_BOUND ( 'NONE', #52165, .T. ) ;
#58135 = CARTESIAN_POINT ( 'NONE',  ( 9.349999999999916156, 2.500000000000000000, -2.511473670974877948 ) ) ;
#58136 = EDGE_CURVE ( 'NONE', #96773, #85603, #84419, .T. ) ;
#58137 = CONICAL_SURFACE ( 'NONE', #20482, 0.09999999999999999167, 0.003490658503988666988 ) ;
#58138 = EDGE_LOOP ( 'NONE', ( #742, #75732, #123405, #73599 ) ) ;
#58139 = ADVANCED_FACE ( 'NONE', ( #57393 ), #9111, .T. ) ;
#58140 = DIRECTION ( 'NONE',  ( 0.000000000000000000, 0.000000000000000000, 1.000000000000000000 ) ) ;
#58141 = EDGE_CURVE ( 'NONE', #84654, #109940, #109043, .T. ) ;
#58142 = FACE_OUTER_BOUND ( 'NONE', #7718, .T. ) ;
#58143 = ADVANCED_FACE ( 'NONE', ( #49518 ), #69754, .T. ) ;
#58144 = CARTESIAN_POINT ( 'NONE',  ( -13.14999999999999147, 2.500000000000000000, 2.511473670974877503 ) ) ;
#58145 = CIRCLE ( 'NONE', #1686, 1.388921157871087386 ) ;
#58146 = EDGE_CURVE ( 'NONE', #70759, #97670, #20056, .T. ) ;
#58147 = ORIENTED_EDGE ( 'NONE', *, *, #91858, .T. ) ;
#58148 = CARTESIAN_POINT ( 'NONE',  ( 10.64999999999990976, 12.50000000000000000, -6.906693963081115051 ) ) ;
#58149 = AXIS2_PLACEMENT_3D ( 'NONE', #28235, #98894, #100195 ) ;
#58150 = DIRECTION ( 'NONE',  ( 0.000000000000000000, 1.000000000000000000, 0.000000000000000000 ) ) ;
#58151 = ORIENTED_EDGE ( 'NONE', *, *, #93477, .F. ) ;
#58152 = EDGE_CURVE ( 'NONE', #85724, #63281, #61917, .T. ) ;
#58153 = ORIENTED_EDGE ( 'NONE', *, *, #21602, .F. ) ;
#58154 = DIRECTION ( 'NONE',  ( 0.000000000000000000, 1.000000000000000000, 0.000000000000000000 ) ) ;
#58155 = EDGE_CURVE ( 'NONE', #37369, #47582, #78177, .T. ) ;
#58156 = CARTESIAN_POINT ( 'NONE',  ( 12.94999999999990337, 2.500000000000000000, 2.165063509461097713 ) ) ;
#58157 = CIRCLE ( 'NONE', #47490, 0.06509327318403745899 ) ;
#58158 = ADVANCED_FACE ( 'NONE', ( #13429 ), #38474, .T. ) ;
#58159 = EDGE_CURVE ( 'NONE', #93574, #14270, #98996, .T. ) ;
#58160 = CARTESIAN_POINT ( 'NONE',  ( -7.700000000000014388, 12.50000000000000000, -4.676537180435977881 ) ) ;
#58161 = ADVANCED_FACE ( 'NONE', ( #42937 ), #34268, .T. ) ;
#58162 = CARTESIAN_POINT ( 'NONE',  ( -9.600000000000008527, 12.50000000000000000, 4.330127018922196314 ) ) ;
#58163 = ORIENTED_EDGE ( 'NONE', *, *, #35282, .F. ) ;
#58164 = DIRECTION ( 'NONE',  ( 0.000000000000000000, 1.000000000000000000, 0.000000000000000000 ) ) ;
#58165 = ORIENTED_EDGE ( 'NONE', *, *, #109126, .F. ) ;
#58166 = VERTEX_POINT ( 'NONE', #72382 ) ;
#58167 = AXIS2_PLACEMENT_3D ( 'NONE', #116384, #27352, #8364 ) ;
#58168 = EDGE_CURVE ( 'NONE', #52604, #45554, #107106, .T. ) ;
#58169 = DIRECTION ( 'NONE',  ( 0.000000000000000000, 0.000000000000000000, -1.000000000000000000 ) ) ;
#58170 = ADVANCED_FACE ( 'NONE', ( #30532 ), #56920, .T. ) ;
#58171 = ORIENTED_EDGE ( 'NONE', *, *, #23375, .T. ) ;
#58172 = DIRECTION ( 'NONE',  ( 0.000000000000000000, 0.000000000000000000, 1.000000000000000000 ) ) ;
#58173 = FACE_BOUND ( 'NONE', #80796, .T. ) ;
#58175 = CIRCLE ( 'NONE', #110381, 0.06509327318403745899 ) ;
#58174 = AXIS2_PLACEMENT_3D ( 'NONE', #114683, #16471, #64300 ) ;
#58176 = VERTEX_POINT ( 'NONE', #40997 ) ;
#58177 = CARTESIAN_POINT ( 'NONE',  ( -8.350000000000013856, 2.500000000000000000, 2.165063509461097713 ) ) ;
#58178 = ORIENTED_EDGE ( 'NONE', *, *, #83839, .F. ) ;
#58179 = CARTESIAN_POINT ( 'NONE',  ( 194.5000000000000000, 0.000000000000000000, 0.000000000000000000 ) ) ;
#58180 = FACE_OUTER_BOUND ( 'NONE', #30666, .T. ) ;
#58181 = FACE_OUTER_BOUND ( 'NONE', #41817, .T. ) ;
#58182 = CARTESIAN_POINT ( 'NONE',  ( 10.84999999999991260, 12.50000000000000000, 7.122917578226811486 ) ) ;
#58183 = DIRECTION ( 'NONE',  ( 0.000000000000000000, 0.000000000000000000, 1.000000000000000000 ) ) ;
#58184 = EDGE_LOOP ( 'NONE', ( #15989, #4927, #20993, #62586 ) ) ;
#58185 = ORIENTED_EDGE ( 'NONE', *, *, #87516, .T. ) ;
#58186 = ORIENTED_EDGE ( 'NONE', *, *, #68518, .F. ) ;
#58187 = DIRECTION ( 'NONE',  ( -0.000000000000000000, -1.000000000000000000, -0.000000000000000000 ) ) ;
#58188 = LINE ( 'NONE', #48347, #76576 ) ;
#58189 = DIRECTION ( 'NONE',  ( 0.000000000000000000, 0.000000000000000000, 1.000000000000000000 ) ) ;
#58192 = VERTEX_POINT ( 'NONE', #40343 ) ;
#58191 = VERTEX_POINT ( 'NONE', #81543 ) ;
#58190 = VECTOR ( 'NONE', #21742, 1000.000000000000000 ) ;
#58193 = ORIENTED_EDGE ( 'NONE', *, *, #9692, .F. ) ;
#58194 = CARTESIAN_POINT ( 'NONE',  ( -12.49999999999995914, 2.500000000000000000, -4.230127018922199333 ) ) ;
#58195 = DIRECTION ( 'NONE',  ( 0.000000000000000000, 0.000000000000000000, 1.000000000000000000 ) ) ;
#58196 = VECTOR ( 'NONE', #78688, 1000.000000000000000 ) ;
#58197 = APPLICATION_PROTOCOL_DEFINITION ( 'draft international standard', 'automotive_design', 1998, #51407 ) ;
#58198 = DIRECTION ( 'NONE',  ( 0.000000000000000000, 1.000000000000000000, 0.000000000000000000 ) ) ;
#58199 = FACE_OUTER_BOUND ( 'NONE', #49143, .T. ) ;
#58200 = CONICAL_SURFACE ( 'NONE', #1728, 0.1000000000000002554, 0.003490658503988666988 ) ;
#58201 = DIRECTION ( 'NONE',  ( 0.000000000000000000, 0.000000000000000000, 1.000000000000000000 ) ) ;
#58202 = CARTESIAN_POINT ( 'NONE',  ( 3.749999999999978684, 12.50000000000000000, -2.099970236277064473 ) ) ;
#58203 = CARTESIAN_POINT ( 'NONE',  ( 129.5000000000000000, -1.500000000000000000, 0.000000000000000000 ) ) ;
#58204 = CARTESIAN_POINT ( 'NONE',  ( 184.6562500006828031, 8.891194145520236347, 5.444286225454521982E-16 ) ) ;
#58205 = ORIENTED_EDGE ( 'NONE', *, *, #109422, .T. ) ;
#58207 = ORIENTED_EDGE ( 'NONE', *, *, #8158, .F. ) ;
#58206 = AXIS2_PLACEMENT_3D ( 'NONE', #124355, #34705, #104066 ) ;
#58208 = EDGE_CURVE ( 'NONE', #49054, #30916, #22638, .T. ) ;
#58210 = CARTESIAN_POINT ( 'NONE',  ( 13.14999999999990088, 12.50000000000000000, 2.511473670974873507 ) ) ;
#58209 = AXIS2_PLACEMENT_3D ( 'NONE', #36471, #37106, #125469 ) ;
#58211 = ADVANCED_FACE ( 'NONE', ( #101828 ), #12780, .T. ) ;
#58212 = DIRECTION ( 'NONE',  ( 0.000000000000000000, 0.000000000000000000, 1.000000000000000000 ) ) ;
#58213 = ORIENTED_EDGE ( 'NONE', *, *, #102812, .T. ) ;
#58214 = ORIENTED_EDGE ( 'NONE', *, *, #59037, .T. ) ;
#58215 = CARTESIAN_POINT ( 'NONE',  ( 186.6510416670080303, 4.367472073101518859, -7.564683531249999149 ) ) ;
#58216 = CARTESIAN_POINT ( 'NONE',  ( 2.899999999999946620, 12.50000000000000000, -0.7579135962115917113 ) ) ;
#58217 = CARTESIAN_POINT ( 'NONE',  ( 8.299999999999922551, 2.500000000000000000, -4.330127018922201643 ) ) ;
#58218 = CIRCLE ( 'NONE', #20551, 0.06509327318403745899 ) ;
#58219 = EDGE_CURVE ( 'NONE', #47326, #129522, #119927, .T. ) ;
#58220 = DIRECTION ( 'NONE',  ( 0.000000000000000000, 0.000000000000000000, 1.000000000000000000 ) ) ;
#58221 = VECTOR ( 'NONE', #45185, 1000.000000000000000 ) ;
#58222 = CARTESIAN_POINT ( 'NONE',  ( 185.0416666666667140, -4.445597072760063107, 7.700000000000102318 ) ) ;
#58223 = CARTESIAN_POINT ( 'NONE',  ( -5.650000000000023448, 2.500000000000000000, -2.511473670974877948 ) ) ;
#58224 = DIRECTION ( 'NONE',  ( -4.274815082592931898E-19, -0.9999939076577903929, -0.003490651415223739937 ) ) ;
#58225 = ORIENTED_EDGE ( 'NONE', *, *, #107633, .T. ) ;
#58226 = DIRECTION ( 'NONE',  ( 0.000000000000000000, 0.000000000000000000, 1.000000000000000000 ) ) ;
#58227 = CARTESIAN_POINT ( 'NONE',  ( -9.150000000000009237, 2.500000000000000000, -6.495190528383297135 ) ) ;
#58228 = EDGE_LOOP ( 'NONE', ( #2002, #120578 ) ) ;
#58229 = VERTEX_POINT ( 'NONE', #53381 ) ;
#58230 = CIRCLE ( 'NONE', #79160, 0.06509327318403745899 ) ;
#58231 = ORIENTED_EDGE ( 'NONE', *, *, #117838, .F. ) ;
#58232 = EDGE_LOOP ( 'NONE', ( #10317, #87522 ) ) ;
#58233 = DIRECTION ( 'NONE',  ( 0.000000000000000000, 1.000000000000000000, 0.000000000000000000 ) ) ;
#58234 = CARTESIAN_POINT ( 'NONE',  ( -14.34999999999998543, 2.500000000000000000, 1.918653347947325338 ) ) ;
#58235 = VECTOR ( 'NONE', #31339, 1000.000000000000000 ) ;
#58236 = ORIENTED_EDGE ( 'NONE', *, *, #85416, .F. ) ;
#58237 = CARTESIAN_POINT ( 'NONE',  ( 9.999999999999911182, 12.50000000000000000, 5.022947341949748790 ) ) ;
#58238 = CARTESIAN_POINT ( 'NONE',  ( -10.20000000000000462, 12.50000000000000000, 0.4115034346978109769 ) ) ;
#58239 = CARTESIAN_POINT ( 'NONE',  ( -6.250000000000021316, 12.50000000000000000, -5.802370205355749988 ) ) ;
#58241 = EDGE_LOOP ( 'NONE', ( #39625, #79086, #39787, #73065 ) ) ;
#58240 = DIRECTION ( 'NONE',  ( 0.000000000000000000, 1.000000000000000000, 0.000000000000000000 ) ) ;
#58242 = DIRECTION ( 'NONE',  ( 0.000000000000000000, 0.000000000000000000, 1.000000000000000000 ) ) ;
#58243 = CIRCLE ( 'NONE', #10110, 0.09999999999999982514 ) ;
#58244 = CARTESIAN_POINT ( 'NONE',  ( -8.950000000000011724, 12.50000000000000000, -6.213873640053559022 ) ) ;
#58245 = EDGE_CURVE ( 'NONE', #80023, #30581, #80229, .T. ) ;
#58246 = ORIENTED_EDGE ( 'NONE', *, *, #127782, .F. ) ;
#58247 = CIRCLE ( 'NONE', #8040, 0.06509327318403741736 ) ;
#58248 = ORIENTED_EDGE ( 'NONE', *, *, #125068, .F. ) ;
#58249 = ORIENTED_EDGE ( 'NONE', *, *, #21778, .T. ) ;
#58250 = FACE_OUTER_BOUND ( 'NONE', #93906, .T. ) ;
#58251 = DIRECTION ( 'NONE',  ( -0.000000000000000000, 1.000000000000000000, -0.000000000000000000 ) ) ;
#58253 = ORIENTED_EDGE ( 'NONE', *, *, #76459, .F. ) ;
#58252 = EDGE_CURVE ( 'NONE', #106738, #16690, #122755, .T. ) ;
#58254 = CARTESIAN_POINT ( 'NONE',  ( -11.84999999999999787, 12.50000000000000000, -2.511473670974873951 ) ) ;
#58255 = LINE ( 'NONE', #98153, #35005 ) ;
#58256 = DIRECTION ( 'NONE',  ( 0.000000000000000000, -0.000000000000000000, 1.000000000000000000 ) ) ;
#58257 = FACE_OUTER_BOUND ( 'NONE', #127725, .T. ) ;
#58258 = EDGE_CURVE ( 'NONE', #115125, #74692, #493, .T. ) ;
#58259 = VERTEX_POINT ( 'NONE', #73010 ) ;
#58260 = AXIS2_PLACEMENT_3D ( 'NONE', #53315, #93234, #34974 ) ;
#58261 = DIRECTION ( 'NONE',  ( 0.000000000000000000, 1.000000000000000000, 0.000000000000000000 ) ) ;
#58262 = EDGE_LOOP ( 'NONE', ( #31574, #4661 ) ) ;
#58263 = ORIENTED_EDGE ( 'NONE', *, *, #10828, .F. ) ;
#58264 = DIRECTION ( 'NONE',  ( -0.000000000000000000, 1.000000000000000000, -0.000000000000000000 ) ) ;
#58265 = EDGE_CURVE ( 'NONE', #13639, #26682, #31171, .T. ) ;
#58266 = FACE_OUTER_BOUND ( 'NONE', #73420, .T. ) ;
#58267 = FACE_BOUND ( 'NONE', #106337, .T. ) ;
#58268 = DIRECTION ( 'NONE',  ( 0.000000000000000000, 0.000000000000000000, 1.000000000000000000 ) ) ;
#58269 = DIRECTION ( 'NONE',  ( 0.000000000000000000, -0.9999939076577903929, 0.003490651415223739937 ) ) ;
#58270 = DIRECTION ( 'NONE',  ( 0.000000000000000000, 0.000000000000000000, 1.000000000000000000 ) ) ;
#58271 = CONICAL_SURFACE ( 'NONE', #95828, 0.1000000000000002554, 0.003490658503988666988 ) ;
#58272 = ORIENTED_EDGE ( 'NONE', *, *, #66933, .T. ) ;
#58273 = DIRECTION ( 'NONE',  ( -4.274815082592931898E-19, -0.9999939076577903929, -0.003490651415223739937 ) ) ;
#58274 = CARTESIAN_POINT ( 'NONE',  ( 11.44999999999991047, 12.50000000000000000, -2.511473670974877948 ) ) ;
#58275 = LINE ( 'NONE', #49106, #71817 ) ;
#58276 = FACE_OUTER_BOUND ( 'NONE', #4600, .T. ) ;
#58277 = ORIENTED_EDGE ( 'NONE', *, *, #88739, .F. ) ;
#58278 = FACE_OUTER_BOUND ( 'NONE', #85378, .T. ) ;
#58279 = VECTOR ( 'NONE', #88310, 1000.000000000000000 ) ;
#58280 = VECTOR ( 'NONE', #16320, 1000.000000000000000 ) ;
#58281 = DIRECTION ( 'NONE',  ( -0.000000000000000000, 1.000000000000000000, -0.000000000000000000 ) ) ;
#58282 = AXIS2_PLACEMENT_3D ( 'NONE', #104541, #54783, #86162 ) ;
#58283 = ORIENTED_EDGE ( 'NONE', *, *, #102641, .T. ) ;
#58284 = EDGE_LOOP ( 'NONE', ( #1223, #117273, #65997, #48955 ) ) ;
#58285 = LINE ( 'NONE', #97545, #50190 ) ;
#58286 = DIRECTION ( 'NONE',  ( 0.000000000000000000, 1.000000000000000000, 0.000000000000000000 ) ) ;
#58287 = FACE_BOUND ( 'NONE', #49494, .T. ) ;
#58288 = CARTESIAN_POINT ( 'NONE',  ( -1.650000000000034772, 2.500000000000000000, 5.902370205355745192 ) ) ;
#58289 = CIRCLE ( 'NONE', #118824, 0.1000000000000002554 ) ;
#58290 = CIRCLE ( 'NONE', #112659, 0.1000000000000000472 ) ;
#58291 = EDGE_CURVE ( 'NONE', #63897, #107875, #124125, .T. ) ;
#58292 = VECTOR ( 'NONE', #44993, 1000.000000000000000 ) ;
#58293 = VERTEX_POINT ( 'NONE', #101184 ) ;
#58294 = DIRECTION ( 'NONE',  ( 0.000000000000000000, 0.000000000000000000, 1.000000000000000000 ) ) ;
#58295 = ORIENTED_EDGE ( 'NONE', *, *, #92988, .F. ) ;
#58296 = EDGE_LOOP ( 'NONE', ( #128153, #2072, #97662, #116249 ) ) ;
#58297 = CARTESIAN_POINT ( 'NONE',  ( 179.5000000000000000, 0.000000000000000000, 0.000000000000000000 ) ) ;
#58298 = EDGE_CURVE ( 'NONE', #41592, #51476, #121451, .T. ) ;
#58299 = CARTESIAN_POINT ( 'NONE',  ( 186.3750000000000284, 8.891194145520236347, 5.444286225454521982E-16 ) ) ;
#58301 = ADVANCED_FACE ( 'NONE', ( #52090 ), #103202, .T. ) ;
#58300 = AXIS2_PLACEMENT_3D ( 'NONE', #49428, #77566, #6875 ) ;
#58302 = ORIENTED_EDGE ( 'NONE', *, *, #114460, .F. ) ;
#58303 = DIRECTION ( 'NONE',  ( 0.000000000000000000, -0.9999939076577903929, 0.003490651415223739937 ) ) ;
#58304 = DIRECTION ( 'NONE',  ( -1.000000000000000000, -0.000000000000000000, -0.000000000000000000 ) ) ;
#58305 = CONICAL_SURFACE ( 'NONE', #35230, 0.1000000000000000472, 0.003490658503988666988 ) ;
#58306 = EDGE_CURVE ( 'NONE', #103698, #35395, #50992, .T. ) ;
#58307 = ADVANCED_FACE ( 'NONE', ( #114851 ), #114226, .T. ) ;
#58308 = DIRECTION ( 'NONE',  ( 0.000000000000000000, -0.000000000000000000, 1.000000000000000000 ) ) ;
#58309 = ADVANCED_FACE ( 'NONE', ( #73640 ), #33968, .T. ) ;
#58310 = CARTESIAN_POINT ( 'NONE',  ( 6.249999999999930722, 12.50000000000000000, -1.407149913249512663 ) ) ;
#58311 = AXIS2_PLACEMENT_3D ( 'NONE', #81646, #28695, #68599 ) ;
#58312 = ORIENTED_EDGE ( 'NONE', *, *, #105524, .F. ) ;
#58313 = DIRECTION ( 'NONE',  ( 0.000000000000000000, 0.000000000000000000, 1.000000000000000000 ) ) ;
#58314 = EDGE_CURVE ( 'NONE', #106863, #2627, #90681, .T. ) ;
#58315 = CARTESIAN_POINT ( 'NONE',  ( -8.950000000000009948, 12.50000000000000000, 2.576566944158910744 ) ) ;
#58316 = CARTESIAN_POINT ( 'NONE',  ( 4.599999999999935696, 12.50000000000000000, 5.022947341949748790 ) ) ;
#58317 = VECTOR ( 'NONE', #97334, 1000.000000000000000 ) ;
#58318 = CARTESIAN_POINT ( 'NONE',  ( 21.24748442509682533, 0.7426088330904827561, -4.181982359507937730 ) ) ;
#58319 = VERTEX_POINT ( 'NONE', #44849 ) ;
#58320 = CARTESIAN_POINT ( 'NONE',  ( -1.050000000000038236, 12.50000000000000000, -6.213873640053564351 ) ) ;
#58321 = ORIENTED_EDGE ( 'NONE', *, *, #114840, .T. ) ;
#58322 = DIRECTION ( 'NONE',  ( 0.000000000000000000, 0.000000000000000000, -1.000000000000000000 ) ) ;
#58323 = EDGE_CURVE ( 'NONE', #27297, #106239, #101155, .T. ) ;
#58324 = ORIENTED_EDGE ( 'NONE', *, *, #12348, .F. ) ;
#58325 = CARTESIAN_POINT ( 'NONE',  ( -10.40000000000000213, 12.50000000000000000, 5.022947341949748790 ) ) ;
#58326 = DIRECTION ( 'NONE',  ( 0.000000000000000000, 1.000000000000000000, 0.000000000000000000 ) ) ;
#58327 = PLANE ( 'NONE',  #47581 ) ;
#58328 = DIRECTION ( 'NONE',  ( 0.000000000000000000, 0.000000000000000000, 1.000000000000000000 ) ) ;
#58329 = EDGE_LOOP ( 'NONE', ( #65228, #1706 ) ) ;
#58330 = VECTOR ( 'NONE', #90722, 1000.000000000000000 ) ;
#58331 = CARTESIAN_POINT ( 'NONE',  ( 0.4499999999999573785, 12.50000000000000000, -6.430097255199264339 ) ) ;
#58332 = DIRECTION ( 'NONE',  ( 0.000000000000000000, -0.9999939076577903929, 0.003490651415223739937 ) ) ;
#58333 = DIRECTION ( 'NONE',  ( 0.000000000000000000, 0.000000000000000000, -1.000000000000000000 ) ) ;
#58334 = CARTESIAN_POINT ( 'NONE',  ( 185.4010416670080872, -4.367472073101520635, 7.564683531249999149 ) ) ;
#58335 = FACE_OUTER_BOUND ( 'NONE', #11028, .T. ) ;
#58336 = AXIS2_PLACEMENT_3D ( 'NONE', #17256, #57215, #17932 ) ;
#58337 = CARTESIAN_POINT ( 'NONE',  ( 8.349999999999919709, 2.500000000000000000, 7.188010851410848723 ) ) ;
#58339 = VERTEX_POINT ( 'NONE', #14709 ) ;
#58338 = AXIS2_PLACEMENT_3D ( 'NONE', #56301, #58261, #87050 ) ;
#58340 = VERTEX_POINT ( 'NONE', #74946 ) ;
#58341 = DIRECTION ( 'NONE',  ( 0.000000000000000000, 0.000000000000000000, -1.000000000000000000 ) ) ;
#58342 = EDGE_LOOP ( 'NONE', ( #87727, #111284, #85490, #129307 ) ) ;
#58343 = CARTESIAN_POINT ( 'NONE',  ( -0.6500000000000398792, 12.50000000000000000, -6.906693963081115939 ) ) ;
#58345 = EDGE_LOOP ( 'NONE', ( #16309, #100383, #110224, #112851 ) ) ;
#58344 = EDGE_LOOP ( 'NONE', ( #70386, #33060 ) ) ;
#58346 = EDGE_LOOP ( 'NONE', ( #94924, #19026, #1082, #16597, #80886 ) ) ;
#58347 = VECTOR ( 'NONE', #72975, 1000.000000000000000 ) ;
#58348 = CARTESIAN_POINT ( 'NONE',  ( 87.49999999999998579, -2.781865847474096931, -7.000342182495692178 ) ) ;
#58349 = DIRECTION ( 'NONE',  ( 0.000000000000000000, -0.9999939076577903929, 0.003490651415223739937 ) ) ;
#58350 = FACE_OUTER_BOUND ( 'NONE', #42631, .T. ) ;
#58352 = CIRCLE ( 'NONE', #49945, 0.1000000000000002554 ) ;
#58351 = AXIS2_PLACEMENT_3D ( 'NONE', #22337, #62259, #13120 ) ;
#58353 = FACE_OUTER_BOUND ( 'NONE', #94244, .T. ) ;
#58354 = CARTESIAN_POINT ( 'NONE',  ( 1.699999999999950218, 2.500000000000000000, 4.330127018922196314 ) ) ;
#58355 = DIRECTION ( 'NONE',  ( -0.000000000000000000, -1.000000000000000000, -0.000000000000000000 ) ) ;
#58356 = FACE_OUTER_BOUND ( 'NONE', #73940, .T. ) ;
#58357 = AXIS2_PLACEMENT_3D ( 'NONE', #119453, #89371, #80199 ) ;
#58358 = DIRECTION ( 'NONE',  ( 0.000000000000000000, 0.000000000000000000, 1.000000000000000000 ) ) ;
#58359 = EDGE_LOOP ( 'NONE', ( #89414, #75549, #27740, #85996 ) ) ;
#58361 = CIRCLE ( 'NONE', #12364, 0.06509327318403745899 ) ;
#58360 = AXIS2_PLACEMENT_3D ( 'NONE', #114373, #94736, #3153 ) ;
#58362 = EDGE_LOOP ( 'NONE', ( #123957, #29599 ) ) ;
#58363 = EDGE_CURVE ( 'NONE', #52693, #23243, #44726, .T. ) ;
#58364 = VERTEX_POINT ( 'NONE', #64469 ) ;
#58365 = CARTESIAN_POINT ( 'NONE',  ( -3.350000000000029399, 2.500000000000000000, 6.495190528383297135 ) ) ;
#58366 = ORIENTED_EDGE ( 'NONE', *, *, #9962, .T. ) ;
#58367 = EDGE_LOOP ( 'NONE', ( #117104, #112069, #109473, #1302 ) ) ;
#58368 = CARTESIAN_POINT ( 'NONE',  ( -9.600000000000006750, 2.500000000000000000, 0.5928203230275495006 ) ) ;
#58369 = EDGE_CURVE ( 'NONE', #42274, #120872, #92748, .T. ) ;
#58370 = CARTESIAN_POINT ( 'NONE',  ( -11.84999999999999787, 12.50000000000000000, -2.576566944158911188 ) ) ;
#58371 = DIRECTION ( 'NONE',  ( -0.000000000000000000, -1.000000000000000000, -0.000000000000000000 ) ) ;
#58372 = DIRECTION ( 'NONE',  ( 0.000000000000000000, 1.000000000000000000, 0.000000000000000000 ) ) ;
#58373 = DIRECTION ( 'NONE',  ( 0.000000000000000000, -0.000000000000000000, 1.000000000000000000 ) ) ;
#58374 = MANIFOLD_SOLID_BREP ( 'Boss-Extrude4', #45697 ) ;
#58375 = DIRECTION ( 'NONE',  ( 0.000000000000000000, 1.000000000000000000, 0.000000000000000000 ) ) ;
#58376 = EDGE_LOOP ( 'NONE', ( #61604, #83542 ) ) ;
#58377 = DIRECTION ( 'NONE',  ( 0.000000000000000000, 0.000000000000000000, 1.000000000000000000 ) ) ;
#58378 = EDGE_LOOP ( 'NONE', ( #96971, #8413, #112094, #99577 ) ) ;
#58380 = DIRECTION ( 'NONE',  ( -0.000000000000000000, 1.000000000000000000, -0.000000000000000000 ) ) ;
#58379 = AXIS2_PLACEMENT_3D ( 'NONE', #75134, #24103, #74491 ) ;
#58382 = EDGE_LOOP ( 'NONE', ( #47935, #59491, #48619, #30762 ) ) ;
#58381 = VECTOR ( 'NONE', #81702, 1000.000000000000000 ) ;
#58383 = CARTESIAN_POINT ( 'NONE',  ( 8.549999999999922551, 2.500000000000000000, -6.148780366869526226 ) ) ;
#58384 = ORIENTED_EDGE ( 'NONE', *, *, #54088, .F. ) ;
#58385 = B_SPLINE_CURVE_WITH_KNOTS ( 'NONE', 3,
 ( #52537, #4069, #125145, #32924, #64918, #112110, #93118, #42750 ),
 .UNSPECIFIED., .F., .F.,
 ( 4, 2, 2, 4 ),
 ( -0.0001155885022056226470, 0.03307027595370837236, 0.04966320818166537060, 0.06625614040962236884 ),
 .UNSPECIFIED. ) ;
#58386 = EDGE_LOOP ( 'NONE', ( #79191, #55361 ) ) ;
#58388 = AXIS2_PLACEMENT_3D ( 'NONE', #37622, #55323, #77525 ) ;
#58387 = PLANE ( 'NONE',  #52375 ) ;
#58389 = CARTESIAN_POINT ( 'NONE',  ( 32.25969448929755856, -3.190781364619325267, -3.146220011503478631 ) ) ;
#58390 = AXIS2_PLACEMENT_3D ( 'NONE', #97950, #76390, #107112 ) ;
#58391 = AXIS2_PLACEMENT_3D ( 'NONE', #53025, #123054, #41923 ) ;
#58392 = LINE ( 'NONE', #37460, #86516 ) ;
#58393 = DIRECTION ( 'NONE',  ( 0.000000000000000000, 0.000000000000000000, 1.000000000000000000 ) ) ;
#58394 = ORIENTED_EDGE ( 'NONE', *, *, #49867, .T. ) ;
#58395 = CARTESIAN_POINT ( 'NONE',  ( 1.449999999999951328, 2.500000000000000000, 2.511473670974873507 ) ) ;
#58396 = CARTESIAN_POINT ( 'NONE',  ( 4.999999999999936939, 2.500000000000000000, -0.6928203230275541413 ) ) ;
#58397 = CARTESIAN_POINT ( 'NONE',  ( -9.150000000000009237, 2.500000000000000000, -6.595190528383296780 ) ) ;
#58398 = CARTESIAN_POINT ( 'NONE',  ( 4.149999999999941735, 12.50000000000000000, -2.857883832488653741 ) ) ;
#58399 = VECTOR ( 'NONE', #47333, 1000.000000000000000 ) ;
#58400 = DIRECTION ( 'NONE',  ( -0.000000000000000000, -1.000000000000000000, -0.000000000000000000 ) ) ;
#58402 = EDGE_CURVE ( 'NONE', #81742, #17997, #27683, .T. ) ;
#58401 = VECTOR ( 'NONE', #54202, 1000.000000000000000 ) ;
#58403 = VERTEX_POINT ( 'NONE', #85406 ) ;
#58404 = ORIENTED_EDGE ( 'NONE', *, *, #15699, .T. ) ;
#58405 = CARTESIAN_POINT ( 'NONE',  ( -6.450000000000017941, 2.500000000000000000, -2.511473670974877948 ) ) ;
#58406 = ORIENTED_EDGE ( 'NONE', *, *, #124593, .T. ) ;
#58407 = CARTESIAN_POINT ( 'NONE',  ( -12.29999999999999716, 2.500000000000000000, 0.3464101615137776813 ) ) ;
#58409 = EDGE_CURVE ( 'NONE', #112496, #72606, #125334, .T. ) ;
#58408 = DIRECTION ( 'NONE',  ( 0.000000000000000000, -0.000000000000000000, 1.000000000000000000 ) ) ;
#58410 = CIRCLE ( 'NONE', #1942, 3.000000000000000000 ) ;
#58412 = VERTEX_POINT ( 'NONE', #61023 ) ;
#58411 = EDGE_CURVE ( 'NONE', #90074, #113119, #105049, .T. ) ;
#58413 = CARTESIAN_POINT ( 'NONE',  ( 184.6666666666666856, -6.668395609140176816, -3.850000000000003642 ) ) ;
#58414 = FACE_OUTER_BOUND ( 'NONE', #82339, .T. ) ;
#58415 = SURFACE_STYLE_FILL_AREA ( #127777 ) ;
#58416 = EDGE_CURVE ( 'NONE', #6453, #98508, #109263, .T. ) ;
#58417 = DIRECTION ( 'NONE',  ( 0.000000000000000000, 0.000000000000000000, 1.000000000000000000 ) ) ;
#58418 = EDGE_LOOP ( 'NONE', ( #99868, #22387, #36515, #119652 ) ) ;
#58419 = CARTESIAN_POINT ( 'NONE',  ( 4.149999999999939959, 12.50000000000000000, -6.495190528383302464 ) ) ;
#58420 = EDGE_CURVE ( 'NONE', #121861, #5978, #34065, .T. ) ;
#58421 = ORIENTED_EDGE ( 'NONE', *, *, #55734, .F. ) ;
#58422 = ADVANCED_FACE ( 'NONE', ( #42708 ), #2641, .T. ) ;
#58423 = CARTESIAN_POINT ( 'NONE',  ( 3.749999999999938716, 2.500000000000000000, 7.288010851410849256 ) ) ;
#58424 = CIRCLE ( 'NONE', #37495, 0.1000000000000002554 ) ;
#58425 = DIRECTION ( 'NONE',  ( -0.000000000000000000, -1.000000000000000000, -0.000000000000000000 ) ) ;
#58426 = DIRECTION ( 'NONE',  ( 0.000000000000000000, 0.000000000000000000, -1.000000000000000000 ) ) ;
#58427 = ORIENTED_EDGE ( 'NONE', *, *, #67291, .T. ) ;
#58428 = CARTESIAN_POINT ( 'NONE',  ( -4.150000000000024336, 2.500000000000000000, -2.065063509461102065 ) ) ;
#58429 = ORIENTED_EDGE ( 'NONE', *, *, #46893, .T. ) ;
#58431 = CONICAL_SURFACE ( 'NONE', #116887, 0.1000000000000002554, 0.003490658503988666988 ) ;
#58430 = DIRECTION ( 'NONE',  ( 0.000000000000000000, 1.000000000000000000, 0.000000000000000000 ) ) ;
#58432 = CARTESIAN_POINT ( 'NONE',  ( -8.750000000000005329, 12.50000000000000000, 5.802370205355744659 ) ) ;
#58433 = FACE_OUTER_BOUND ( 'NONE', #28724, .T. ) ;
#58434 = ORIENTED_EDGE ( 'NONE', *, *, #48127, .T. ) ;
#58435 = DIRECTION ( 'NONE',  ( 0.000000000000000000, 1.000000000000000000, 0.000000000000000000 ) ) ;
#58437 = CIRCLE ( 'NONE', #106446, 0.06509327318403745899 ) ;
#58436 = CONICAL_SURFACE ( 'NONE', #98122, 0.1000000000000000472, 0.003490658503988666988 ) ;
#58438 = CARTESIAN_POINT ( 'NONE',  ( 185.5312500006828031, 9.429780353434619030E-16, -7.700000000000000178 ) ) ;
#58439 = VECTOR ( 'NONE', #38856, 1000.000000000000000 ) ;
#58440 = VERTEX_POINT ( 'NONE', #80682 ) ;
#58441 = CARTESIAN_POINT ( 'NONE',  ( -8.300000000000011369, 12.50000000000000000, -2.276824562219559311E-15 ) ) ;
#58442 = EDGE_LOOP ( 'NONE', ( #32008, #52246 ) ) ;
#58443 = FACE_OUTER_BOUND ( 'NONE', #71934, .T. ) ;
#58445 = CIRCLE ( 'NONE', #22756, 0.09999999999999999167 ) ;
#58444 = AXIS2_PLACEMENT_3D ( 'NONE', #70444, #101195, #59355 ) ;
#58446 = EDGE_CURVE ( 'NONE', #55057, #59725, #113342, .T. ) ;
#58447 = ORIENTED_EDGE ( 'NONE', *, *, #97095, .F. ) ;
#58448 = DIRECTION ( 'NONE',  ( 0.000000000000000000, 0.000000000000000000, 1.000000000000000000 ) ) ;
#58449 = DIRECTION ( 'NONE',  ( 0.000000000000000000, 0.000000000000000000, 1.000000000000000000 ) ) ;
#58450 = ORIENTED_EDGE ( 'NONE', *, *, #98470, .F. ) ;
#58451 = VERTEX_POINT ( 'NONE', #72149 ) ;
#58452 = CARTESIAN_POINT ( 'NONE',  ( 9.149999999999916866, 12.50000000000000000, 5.737276932171707422 ) ) ;
#58453 = FACE_OUTER_BOUND ( 'NONE', #103207, .T. ) ;
#58454 = ORIENTED_EDGE ( 'NONE', *, *, #102074, .F. ) ;
#58455 = ADVANCED_FACE ( 'NONE', ( #30943 ), #4689, .T. ) ;
#58456 = CARTESIAN_POINT ( 'NONE',  ( -12.29999999999999716, 2.500000000000000000, -3.883716857408423984 ) ) ;
#58457 = CARTESIAN_POINT ( 'NONE',  ( 186.6927083336747160, 6.551208109652275624, -3.782341765624998686 ) ) ;
#58458 = CARTESIAN_POINT ( 'NONE',  ( 9.149999999999916866, 12.50000000000000000, -2.792790559304616504 ) ) ;
#58459 = FACE_OUTER_BOUND ( 'NONE', #60758, .T. ) ;
#58460 = AXIS2_PLACEMENT_3D ( 'NONE', #52027, #93239, #123336 ) ;
#58461 = PLANE ( 'NONE',  #82273 ) ;
#58462 = EDGE_CURVE ( 'NONE', #119461, #37781, #77862, .T. ) ;
#58463 = CARTESIAN_POINT ( 'NONE',  ( -11.84999999999999787, 2.500000000000000000, -2.511473670974873951 ) ) ;
#58464 = DIRECTION ( 'NONE',  ( 0.000000000000000000, 0.000000000000000000, 1.000000000000000000 ) ) ;
#58465 = EDGE_CURVE ( 'NONE', #34821, #83361, #75806, .T. ) ;
#58466 = EDGE_CURVE ( 'NONE', #81614, #126271, #111300, .T. ) ;
#58467 = AXIS2_PLACEMENT_3D ( 'NONE', #118761, #10715, #80136 ) ;
#58468 = CONICAL_SURFACE ( 'NONE', #60536, 0.09999999999999982514, 0.003490658503988666988 ) ;
#58469 = ORIENTED_EDGE ( 'NONE', *, *, #61409, .F. ) ;
#58470 = ORIENTED_EDGE ( 'NONE', *, *, #38257, .F. ) ;
#58472 = VERTEX_POINT ( 'NONE', #100940 ) ;
#58471 = EDGE_CURVE ( 'NONE', #87106, #127915, #100846, .T. ) ;
#58473 = ORIENTED_EDGE ( 'NONE', *, *, #95725, .T. ) ;
#58474 = DIRECTION ( 'NONE',  ( -4.274815082592931898E-19, -0.9999939076577903929, -0.003490651415223739937 ) ) ;
#58475 = DIRECTION ( 'NONE',  ( 0.000000000000000000, 0.000000000000000000, 1.000000000000000000 ) ) ;
#58476 = DIRECTION ( 'NONE',  ( 0.000000000000000000, 1.000000000000000000, 0.000000000000000000 ) ) ;
#58477 = ORIENTED_EDGE ( 'NONE', *, *, #26952, .T. ) ;
#58478 = FACE_BOUND ( 'NONE', #47118, .T. ) ;
#58479 = ORIENTED_EDGE ( 'NONE', *, *, #8107, .T. ) ;
#58480 = CARTESIAN_POINT ( 'NONE',  ( -14.19999999999998685, 2.500000000000000000, -1.084202172485504434E-16 ) ) ;
#58481 = CARTESIAN_POINT ( 'NONE',  ( -12.29999999999999538, 2.500000000000000000, -4.576537180435975571 ) ) ;
#58482 = AXIS2_PLACEMENT_3D ( 'NONE', #83347, #31658, #13285 ) ;
#58484 = EDGE_CURVE ( 'NONE', #111766, #82690, #92538, .T. ) ;
#58483 = VECTOR ( 'NONE', #54017, 1000.000000000000000 ) ;
#58485 = DIRECTION ( 'NONE',  ( -1.000000000000000000, -0.000000000000000000, -0.000000000000000000 ) ) ;
#58486 = CIRCLE ( 'NONE', #93971, 0.1000000000000002554 ) ;
#58487 = EDGE_CURVE ( 'NONE', #91091, #37483, #54880, .T. ) ;
#58488 = DIRECTION ( 'NONE',  ( -0.000000000000000000, -1.000000000000000000, -0.000000000000000000 ) ) ;
#58489 = DIRECTION ( 'NONE',  ( 0.000000000000000000, 1.000000000000000000, 0.000000000000000000 ) ) ;
#58490 = CARTESIAN_POINT ( 'NONE',  ( 127.5000000000000000, -5.000000000000000000, -1.999999999999998224 ) ) ;
#58491 = PLANE ( 'NONE',  #106332 ) ;
#58492 = CARTESIAN_POINT ( 'NONE',  ( -1.850000000000033840, 2.500000000000000000, 2.611473670974873151 ) ) ;
#58493 = CARTESIAN_POINT ( 'NONE',  ( -0.6000000000000388356, 12.50000000000000000, 3.918623584224383727 ) ) ;
#58494 = CIRCLE ( 'NONE', #2025, 0.09999999999999982514 ) ;
#58495 = CARTESIAN_POINT ( 'NONE',  ( 4.349999999999940137, 2.500000000000000000, -6.841600689897078702 ) ) ;
#58496 = VECTOR ( 'NONE', #127927, 1000.000000000000000 ) ;
#58497 = VERTEX_POINT ( 'NONE', #1453 ) ;
#58498 = ORIENTED_EDGE ( 'NONE', *, *, #8048, .T. ) ;
#58499 = VECTOR ( 'NONE', #113464, 1000.000000000000000 ) ;
#58500 = ORIENTED_EDGE ( 'NONE', *, *, #113906, .F. ) ;
#58501 = ORIENTED_EDGE ( 'NONE', *, *, #39014, .F. ) ;
#58502 = CARTESIAN_POINT ( 'NONE',  ( 4.999999999999973355, 2.500000000000000000, -4.330127018922201643 ) ) ;
#58503 = CARTESIAN_POINT ( 'NONE',  ( -1.650000000000035216, 12.50000000000000000, -5.867463478539787225 ) ) ;
#58505 = ORIENTED_EDGE ( 'NONE', *, *, #37481, .T. ) ;
#58504 = VERTEX_POINT ( 'NONE', #41408 ) ;
#58506 = EDGE_LOOP ( 'NONE', ( #5849, #4295 ) ) ;
#58507 = PLANE ( 'NONE',  #31322 ) ;
#58508 = CIRCLE ( 'NONE', #73155, 0.06509327318403745899 ) ;
#58509 = DIRECTION ( 'NONE',  ( 0.000000000000000000, 0.000000000000000000, 1.000000000000000000 ) ) ;
#58510 = DIRECTION ( 'NONE',  ( 0.000000000000000000, 0.000000000000000000, 1.000000000000000000 ) ) ;
#58511 = DIRECTION ( 'NONE',  ( -4.274815082592931898E-19, -0.9999939076577903929, -0.003490651415223739937 ) ) ;
#58512 = FACE_OUTER_BOUND ( 'NONE', #93756, .T. ) ;
#58513 = AXIS2_PLACEMENT_3D ( 'NONE', #15751, #113320, #55689 ) ;
#58514 = DIRECTION ( 'NONE',  ( 0.000000000000000000, 0.000000000000000000, 1.000000000000000000 ) ) ;
#58515 = FACE_OUTER_BOUND ( 'NONE', #98533, .T. ) ;
#58516 = VERTEX_POINT ( 'NONE', #32239 ) ;
#58517 = DIRECTION ( 'NONE',  ( 0.000000000000000000, 0.000000000000000000, 1.000000000000000000 ) ) ;
#58518 = EDGE_LOOP ( 'NONE', ( #85163, #128732, #38890, #88269 ) ) ;
#58519 = ORIENTED_EDGE ( 'NONE', *, *, #123900, .F. ) ;
#58520 = ORIENTED_EDGE ( 'NONE', *, *, #20437, .T. ) ;
#58521 = CARTESIAN_POINT ( 'NONE',  ( -7.900000000000014566, 12.50000000000000000, -2.276824562219559311E-15 ) ) ;
#58522 = ORIENTED_EDGE ( 'NONE', *, *, #124943, .T. ) ;
#58523 = ORIENTED_EDGE ( 'NONE', *, *, #15969, .T. ) ;
#58524 = DIRECTION ( 'NONE',  ( 0.000000000000000000, 1.000000000000000000, 0.000000000000000000 ) ) ;
#58525 = EDGE_CURVE ( 'NONE', #120418, #93687, #23041, .T. ) ;
#58526 = DIRECTION ( 'NONE',  ( -0.000000000000000000, 1.000000000000000000, -0.000000000000000000 ) ) ;
#58527 = CARTESIAN_POINT ( 'NONE',  ( -2.700000000000030820, 2.500000000000000000, -3.883716857408426648 ) ) ;
#58528 = CARTESIAN_POINT ( 'NONE',  ( -10.00000000000000533, 12.50000000000000000, 0.6928203230275494784 ) ) ;
#58529 = DIRECTION ( 'NONE',  ( 0.000000000000000000, 1.000000000000000000, 0.000000000000000000 ) ) ;
#58530 = ORIENTED_EDGE ( 'NONE', *, *, #92568, .F. ) ;
#58531 = DIRECTION ( 'NONE',  ( 0.000000000000000000, 0.000000000000000000, -1.000000000000000000 ) ) ;
#58532 = EDGE_LOOP ( 'NONE', ( #12419, #95135, #82796, #61007 ) ) ;
#58533 = DIRECTION ( 'NONE',  ( 0.000000000000000000, 1.000000000000000000, 0.000000000000000000 ) ) ;
#58535 = AXIS2_PLACEMENT_3D ( 'NONE', #115556, #6245, #57309 ) ;
#58534 = CIRCLE ( 'NONE', #73187, 0.06509327318403741736 ) ;
#58536 = ORIENTED_EDGE ( 'NONE', *, *, #5210, .F. ) ;
#58537 = CARTESIAN_POINT ( 'NONE',  ( 112.6717552496036205, 8.515422928616107612, 1.789336338813789506 ) ) ;
#58538 = FACE_OUTER_BOUND ( 'NONE', #52370, .T. ) ;
#58539 = ORIENTED_EDGE ( 'NONE', *, *, #8141, .F. ) ;
#58540 = CARTESIAN_POINT ( 'NONE',  ( 11.04999999999990656, 2.500000000000000000, 2.511473670974873507 ) ) ;
#58541 = CARTESIAN_POINT ( 'NONE',  ( 15.59999999999988951, 2.500000000000000000, 0.4464101615137735513 ) ) ;
#58542 = ORIENTED_EDGE ( 'NONE', *, *, #89787, .T. ) ;
#58544 = CIRCLE ( 'NONE', #29289, 0.1000000000000002554 ) ;
#58543 = AXIS2_PLACEMENT_3D ( 'NONE', #5404, #27607, #45351 ) ;
#58545 = DIRECTION ( 'NONE',  ( 0.000000000000000000, 0.000000000000000000, -1.000000000000000000 ) ) ;
#58546 = EDGE_LOOP ( 'NONE', ( #113802, #90092 ) ) ;
#58547 = EDGE_LOOP ( 'NONE', ( #108306, #60306, #10630, #76396 ) ) ;
#58548 = DIRECTION ( 'NONE',  ( 0.000000000000000000, 0.000000000000000000, 1.000000000000000000 ) ) ;
#58549 = DIRECTION ( 'NONE',  ( 0.000000000000000000, 1.000000000000000000, 0.000000000000000000 ) ) ;
#58550 = CARTESIAN_POINT ( 'NONE',  ( 184.1510416670080588, 4.367472073101518859, -7.564683531249999149 ) ) ;
#58551 = FACE_OUTER_BOUND ( 'NONE', #99879, .T. ) ;
#58552 = DIRECTION ( 'NONE',  ( -0.8660254037844390407, 0.000000000000000000, -0.4999999999999991673 ) ) ;
#58553 = CARTESIAN_POINT ( 'NONE',  ( 184.2812500006828031, 0.000000000000000000, 7.700000000000000178 ) ) ;
#58554 = ORIENTED_EDGE ( 'NONE', *, *, #98644, .F. ) ;
#58555 = DIRECTION ( 'NONE',  ( 0.000000000000000000, -0.9999939076577903929, 0.003490651415223739937 ) ) ;
#58556 = AXIS2_PLACEMENT_3D ( 'NONE', #103420, #74599, #114510 ) ;
#58558 = EDGE_CURVE ( 'NONE', #91215, #123206, #107206, .T. ) ;
#58557 = CARTESIAN_POINT ( 'NONE',  ( 8.749999999999957367, 2.500000000000000000, 2.265063509461097357 ) ) ;
#58559 = AXIS2_PLACEMENT_3D ( 'NONE', #55258, #115429, #56527 ) ;
#58560 = ORIENTED_EDGE ( 'NONE', *, *, #118278, .F. ) ;
#58561 = ADVANCED_FACE ( 'NONE', ( #71484 ), #61691, .T. ) ;
#58562 = CARTESIAN_POINT ( 'NONE',  ( 6.849999999999929479, 2.500000000000000000, 6.741600689897071952 ) ) ;
#58563 = DIRECTION ( 'NONE',  ( 0.000000000000000000, -0.9999939076577903929, 0.003490651415223739937 ) ) ;
#58564 = CARTESIAN_POINT ( 'NONE',  ( -14.54999999999998472, 2.500000000000000000, -2.065063509461099844 ) ) ;
#58565 = DIRECTION ( 'NONE',  ( 0.000000000000000000, 0.000000000000000000, 1.000000000000000000 ) ) ;
#58566 = EDGE_CURVE ( 'NONE', #116432, #102156, #44423, .T. ) ;
#58567 = CARTESIAN_POINT ( 'NONE',  ( 5.399999999999931966, 2.500000000000000000, 4.230127018922196669 ) ) ;
#58568 = EDGE_LOOP ( 'NONE', ( #76627, #127642, #127510, #57970 ) ) ;
#58569 = AXIS2_PLACEMENT_3D ( 'NONE', #3201, #116349, #127475 ) ;
#58570 = FACE_OUTER_BOUND ( 'NONE', #18158, .T. ) ;
#58571 = PLANE ( 'NONE',  #83098 ) ;
#58572 = EDGE_CURVE ( 'NONE', #72837, #62517, #102249, .T. ) ;
#58573 = EDGE_CURVE ( 'NONE', #63390, #128977, #53151, .T. ) ;
#58574 = EDGE_CURVE ( 'NONE', #96204, #83685, #52836, .T. ) ;
#58575 = AXIS2_PLACEMENT_3D ( 'NONE', #60074, #109804, #48958 ) ;
#58576 = EDGE_LOOP ( 'NONE', ( #31329, #25101 ) ) ;
#58577 = CARTESIAN_POINT ( 'NONE',  ( 17.50000000000000000, 2.500000000000000000, -3.999999999999996447 ) ) ;
#58578 = CONICAL_SURFACE ( 'NONE', #71088, 0.1000000000000002554, 0.003490658503988666988 ) ;
#58579 = AXIS2_PLACEMENT_3D ( 'NONE', #21717, #72749, #41373 ) ;
#58580 = EDGE_LOOP ( 'NONE', ( #47830, #128194 ) ) ;
#58581 = ORIENTED_EDGE ( 'NONE', *, *, #56075, .F. ) ;
#58582 = DIRECTION ( 'NONE',  ( 0.000000000000000000, 0.000000000000000000, 1.000000000000000000 ) ) ;
#58583 = ORIENTED_EDGE ( 'NONE', *, *, #108766, .F. ) ;
#58584 = DIRECTION ( 'NONE',  ( 0.000000000000000000, -0.000000000000000000, 1.000000000000000000 ) ) ;
#58585 = DIRECTION ( 'NONE',  ( -4.274815082592931898E-19, -0.9999939076577903929, -0.003490651415223739937 ) ) ;
#58586 = CIRCLE ( 'NONE', #56504, 0.06509327318403745899 ) ;
#58587 = EDGE_LOOP ( 'NONE', ( #78098, #88575, #100167, #91245 ) ) ;
#58588 = DIRECTION ( 'NONE',  ( 0.000000000000000000, -0.000000000000000000, 1.000000000000000000 ) ) ;
#58590 = EDGE_LOOP ( 'NONE', ( #95059, #74950, #48129, #126866 ) ) ;
#58589 = DIRECTION ( 'NONE',  ( 0.000000000000000000, 0.000000000000000000, -1.000000000000000000 ) ) ;
#58591 = DIRECTION ( 'NONE',  ( -0.000000000000000000, -1.000000000000000000, -0.000000000000000000 ) ) ;
#58592 = CARTESIAN_POINT ( 'NONE',  ( -6.650000000000015454, 2.500000000000000000, 2.957883832488649389 ) ) ;
#58593 = ORIENTED_EDGE ( 'NONE', *, *, #26028, .T. ) ;
#58594 = VERTEX_POINT ( 'NONE', #95008 ) ;
#58595 = EDGE_LOOP ( 'NONE', ( #103281, #7105, #30910, #51157 ) ) ;
#58596 = DIRECTION ( 'NONE',  ( 0.000000000000000000, -0.000000000000000000, 1.000000000000000000 ) ) ;
#58597 = CARTESIAN_POINT ( 'NONE',  ( 3.749999999999978684, 2.500000000000000000, -6.395190528383301931 ) ) ;
#58598 =( BOUNDED_SURFACE ( )  B_SPLINE_SURFACE ( 3, 2, ( 
 ( #74458, #3783, #62714 ),
 ( #93449, #3146, #114368 ),
 ( #31966, #54179, #53536 ),
 ( #4390, #2472, #33265 ),
 ( #101990, #51607, #71891 ),
 ( #43731, #102614, #12935 ),
 ( #91517, #12300, #63990 ),
 ( #73797, #1838, #41798 ),
 ( #52885, #84261, #33880 ),
 ( #14227, #43092, #81690 ),
 ( #73170, #83002, #52244 ),
 ( #113081, #123539, #92154 ) ),
 .UNSPECIFIED., .F., .F., .F. ) 
 B_SPLINE_SURFACE_WITH_KNOTS ( ( 4, 2, 2, 2, 2, 4 ),
 ( 3, 3 ),
 ( -5.075233897207043562E-05, 0.01652955890749042978, 0.03310987015395293331, 0.04969018140041543685, 0.05798033702364668862, 0.06627049264687794039 ),
 ( 0.000000000000000000, 1.000000000000000000 ),
 .UNSPECIFIED. ) 
 GEOMETRIC_REPRESENTATION_ITEM ( )  RATIONAL_B_SPLINE_SURFACE ( (
 ( 1.000000000000000000, 1.000000000000000000, 1.000000000000000000),
 ( 1.000000000000000000, 0.9999962913205889814, 1.000000000000000000),
 ( 1.000000000000000000, 0.9967432547768471096, 1.000000000000000000),
 ( 1.000000000000000000, 0.9780629203666471039, 1.000000000000000000),
 ( 1.000000000000000000, 0.9624374449462932413, 1.000000000000000000),
 ( 1.000000000000000000, 0.9156028756791357859, 1.000000000000000000),
 ( 1.000000000000000000, 0.8842425819005229615, 1.000000000000000000),
 ( 1.000000000000000000, 0.8293059173955059649, 1.000000000000000000),
 ( 1.000000000000000000, 0.8097380764758507210, 1.000000000000000000),
 ( 1.000000000000000000, 0.7702514575403359709, 1.000000000000000000),
 ( 1.000000000000000000, 0.7503390841289654389, 1.000000000000000000),
 ( 1.000000000000000000, 0.7318752858502187708, 1.000000000000000000) ) ) 
 REPRESENTATION_ITEM ( '' )  SURFACE ( )  );
#58599 = CARTESIAN_POINT ( 'NONE',  ( 15.39999999999989022, 2.500000000000000000, -0.1000000000000023925 ) ) ;
#58600 = EDGE_CURVE ( 'NONE', #84391, #85395, #85809, .T. ) ;
#58601 = FACE_BOUND ( 'NONE', #108346, .T. ) ;
#58602 = ORIENTED_EDGE ( 'NONE', *, *, #90615, .T. ) ;
#58603 = DIRECTION ( 'NONE',  ( 0.000000000000000000, 1.000000000000000000, 0.000000000000000000 ) ) ;
#58604 = CARTESIAN_POINT ( 'NONE',  ( 3.149999999999944400, 2.500000000000000000, 1.818653347947321475 ) ) ;
#58605 = ORIENTED_EDGE ( 'NONE', *, *, #67880, .T. ) ;
#58606 = CARTESIAN_POINT ( 'NONE',  ( 105.6184301395928031, 8.500000000000000000, 1.375000000000001110 ) ) ;
#58607 = DIRECTION ( 'NONE',  ( 0.000000000000000000, 0.000000000000000000, 1.000000000000000000 ) ) ;
#58610 = EDGE_CURVE ( 'NONE', #19273, #56340, #63297, .T. ) ;
#58609 = CARTESIAN_POINT ( 'NONE',  ( -6.050000000000017586, 2.500000000000000000, 1.818653347947321475 ) ) ;
#58608 = AXIS2_PLACEMENT_3D ( 'NONE', #67159, #119508, #127408 ) ;
#58611 = FACE_OUTER_BOUND ( 'NONE', #81349, .T. ) ;
#58612 = DIRECTION ( 'NONE',  ( 0.000000000000000000, 1.000000000000000000, 0.000000000000000000 ) ) ;
#58613 = EDGE_CURVE ( 'NONE', #67849, #118985, #46528, .T. ) ;
#58614 = DIRECTION ( 'NONE',  ( 0.000000000000000000, 1.000000000000000000, 0.000000000000000000 ) ) ;
#58615 = DIRECTION ( 'NONE',  ( 0.000000000000000000, 0.000000000000000000, -1.000000000000000000 ) ) ;
#58616 = EDGE_CURVE ( 'NONE', #80402, #48868, #45264, .T. ) ;
#58618 = CONICAL_SURFACE ( 'NONE', #60677, 0.1000000000000002554, 0.003490658503988666988 ) ;
#58617 = AXIS2_PLACEMENT_3D ( 'NONE', #101052, #19252, #42139 ) ;
#58619 = ORIENTED_EDGE ( 'NONE', *, *, #49201, .F. ) ;
#58620 = EDGE_LOOP ( 'NONE', ( #19423, #19696 ) ) ;
#58621 = EDGE_LOOP ( 'NONE', ( #52978, #115773 ) ) ;
#58622 = ORIENTED_EDGE ( 'NONE', *, *, #61562, .T. ) ;
#58623 = ORIENTED_EDGE ( 'NONE', *, *, #72169, .T. ) ;
#58624 = DIRECTION ( 'NONE',  ( -4.274815082592931898E-19, -0.9999939076577903929, -0.003490651415223739937 ) ) ;
#58625 = ADVANCED_FACE ( 'NONE', ( #66805 ), #40332, .T. ) ;
#58626 = CARTESIAN_POINT ( 'NONE',  ( 7.099999999999927702, 12.50000000000000000, -3.637306695894650055 ) ) ;
#58628 = EDGE_CURVE ( 'NONE', #102156, #116432, #59102, .T. ) ;
#58627 = EDGE_LOOP ( 'NONE', ( #19761, #7035 ) ) ;
#58629 = FACE_BOUND ( 'NONE', #93379, .T. ) ;
#58630 = DIRECTION ( 'NONE',  ( 0.000000000000000000, 1.000000000000000000, 0.000000000000000000 ) ) ;
#58631 = EDGE_CURVE ( 'NONE', #34514, #97550, #103000, .T. ) ;
#58632 = ADVANCED_FACE ( 'NONE', ( #76650 ), #23586, .T. ) ;
#58633 = ADVANCED_FACE ( 'NONE', ( #96921 ), #17399, .T. ) ;
#58634 = DIRECTION ( 'NONE',  ( 0.000000000000000000, 0.000000000000000000, 1.000000000000000000 ) ) ;
#58635 = DIRECTION ( 'NONE',  ( 0.000000000000000000, -0.000000000000000000, 1.000000000000000000 ) ) ;
#58636 = DIRECTION ( 'NONE',  ( -0.000000000000000000, 1.000000000000000000, -0.000000000000000000 ) ) ;
#58637 = CARTESIAN_POINT ( 'NONE',  ( 1.699999999999951994, 2.500000000000000000, -2.276824562219559311E-15 ) ) ;
#58638 = ORIENTED_EDGE ( 'NONE', *, *, #73817, .F. ) ;
#58639 = EDGE_CURVE ( 'NONE', #6619, #28229, #67476, .T. ) ;
#58640 = ORIENTED_EDGE ( 'NONE', *, *, #10432, .T. ) ;
#58641 = ORIENTED_EDGE ( 'NONE', *, *, #126862, .T. ) ;
#58642 = ORIENTED_EDGE ( 'NONE', *, *, #117960, .F. ) ;
#58643 = DIRECTION ( 'NONE',  ( 0.000000000000000000, 1.000000000000000000, 0.000000000000000000 ) ) ;
#58644 = DIRECTION ( 'NONE',  ( -0.000000000000000000, 1.000000000000000000, -0.000000000000000000 ) ) ;
#58645 = DIRECTION ( 'NONE',  ( -0.000000000000000000, -1.000000000000000000, -0.000000000000000000 ) ) ;
#58646 = ORIENTED_EDGE ( 'NONE', *, *, #86200, .T. ) ;
#58647 = DIRECTION ( 'NONE',  ( -0.000000000000000000, -1.000000000000000000, -0.000000000000000000 ) ) ;
#58648 = DIRECTION ( 'NONE',  ( 0.000000000000000000, 0.000000000000000000, 1.000000000000000000 ) ) ;
#58649 = CARTESIAN_POINT ( 'NONE',  ( -6.250000000000019540, 12.50000000000000000, -7.188010851410854052 ) ) ;
#58650 = CARTESIAN_POINT ( 'NONE',  ( 184.6510416670080588, 4.367472073101518859, -7.564683531249999149 ) ) ;
#58651 = CARTESIAN_POINT ( 'NONE',  ( 10.59999999999991260, 2.500000000000000000, -0.3464101615137783474 ) ) ;
#58652 = DIRECTION ( 'NONE',  ( 0.000000000000000000, 0.000000000000000000, -1.000000000000000000 ) ) ;
#58653 = DIRECTION ( 'NONE',  ( 0.000000000000000000, 0.000000000000000000, 1.000000000000000000 ) ) ;
#58654 = VERTEX_POINT ( 'NONE', #94341 ) ;
#58655 = DIRECTION ( 'NONE',  ( -0.000000000000000000, 1.000000000000000000, -0.000000000000000000 ) ) ;
#58656 = CONICAL_SURFACE ( 'NONE', #106748, 0.1000000000000002554, 0.003490658503988666988 ) ;
#58657 = ORIENTED_EDGE ( 'NONE', *, *, #99975, .T. ) ;
#58658 = EDGE_LOOP ( 'NONE', ( #39750, #93485 ) ) ;
#58659 = CARTESIAN_POINT ( 'NONE',  ( -5.850000000000019185, 12.50000000000000000, 2.165063509461097713 ) ) ;
#58660 = DIRECTION ( 'NONE',  ( 0.000000000000000000, 1.000000000000000000, 0.000000000000000000 ) ) ;
#58661 = CARTESIAN_POINT ( 'NONE',  ( -8.350000000000013856, 2.500000000000000000, -6.395190528383296602 ) ) ;
#58662 = VERTEX_POINT ( 'NONE', #5953 ) ;
#58663 = ORIENTED_EDGE ( 'NONE', *, *, #82565, .F. ) ;
#58664 = AXIS2_PLACEMENT_3D ( 'NONE', #126981, #96860, #124405 ) ;
#58665 = CARTESIAN_POINT ( 'NONE',  ( 12.29999999999990479, 2.500000000000000000, -3.983716857408426293 ) ) ;
#58666 = AXIS2_PLACEMENT_3D ( 'NONE', #38806, #12993, #83061 ) ;
#58667 = EDGE_CURVE ( 'NONE', #93997, #27988, #67578, .T. ) ;
#58668 = CARTESIAN_POINT ( 'NONE',  ( -8.749999999999971578, 12.50000000000000000, 6.560283801567334372 ) ) ;
#58669 = CARTESIAN_POINT ( 'NONE',  ( 2.500000000000002220, -1.500000000000000000, -9.999999999999998224 ) ) ;
#58670 = ORIENTED_EDGE ( 'NONE', *, *, #105991, .T. ) ;
#58671 = ORIENTED_EDGE ( 'NONE', *, *, #25300, .T. ) ;
#58672 = LINE ( 'NONE', #69119, #64845 ) ;
#58673 = VECTOR ( 'NONE', #106547, 1000.000000000000000 ) ;
#58674 = ORIENTED_EDGE ( 'NONE', *, *, #58002, .F. ) ;
#58675 = DIRECTION ( 'NONE',  ( -0.000000000000000000, -1.000000000000000000, -0.000000000000000000 ) ) ;
#58676 = ORIENTED_EDGE ( 'NONE', *, *, #55513, .T. ) ;
#58677 = DIRECTION ( 'NONE',  ( 0.000000000000000000, 0.000000000000000000, 1.000000000000000000 ) ) ;
#58678 = LINE ( 'NONE', #48871, #46236 ) ;
#58679 = AXIS2_PLACEMENT_3D ( 'NONE', #111215, #119768, #22877 ) ;
#58680 = CARTESIAN_POINT ( 'NONE',  ( 3.149999999999942624, 2.500000000000000000, 6.741600689897071952 ) ) ;
#58681 = ADVANCED_FACE ( 'NONE', ( #26267 ), #15245, .T. ) ;
#58682 = DIRECTION ( 'NONE',  ( 0.000000000000000000, 1.000000000000000000, 0.000000000000000000 ) ) ;
#58683 = ORIENTED_EDGE ( 'NONE', *, *, #68426, .T. ) ;
#58684 = DIRECTION ( 'NONE',  ( 0.000000000000000000, 0.000000000000000000, 1.000000000000000000 ) ) ;
#58685 = EDGE_LOOP ( 'NONE', ( #7576, #28448 ) ) ;
#58686 = ORIENTED_EDGE ( 'NONE', *, *, #103650, .T. ) ;
#58687 = CARTESIAN_POINT ( 'NONE',  ( -1.700000000000035261, 2.500000000000000000, 4.430127018922196847 ) ) ;
#58688 = DIRECTION ( 'NONE',  ( 0.000000000000000000, 0.000000000000000000, 1.000000000000000000 ) ) ;
#58689 = DIRECTION ( 'NONE',  ( 0.000000000000000000, 0.000000000000000000, 1.000000000000000000 ) ) ;
#58690 = DIRECTION ( 'NONE',  ( 0.000000000000000000, 0.000000000000000000, 1.000000000000000000 ) ) ;
#58691 = CARTESIAN_POINT ( 'NONE',  ( 0.6499999999999543920, 12.50000000000000000, 6.213873640053559022 ) ) ;
#58692 = CARTESIAN_POINT ( 'NONE',  ( -7.300000000000016698, 2.500000000000000000, -0.3464101615137783474 ) ) ;
#58693 = FACE_OUTER_BOUND ( 'NONE', #66537, .T. ) ;
#58694 = CARTESIAN_POINT ( 'NONE',  ( -8.750000000000007105, 2.500000000000000000, 7.188010851410848723 ) ) ;
#58695 = DIRECTION ( 'NONE',  ( 0.000000000000000000, 1.000000000000000000, 0.000000000000000000 ) ) ;
#58696 = AXIS2_PLACEMENT_3D ( 'NONE', #81219, #78654, #109380 ) ;
#58697 = AXIS2_PLACEMENT_3D ( 'NONE', #46607, #123869, #96338 ) ;
#58698 = CIRCLE ( 'NONE', #46164, 0.06509327318403745899 ) ;
#58699 = CARTESIAN_POINT ( 'NONE',  ( 0.6499999999999566125, 12.50000000000000000, -6.841600689897077814 ) ) ;
#58700 = EDGE_CURVE ( 'NONE', #43111, #112381, #111395, .T. ) ;
#58701 = CIRCLE ( 'NONE', #18973, 0.06509327318403745899 ) ;
#58702 = ORIENTED_EDGE ( 'NONE', *, *, #8004, .F. ) ;
#58703 = DIRECTION ( 'NONE',  ( 0.000000000000000000, -0.9999939076577903929, 0.003490651415223739937 ) ) ;
#58704 = AXIS2_PLACEMENT_3D ( 'NONE', #1019, #1654, #110331 ) ;
#58705 = CARTESIAN_POINT ( 'NONE',  ( -5.800000000000018474, 2.500000000000000000, -0.1000000000000022815 ) ) ;
#58706 = DIRECTION ( 'NONE',  ( 0.000000000000000000, 0.000000000000000000, -1.000000000000000000 ) ) ;
#58707 = DIRECTION ( 'NONE',  ( -0.000000000000000000, 1.000000000000000000, -0.000000000000000000 ) ) ;
#58708 = CARTESIAN_POINT ( 'NONE',  ( 3.749999999999942268, 2.500000000000000000, 1.472243186433545459 ) ) ;
#58709 = EDGE_CURVE ( 'NONE', #38624, #60290, #121876, .T. ) ;
#58710 = ORIENTED_EDGE ( 'NONE', *, *, #74741, .T. ) ;
#58711 = FACE_OUTER_BOUND ( 'NONE', #33992, .T. ) ;
#58712 = CARTESIAN_POINT ( 'NONE',  ( 186.5000000000000000, 0.000000000000000000, 0.000000000000000000 ) ) ;
#58714 = VERTEX_POINT ( 'NONE', #104795 ) ;
#58713 = CARTESIAN_POINT ( 'NONE',  ( -1.650000000000035216, 2.500000000000000000, -1.572243186433550211 ) ) ;
#58715 = ADVANCED_FACE ( 'NONE', ( #114004 ), #125103, .T. ) ;
#58716 = ADVANCED_FACE ( 'NONE', ( #65532 ), #107302, .T. ) ;
#58717 = EDGE_CURVE ( 'NONE', #65306, #83794, #27885, .T. ) ;
#58718 = ADVANCED_FACE ( 'NONE', ( #8527 ), #49784, .T. ) ;
#58719 = ADVANCED_FACE ( 'NONE', ( #89689 ), #65439, .T. ) ;
#58720 = ORIENTED_EDGE ( 'NONE', *, *, #59383, .T. ) ;
#58721 = DIRECTION ( 'NONE',  ( -0.000000000000000000, 1.000000000000000000, -0.000000000000000000 ) ) ;
#58722 = EDGE_LOOP ( 'NONE', ( #90146, #72939 ) ) ;
#58723 = ORIENTED_EDGE ( 'NONE', *, *, #25578, .F. ) ;
#58724 = VERTEX_POINT ( 'NONE', #9840 ) ;
#58725 = FACE_OUTER_BOUND ( 'NONE', #117788, .T. ) ;
#58726 = EDGE_CURVE ( 'NONE', #55549, #77652, #8998, .T. ) ;
#58727 = DIRECTION ( 'NONE',  ( 0.000000000000000000, 0.000000000000000000, 1.000000000000000000 ) ) ;
#58728 = DIRECTION ( 'NONE',  ( 0.000000000000000000, 1.000000000000000000, 0.000000000000000000 ) ) ;
#58729 = EDGE_CURVE ( 'NONE', #6508, #20003, #100937, .T. ) ;
#58730 = CARTESIAN_POINT ( 'NONE',  ( 10.39999999999991154, 2.500000000000000000, -4.922947341949753586 ) ) ;
#58732 = ORIENTED_EDGE ( 'NONE', *, *, #115500, .T. ) ;
#58731 = ADVANCED_FACE ( 'NONE', ( #108679 ), #105145, .T. ) ;
#58733 = AXIS2_PLACEMENT_3D ( 'NONE', #56708, #77020, #7622 ) ;
#58734 = CARTESIAN_POINT ( 'NONE',  ( 1.049999999999953637, 2.500000000000000000, 2.511473670974873507 ) ) ;
#58735 = ORIENTED_EDGE ( 'NONE', *, *, #38037, .F. ) ;
#58736 = CARTESIAN_POINT ( 'NONE',  ( -5.200000000000020606, 2.500000000000000000, 3.983716857408420964 ) ) ;
#58737 = CARTESIAN_POINT ( 'NONE',  ( 18.78720903127623032, -2.539625591034306407, -4.564429507521173157 ) ) ;
#58738 = CARTESIAN_POINT ( 'NONE',  ( 2.949999999999946887, 2.500000000000000000, -2.165063509461101710 ) ) ;
#58739 = DIRECTION ( 'NONE',  ( 0.000000000000000000, -0.000000000000000000, 1.000000000000000000 ) ) ;
#58740 = DIRECTION ( 'NONE',  ( 0.000000000000000000, 0.000000000000000000, 1.000000000000000000 ) ) ;
#58741 = AXIS2_PLACEMENT_3D ( 'NONE', #50004, #2813, #21156 ) ;
#58742 = ORIENTED_EDGE ( 'NONE', *, *, #77191, .T. ) ;
#58743 = AXIS2_PLACEMENT_3D ( 'NONE', #102149, #93611, #81841 ) ;
#58744 = ORIENTED_EDGE ( 'NONE', *, *, #34546, .T. ) ;
#58745 = EDGE_LOOP ( 'NONE', ( #82089, #61269 ) ) ;
#58746 = ORIENTED_EDGE ( 'NONE', *, *, #34363, .T. ) ;
#58747 = VERTEX_POINT ( 'NONE', #58949 ) ;
#58748 = CARTESIAN_POINT ( 'NONE',  ( 8.149999999999923972, 2.500000000000000000, -6.248780366869526759 ) ) ;
#58749 = CARTESIAN_POINT ( 'NONE',  ( 65.39894234688509300, 3.129862333795020657, 5.811320850201310506 ) ) ;
#58750 = CARTESIAN_POINT ( 'NONE',  ( -13.74999999999995381, 12.50000000000000000, -2.165063509461099489 ) ) ;
#58751 = FACE_BOUND ( 'NONE', #77797, .T. ) ;
#58752 = DIRECTION ( 'NONE',  ( 0.000000000000000000, 1.000000000000000000, 0.000000000000000000 ) ) ;
#58753 = CARTESIAN_POINT ( 'NONE',  ( 186.6562500006828316, 8.891194145520236347, 5.444286225454521982E-16 ) ) ;
#58754 = CARTESIAN_POINT ( 'NONE',  ( 9.999999999999914735, 2.500000000000000000, 0.7928203230275495672 ) ) ;
#58755 = DIRECTION ( 'NONE',  ( 0.000000000000000000, 1.000000000000000000, 0.000000000000000000 ) ) ;
#58756 = CONICAL_SURFACE ( 'NONE', #98442, 0.1000000000000002554, 0.003490658503988666988 ) ;
#58757 = CIRCLE ( 'NONE', #2296, 0.06509327318403745899 ) ;
#58758 = CARTESIAN_POINT ( 'NONE',  ( 185.6302083336747444, -4.367472073101514418, -7.564683531250002702 ) ) ;
#58759 = CARTESIAN_POINT ( 'NONE',  ( -7.950000000000016165, 12.50000000000000000, -6.495190528383297135 ) ) ;
#58760 = DIRECTION ( 'NONE',  ( 0.000000000000000000, 1.000000000000000000, 0.000000000000000000 ) ) ;
#58761 = CIRCLE ( 'NONE', #127799, 0.09999999999999982514 ) ;
#58762 = CARTESIAN_POINT ( 'NONE',  ( 5.849999999999932143, 12.50000000000000000, 2.230156782645134950 ) ) ;
#58763 = ADVANCED_FACE ( 'NONE', ( #127048 ), #113570, .T. ) ;
#58764 = ORIENTED_EDGE ( 'NONE', *, *, #22365, .T. ) ;
#58765 = CIRCLE ( 'NONE', #127713, 0.1000000000000000472 ) ;
#58766 = VERTEX_POINT ( 'NONE', #39955 ) ;
#58767 = VERTEX_POINT ( 'NONE', #119792 ) ;
#58768 = ORIENTED_EDGE ( 'NONE', *, *, #65633, .F. ) ;
#58769 = CARTESIAN_POINT ( 'NONE',  ( -6.450000000000014388, 12.50000000000000000, 1.753560074763284016 ) ) ;
#58770 = DIRECTION ( 'NONE',  ( 0.000000000000000000, -0.000000000000000000, 1.000000000000000000 ) ) ;
#58771 = EDGE_CURVE ( 'NONE', #21419, #69282, #71708, .T. ) ;
#58772 = FACE_BOUND ( 'NONE', #83129, .T. ) ;
#58773 = CARTESIAN_POINT ( 'NONE',  ( 10.84999999999991260, 2.500000000000000000, 7.288010851410849256 ) ) ;
#58774 = EDGE_CURVE ( 'NONE', #70218, #120216, #29952, .T. ) ;
#58775 = EDGE_CURVE ( 'NONE', #7138, #54276, #88421, .T. ) ;
#58776 = EDGE_LOOP ( 'NONE', ( #41531, #103595 ) ) ;
#58777 = CARTESIAN_POINT ( 'NONE',  ( -6.650000000000018119, 2.500000000000000000, -2.165063509461101710 ) ) ;
#58778 = LINE ( 'NONE', #14471, #59956 ) ;
#58779 = LINE ( 'NONE', #91295, #62484 ) ;
#58780 = CARTESIAN_POINT ( 'NONE',  ( -5.600000000000020073, 2.500000000000000000, 0.3464101615137736845 ) ) ;
#58781 = ORIENTED_EDGE ( 'NONE', *, *, #67117, .T. ) ;
#58782 = CARTESIAN_POINT ( 'NONE',  ( 107.5000000000000142, -1.500000000000000222, 1.322875655532295136 ) ) ;
#58783 = ADVANCED_FACE ( 'NONE', ( #38683 ), #77965, .T. ) ;
#58784 = MANIFOLD_SOLID_BREP ( 'Boss-Extrude2', #33189 ) ;
#58785 = VERTEX_POINT ( 'NONE', #47846 ) ;
#58786 = AXIS2_PLACEMENT_3D ( 'NONE', #75253, #24869, #64782 ) ;
#58787 = VERTEX_POINT ( 'NONE', #87738 ) ;
#58788 = PLANE ( 'NONE',  #6864 ) ;
#58789 = AXIS2_PLACEMENT_3D ( 'NONE', #67671, #127262, #77497 ) ;
#58790 = PLANE ( 'NONE',  #20427 ) ;
#58791 = ORIENTED_EDGE ( 'NONE', *, *, #43954, .T. ) ;
#58792 = DIRECTION ( 'NONE',  ( 0.000000000000000000, 0.000000000000000000, 1.000000000000000000 ) ) ;
#58793 = CONICAL_SURFACE ( 'NONE', #16975, 0.09999999999999999167, 0.003490658503988666988 ) ;
#58795 = AXIS2_PLACEMENT_3D ( 'NONE', #34517, #45618, #124813 ) ;
#58794 = CARTESIAN_POINT ( 'NONE',  ( -6.050000000000020250, 2.500000000000000000, -6.841600689897078702 ) ) ;
#58796 = ORIENTED_EDGE ( 'NONE', *, *, #126748, .F. ) ;
#58797 = DIRECTION ( 'NONE',  ( 0.000000000000000000, 1.000000000000000000, 0.000000000000000000 ) ) ;
#58798 = ORIENTED_EDGE ( 'NONE', *, *, #45238, .T. ) ;
#58799 = CIRCLE ( 'NONE', #60938, 0.06509327318403743123 ) ;
#58800 = CARTESIAN_POINT ( 'NONE',  ( -6.900000000000019007, 12.50000000000000000, -3.918623584224389056 ) ) ;
#58801 = EDGE_CURVE ( 'NONE', #74701, #72217, #115606, .T. ) ;
#58802 = EDGE_LOOP ( 'NONE', ( #89406, #111108, #83641, #32312 ) ) ;
#58803 = CARTESIAN_POINT ( 'NONE',  ( 0.1999999999999567124, 2.500000000000000000, -3.983716857408426293 ) ) ;
#58804 = FACE_BOUND ( 'NONE', #57610, .T. ) ;
#58805 = ORIENTED_EDGE ( 'NONE', *, *, #73086, .T. ) ;
#58806 = CARTESIAN_POINT ( 'NONE',  ( -2.900000000000029665, 2.500000000000000000, 3.637306695894644726 ) ) ;
#58807 = ORIENTED_EDGE ( 'NONE', *, *, #49861, .T. ) ;
#58808 = DIRECTION ( 'NONE',  ( 0.000000000000000000, -0.9999939076577903929, 0.003490651415223739937 ) ) ;
#58809 = DIRECTION ( 'NONE',  ( 0.000000000000000000, 0.000000000000000000, 1.000000000000000000 ) ) ;
#58810 = CARTESIAN_POINT ( 'NONE',  ( 184.5000000000000000, 0.000000000000000000, 0.000000000000000000 ) ) ;
#58811 = CARTESIAN_POINT ( 'NONE',  ( 3.749999999999940492, 2.500000000000000000, 5.702370205355745014 ) ) ;
#58812 = FACE_OUTER_BOUND ( 'NONE', #32688, .T. ) ;
#58813 = ORIENTED_EDGE ( 'NONE', *, *, #35114, .T. ) ;
#58814 = ORIENTED_EDGE ( 'NONE', *, *, #90285, .T. ) ;
#58815 = EDGE_LOOP ( 'NONE', ( #70085, #31198, #90003, #18449 ) ) ;
#58816 = DIRECTION ( 'NONE',  ( -0.000000000000000000, -1.000000000000000000, -0.000000000000000000 ) ) ;
#58817 = EDGE_CURVE ( 'NONE', #128968, #96874, #73854, .T. ) ;
#58818 = CARTESIAN_POINT ( 'NONE',  ( -9.800000000000006040, 12.50000000000000000, 0.4115034346978109769 ) ) ;
#58819 = LINE ( 'NONE', #98724, #56442 ) ;
#58821 = VERTEX_POINT ( 'NONE', #122176 ) ;
#58820 = ORIENTED_EDGE ( 'NONE', *, *, #97604, .T. ) ;
#58822 = ORIENTED_EDGE ( 'NONE', *, *, #97529, .T. ) ;
#58823 = PLANE ( 'NONE',  #49882 ) ;
#58824 = AXIS2_PLACEMENT_3D ( 'NONE', #47606, #88129, #105873 ) ;
#58825 = DIRECTION ( 'NONE',  ( -0.000000000000000000, -1.000000000000000000, -0.000000000000000000 ) ) ;
#58826 = AXIS2_PLACEMENT_3D ( 'NONE', #106954, #96483, #17268 ) ;
#58827 = DIRECTION ( 'NONE',  ( 0.000000000000000000, 1.000000000000000000, 0.000000000000000000 ) ) ;
#58828 = CARTESIAN_POINT ( 'NONE',  ( -6.850000000000017408, 2.500000000000000000, -6.841600689897077814 ) ) ;
#58829 = CARTESIAN_POINT ( 'NONE',  ( 11.44999999999990692, 12.50000000000000000, 1.818653347947321475 ) ) ;
#58830 = CARTESIAN_POINT ( 'NONE',  ( 4.349999999999938360, 12.50000000000000000, 1.753560074763284016 ) ) ;
#58831 = LINE ( 'NONE', #89577, #75944 ) ;
#58832 = EDGE_CURVE ( 'NONE', #87563, #103647, #2738, .T. ) ;
#58833 = CARTESIAN_POINT ( 'NONE',  ( -6.650000000000014566, 12.50000000000000000, 5.867463478539781896 ) ) ;
#58834 = ORIENTED_EDGE ( 'NONE', *, *, #117199, .F. ) ;
#58835 = AXIS2_PLACEMENT_3D ( 'NONE', #69960, #129547, #9744 ) ;
#58836 = ORIENTED_EDGE ( 'NONE', *, *, #48973, .T. ) ;
#58837 = DIRECTION ( 'NONE',  ( 0.000000000000000000, 1.000000000000000000, 0.000000000000000000 ) ) ;
#58838 = DIRECTION ( 'NONE',  ( 0.000000000000000000, -0.000000000000000000, 1.000000000000000000 ) ) ;
#58839 = EDGE_LOOP ( 'NONE', ( #121265, #24016 ) ) ;
#58840 = VERTEX_POINT ( 'NONE', #103170 ) ;
#58841 = CARTESIAN_POINT ( 'NONE',  ( 185.7760416670080588, 6.551208109652274736, 3.782341765625001351 ) ) ;
#58842 = DIRECTION ( 'NONE',  ( 0.000000000000000000, 0.000000000000000000, -1.000000000000000000 ) ) ;
#58843 = LINE ( 'NONE', #128899, #107272 ) ;
#58844 = FACE_OUTER_BOUND ( 'NONE', #24663, .T. ) ;
#58845 = AXIS2_PLACEMENT_3D ( 'NONE', #16296, #24853, #125612 ) ;
#58846 = AXIS2_PLACEMENT_3D ( 'NONE', #87386, #27826, #98491 ) ;
#58847 = DIRECTION ( 'NONE',  ( -0.000000000000000000, 1.000000000000000000, -0.000000000000000000 ) ) ;
#58848 = LINE ( 'NONE', #555, #7187 ) ;
#58849 = VECTOR ( 'NONE', #90746, 1000.000000000000000 ) ;
#58850 = DIRECTION ( 'NONE',  ( 0.000000000000000000, 0.000000000000000000, -1.000000000000000000 ) ) ;
#58851 = VECTOR ( 'NONE', #48132, 1000.000000000000000 ) ;
#58852 = DIRECTION ( 'NONE',  ( 0.000000000000000000, 0.000000000000000000, -1.000000000000000000 ) ) ;
#58853 = ORIENTED_EDGE ( 'NONE', *, *, #25632, .F. ) ;
#58854 = EDGE_CURVE ( 'NONE', #96136, #80214, #13195, .T. ) ;
#58855 = CIRCLE ( 'NONE', #37924, 0.1000000000000000056 ) ;
#58856 = AXIS2_PLACEMENT_3D ( 'NONE', #87470, #26001, #27268 ) ;
#58857 = VERTEX_POINT ( 'NONE', #12193 ) ;
#58858 = ORIENTED_EDGE ( 'NONE', *, *, #91688, .F. ) ;
#58859 = ORIENTED_EDGE ( 'NONE', *, *, #79152, .T. ) ;
#58860 = DIRECTION ( 'NONE',  ( 0.000000000000000000, -0.9999939076577903929, 0.003490651415223739937 ) ) ;
#58861 = FACE_OUTER_BOUND ( 'NONE', #101855, .T. ) ;
#58862 = EDGE_CURVE ( 'NONE', #12583, #64010, #103713, .T. ) ;
#58863 = ORIENTED_EDGE ( 'NONE', *, *, #123486, .T. ) ;
#58864 = DIRECTION ( 'NONE',  ( 0.000000000000000000, 0.000000000000000000, 1.000000000000000000 ) ) ;
#58865 = CARTESIAN_POINT ( 'NONE',  ( 17.50000000000000000, -0.9166666666666696273, -2.864912725862979848 ) ) ;
#58866 = CARTESIAN_POINT ( 'NONE',  ( 184.5000000000000000, 0.000000000000000000, -7.699999999999999289 ) ) ;
#58868 = ORIENTED_EDGE ( 'NONE', *, *, #90237, .F. ) ;
#58867 = DIRECTION ( 'NONE',  ( 0.000000000000000000, 0.000000000000000000, 1.000000000000000000 ) ) ;
#58869 = ADVANCED_FACE ( 'NONE', ( #72430 ), #3045, .T. ) ;
#58870 = EDGE_CURVE ( 'NONE', #50389, #64315, #119827, .T. ) ;
#58871 = EDGE_CURVE ( 'NONE', #40542, #23039, #13482, .T. ) ;
#58872 = DIRECTION ( 'NONE',  ( 0.000000000000000000, 1.000000000000000000, 0.000000000000000000 ) ) ;
#58873 = EDGE_CURVE ( 'NONE', #79801, #59178, #80123, .T. ) ;
#58874 = CARTESIAN_POINT ( 'NONE',  ( 1.849999999999950573, 12.50000000000000000, -1.818653347947326138 ) ) ;
#58875 = EDGE_LOOP ( 'NONE', ( #103475, #731, #63336, #69933 ) ) ;
#58876 = ORIENTED_EDGE ( 'NONE', *, *, #123033, .F. ) ;
#58878 = ORIENTED_EDGE ( 'NONE', *, *, #91850, .T. ) ;
#58877 = EDGE_CURVE ( 'NONE', #89429, #3071, #40429, .T. ) ;
#58879 = CIRCLE ( 'NONE', #109026, 0.06509327318403745899 ) ;
#58880 = ORIENTED_EDGE ( 'NONE', *, *, #43518, .F. ) ;
#58881 = DIRECTION ( 'NONE',  ( -0.000000000000000000, 1.000000000000000000, -0.000000000000000000 ) ) ;
#58882 = CIRCLE ( 'NONE', #127824, 0.1000000000000000472 ) ;
#58883 = CIRCLE ( 'NONE', #75587, 0.06509327318403745899 ) ;
#58884 = ADVANCED_FACE ( 'NONE', ( #111703 ), #71125, .T. ) ;
#58885 = EDGE_CURVE ( 'NONE', #35899, #106061, #93352, .T. ) ;
#58886 = CARTESIAN_POINT ( 'NONE',  ( 14.99999999999992895, 12.50000000000000000, -2.276824562219559311E-15 ) ) ;
#58887 = ADVANCED_FACE ( 'NONE', ( #111029 ), #86453, .T. ) ;
#58889 = EDGE_CURVE ( 'NONE', #104132, #37082, #101885, .T. ) ;
#58888 = AXIS2_PLACEMENT_3D ( 'NONE', #78549, #90260, #9141 ) ;
#58890 = AXIS2_PLACEMENT_3D ( 'NONE', #120783, #21965, #51427 ) ;
#58892 = ORIENTED_EDGE ( 'NONE', *, *, #57622, .F. ) ;
#58891 = CONICAL_SURFACE ( 'NONE', #2430, 0.1000000000000002554, 0.003490658503988666988 ) ;
#58893 = CARTESIAN_POINT ( 'NONE',  ( -8.150000000000009237, 2.500000000000000000, 6.941600689897073018 ) ) ;
#58894 = CARTESIAN_POINT ( 'NONE',  ( 19.52519901027828197, -0.5909487300084618200, -4.333354523369954414 ) ) ;
#58895 = DIRECTION ( 'NONE',  ( 0.000000000000000000, 1.000000000000000000, 0.000000000000000000 ) ) ;
#58896 = CARTESIAN_POINT ( 'NONE',  ( 5.849999999999932143, 2.500000000000000000, 2.165063509461097713 ) ) ;
#58897 = EDGE_CURVE ( 'NONE', #18181, #82263, #107888, .T. ) ;
#58898 = VECTOR ( 'NONE', #27208, 1000.000000000000000 ) ;
#58899 = EDGE_LOOP ( 'NONE', ( #96319, #56818 ) ) ;
#58900 = CARTESIAN_POINT ( 'NONE',  ( -2.100000000000034728, 12.50000000000000000, 4.395220292106234439 ) ) ;
#58901 = ORIENTED_EDGE ( 'NONE', *, *, #8713, .T. ) ;
#58902 = ORIENTED_EDGE ( 'NONE', *, *, #112585, .F. ) ;
#58903 = LINE ( 'NONE', #17670, #112400 ) ;
#58904 = DIRECTION ( 'NONE',  ( 0.000000000000000000, 0.000000000000000000, 1.000000000000000000 ) ) ;
#58905 = FACE_BOUND ( 'NONE', #76286, .T. ) ;
#58906 = DIRECTION ( 'NONE',  ( -0.000000000000000000, 1.000000000000000000, -0.000000000000000000 ) ) ;
#58907 = DIRECTION ( 'NONE',  ( 0.000000000000000000, 0.000000000000000000, -1.000000000000000000 ) ) ;
#58908 = DIRECTION ( 'NONE',  ( 0.000000000000000000, 0.000000000000000000, 1.000000000000000000 ) ) ;
#58909 = ORIENTED_EDGE ( 'NONE', *, *, #30554, .T. ) ;
#58910 = DIRECTION ( 'NONE',  ( 0.000000000000000000, 1.000000000000000000, 0.000000000000000000 ) ) ;
#58911 = CARTESIAN_POINT ( 'NONE',  ( -11.89999999999999680, 2.500000000000000000, -3.883716857408423984 ) ) ;
#58912 = DIRECTION ( 'NONE',  ( 0.000000000000000000, 0.000000000000000000, 1.000000000000000000 ) ) ;
#58913 = DIRECTION ( 'NONE',  ( -0.000000000000000000, 1.000000000000000000, -0.000000000000000000 ) ) ;
#58914 = VERTEX_POINT ( 'NONE', #105083 ) ;
#58915 = CIRCLE ( 'NONE', #23297, 0.06509327318403745899 ) ;
#58916 = CARTESIAN_POINT ( 'NONE',  ( 2.699999999999946443, 2.500000000000000000, -3.983716857408426293 ) ) ;
#58917 = CARTESIAN_POINT ( 'NONE',  ( 9.999999999999911182, 2.500000000000000000, -3.537306695894649966 ) ) ;
#58918 = VERTEX_POINT ( 'NONE', #94625 ) ;
#58919 = ORIENTED_EDGE ( 'NONE', *, *, #69687, .T. ) ;
#58920 = CARTESIAN_POINT ( 'NONE',  ( -3.150000000000030109, 2.500000000000000000, -2.611473670974877592 ) ) ;
#58921 = CARTESIAN_POINT ( 'NONE',  ( -3.300000000000028244, 2.500000000000000000, 4.230127018922196669 ) ) ;
#58922 = FACE_BOUND ( 'NONE', #125770, .T. ) ;
#58923 = AXIS2_PLACEMENT_3D ( 'NONE', #58100, #61320, #42320 ) ;
#58924 = CARTESIAN_POINT ( 'NONE',  ( -14.34999999999998543, 2.500000000000000000, 1.718653347947325383 ) ) ;
#58925 = AXIS2_PLACEMENT_3D ( 'NONE', #93276, #74926, #124017 ) ;
#58926 = EDGE_CURVE ( 'NONE', #54395, #35289, #16694, .T. ) ;
#58927 = VERTEX_POINT ( 'NONE', #15413 ) ;
#58929 = DIRECTION ( 'NONE',  ( 0.000000000000000000, 0.000000000000000000, -1.000000000000000000 ) ) ;
#58928 = AXIS2_PLACEMENT_3D ( 'NONE', #122147, #23271, #103132 ) ;
#58930 = VECTOR ( 'NONE', #112087, 1000.000000000000000 ) ;
#58931 = ADVANCED_FACE ( 'NONE', ( #95924 ), #44610, .T. ) ;
#58932 = VERTEX_POINT ( 'NONE', #14756 ) ;
#58933 = LINE ( 'NONE', #49128, #8957 ) ;
#58934 = CARTESIAN_POINT ( 'NONE',  ( 187.2083333333333428, -4.445597072760115509, -7.700000000000001954 ) ) ;
#58935 = ORIENTED_EDGE ( 'NONE', *, *, #111194, .F. ) ;
#58937 = PLANE ( 'NONE',  #126339 ) ;
#58936 = VECTOR ( 'NONE', #127952, 1000.000000000000000 ) ;
#58938 = CARTESIAN_POINT ( 'NONE',  ( 8.949999999999919353, 12.50000000000000000, 2.511473670974873507 ) ) ;
#58939 = EDGE_CURVE ( 'NONE', #45959, #119467, #23786, .T. ) ;
#58940 = AXIS2_PLACEMENT_3D ( 'NONE', #3531, #75481, #34943 ) ;
#58941 = EDGE_CURVE ( 'NONE', #61697, #41126, #107391, .T. ) ;
#58942 = AXIS2_PLACEMENT_3D ( 'NONE', #78081, #59753, #68248 ) ;
#58943 = AXIS2_PLACEMENT_3D ( 'NONE', #42092, #204, #40159 ) ;
#58944 = AXIS2_PLACEMENT_3D ( 'NONE', #18696, #58643, #98530 ) ;
#58945 = DIRECTION ( 'NONE',  ( -0.000000000000000000, 1.000000000000000000, -0.000000000000000000 ) ) ;
#58946 = CARTESIAN_POINT ( 'NONE',  ( 11.24999999999990585, 2.500000000000000000, 2.757883832488649656 ) ) ;
#58947 = CIRCLE ( 'NONE', #2488, 0.1000000000000002554 ) ;
#58948 = ORIENTED_EDGE ( 'NONE', *, *, #36154, .F. ) ;
#58949 = CARTESIAN_POINT ( 'NONE',  ( -1.658312395177699017, -2.500000000000000444, -5.000000000000004441 ) ) ;
#58950 = CIRCLE ( 'NONE', #67319, 0.09999999999999982514 ) ;
#58951 = DIRECTION ( 'NONE',  ( 0.000000000000000000, 1.000000000000000000, 0.000000000000000000 ) ) ;
#58952 = LINE ( 'NONE', #68107, #91032 ) ;
#58953 = LINE ( 'NONE', #28849, #51186 ) ;
#58954 = VERTEX_POINT ( 'NONE', #93995 ) ;
#58955 = EDGE_LOOP ( 'NONE', ( #77531, #89624, #80590, #92604 ) ) ;
#58956 = EDGE_LOOP ( 'NONE', ( #91902, #106095, #102406, #119863 ) ) ;
#58957 = CARTESIAN_POINT ( 'NONE',  ( 184.5000000000000000, -2.986254062820097310, -7.097343634930640022 ) ) ;
#58958 = CARTESIAN_POINT ( 'NONE',  ( 87.50000000000001421, -3.974992050023845369, 6.359987280038161828 ) ) ;
#58959 = CARTESIAN_POINT ( 'NONE',  ( -0.8500000000000386136, 2.500000000000000000, 1.472243186433545459 ) ) ;
#58960 = CARTESIAN_POINT ( 'NONE',  ( -12.69999999999999041, 12.50000000000000000, 3.983716857408420964 ) ) ;
#58961 = VERTEX_POINT ( 'NONE', #6231 ) ;
#58962 = FACE_OUTER_BOUND ( 'NONE', #25057, .T. ) ;
#58963 = CARTESIAN_POINT ( 'NONE',  ( -9.150000000000009237, 2.500000000000000000, -2.757883832488654097 ) ) ;
#58964 = DIRECTION ( 'NONE',  ( 0.000000000000000000, 0.000000000000000000, 1.000000000000000000 ) ) ;
#58965 = CARTESIAN_POINT ( 'NONE',  ( 184.6510416670080588, 4.367472073101518859, -7.564683531249999149 ) ) ;
#58966 = CARTESIAN_POINT ( 'NONE',  ( 0.5999999999999551248, 2.500000000000000000, -4.576537180435978236 ) ) ;
#58967 = DIRECTION ( 'NONE',  ( 0.000000000000000000, -0.9999939076577903929, 0.003490651415223739937 ) ) ;
#58968 = EDGE_CURVE ( 'NONE', #98422, #34323, #24615, .T. ) ;
#58969 = ORIENTED_EDGE ( 'NONE', *, *, #40005, .T. ) ;
#58970 = EDGE_LOOP ( 'NONE', ( #71834, #60622 ) ) ;
#58971 = CARTESIAN_POINT ( 'NONE',  ( 8.349999999999923261, 2.500000000000000000, 1.572243186433545548 ) ) ;
#58972 = VERTEX_POINT ( 'NONE', #103820 ) ;
#58973 = CIRCLE ( 'NONE', #94552, 0.09999999999999982514 ) ;
#58974 = CARTESIAN_POINT ( 'NONE',  ( 15.19999999999989093, 2.500000000000000000, 0.2464101615137735679 ) ) ;
#58975 = CIRCLE ( 'NONE', #119592, 0.06509327318403745899 ) ;
#58977 = VERTEX_POINT ( 'NONE', #126016 ) ;
#58976 = ORIENTED_EDGE ( 'NONE', *, *, #124170, .T. ) ;
#58978 = EDGE_LOOP ( 'NONE', ( #129540, #31686, #118287, #76701 ) ) ;
#58979 = CARTESIAN_POINT ( 'NONE',  ( 17.50000000000000000, -0.4166666666666616337, -3.999999999999996447 ) ) ;
#58980 = FACE_OUTER_BOUND ( 'NONE', #86765, .T. ) ;
#58981 = CONICAL_SURFACE ( 'NONE', #50657, 0.09999999999999999167, 0.003490658503988666988 ) ;
#58983 = LINE ( 'NONE', #48, #91488 ) ;
#58982 = CIRCLE ( 'NONE', #31793, 0.09999999999999982514 ) ;
#58984 = CIRCLE ( 'NONE', #79807, 0.09999999999999982514 ) ;
#58985 = DIRECTION ( 'NONE',  ( -0.000000000000000000, -1.000000000000000000, -0.000000000000000000 ) ) ;
#58986 = DIRECTION ( 'NONE',  ( -0.000000000000000000, 1.000000000000000000, -0.000000000000000000 ) ) ;
#58988 = EDGE_CURVE ( 'NONE', #109829, #10701, #61340, .T. ) ;
#58987 = AXIS2_PLACEMENT_3D ( 'NONE', #37565, #108218, #106290 ) ;
#58989 = DIRECTION ( 'NONE',  ( 0.000000000000000000, 0.000000000000000000, -1.000000000000000000 ) ) ;
#58990 = DIRECTION ( 'NONE',  ( -0.000000000000000000, -1.000000000000000000, -0.000000000000000000 ) ) ;
#58991 = AXIS2_PLACEMENT_3D ( 'NONE', #74823, #7351, #15889 ) ;
#58992 = EDGE_CURVE ( 'NONE', #58747, #61997, #83540, .T. ) ;
#58993 = FACE_OUTER_BOUND ( 'NONE', #82901, .T. ) ;
#58994 = EDGE_LOOP ( 'NONE', ( #53110, #73529, #126941, #72999 ) ) ;
#58995 = VERTEX_POINT ( 'NONE', #84809 ) ;
#58996 = FACE_OUTER_BOUND ( 'NONE', #129574, .T. ) ;
#58997 = ORIENTED_EDGE ( 'NONE', *, *, #128067, .T. ) ;
#58998 = EDGE_CURVE ( 'NONE', #49639, #48345, #50984, .T. ) ;
#58999 = ORIENTED_EDGE ( 'NONE', *, *, #48952, .T. ) ;
#59000 = LINE ( 'NONE', #68813, #100544 ) ;
#59001 = PLANE ( 'NONE',  #100580 ) ;
#59002 = LINE ( 'NONE', #108087, #121655 ) ;
#59003 = CARTESIAN_POINT ( 'NONE',  ( 5.199999999999931788, 2.500000000000000000, 4.676537180435972552 ) ) ;
#59004 = DIRECTION ( 'NONE',  ( -0.000000000000000000, -1.000000000000000000, -0.000000000000000000 ) ) ;
#59005 = ORIENTED_EDGE ( 'NONE', *, *, #10516, .F. ) ;
#59006 = AXIS2_PLACEMENT_3D ( 'NONE', #27295, #98602, #67193 ) ;
#59007 = VERTEX_POINT ( 'NONE', #66457 ) ;
#59008 = DIRECTION ( 'NONE',  ( -0.000000000000000000, -1.000000000000000000, -0.000000000000000000 ) ) ;
#59009 = ORIENTED_EDGE ( 'NONE', *, *, #106270, .F. ) ;
#59010 = DIRECTION ( 'NONE',  ( 0.000000000000000000, 1.000000000000000000, 0.000000000000000000 ) ) ;
#59011 = ORIENTED_EDGE ( 'NONE', *, *, #42508, .F. ) ;
#59012 = ORIENTED_EDGE ( 'NONE', *, *, #114252, .F. ) ;
#59013 = AXIS2_PLACEMENT_3D ( 'NONE', #65148, #35090, #76287 ) ;
#59014 = CARTESIAN_POINT ( 'NONE',  ( 8.349999999999923261, 2.500000000000000000, 1.572243186433545548 ) ) ;
#59015 = PLANE ( 'NONE',  #54797 ) ;
#59016 = AXIS2_PLACEMENT_3D ( 'NONE', #49355, #58524, #68317 ) ;
#59018 = ADVANCED_FACE ( 'NONE', ( #4291 ), #2845, .T. ) ;
#59017 = AXIS2_PLACEMENT_3D ( 'NONE', #121962, #121311, #32319 ) ;
#59019 = FACE_OUTER_BOUND ( 'NONE', #78267, .T. ) ;
#59020 = AXIS2_PLACEMENT_3D ( 'NONE', #124059, #74963, #94584 ) ;
#59021 = DIRECTION ( 'NONE',  ( 0.000000000000000000, 1.000000000000000000, 0.000000000000000000 ) ) ;
#59022 = CARTESIAN_POINT ( 'NONE',  ( 12.69999999999990159, 2.500000000000000000, -3.983716857408426293 ) ) ;
#59023 = ORIENTED_EDGE ( 'NONE', *, *, #108837, .T. ) ;
#59024 = CARTESIAN_POINT ( 'NONE',  ( 12.89999999999990266, 12.50000000000000000, 4.957854068765711553 ) ) ;
#59025 = CARTESIAN_POINT ( 'NONE',  ( -0.8000000000000381251, 12.50000000000000000, 4.330127018922196314 ) ) ;
#59026 = EDGE_CURVE ( 'NONE', #60686, #104656, #17494, .T. ) ;
#59027 = CARTESIAN_POINT ( 'NONE',  ( 2.949999999999943334, 12.50000000000000000, 6.560283801567334372 ) ) ;
#59028 = ADVANCED_FACE ( 'NONE', ( #54069 ), #40526, .T. ) ;
#59029 = DIRECTION ( 'NONE',  ( 0.000000000000000000, 0.000000000000000000, -1.000000000000000000 ) ) ;
#59030 = EDGE_CURVE ( 'NONE', #120803, #120419, #67677, .T. ) ;
#59031 = AXIS2_PLACEMENT_3D ( 'NONE', #80152, #114582, #20586 ) ;
#59032 = CONICAL_SURFACE ( 'NONE', #13028, 0.1000000000000000472, 0.003490658503988666988 ) ;
#59033 = LINE ( 'NONE', #68190, #66761 ) ;
#59034 = VERTEX_POINT ( 'NONE', #75620 ) ;
#59035 = AXIS2_PLACEMENT_3D ( 'NONE', #55099, #106129, #14506 ) ;
#59036 = VERTEX_POINT ( 'NONE', #84161 ) ;
#59037 = EDGE_CURVE ( 'NONE', #28707, #64176, #105750, .T. ) ;
#59038 = CARTESIAN_POINT ( 'NONE',  ( -10.85000000000000142, 2.500000000000000000, -6.395190528383298378 ) ) ;
#59039 = EDGE_CURVE ( 'NONE', #88979, #62189, #124094, .T. ) ;
#59040 = AXIS2_PLACEMENT_3D ( 'NONE', #29465, #69370, #89670 ) ;
#59041 = EDGE_LOOP ( 'NONE', ( #40432, #45684 ) ) ;
#59042 = CARTESIAN_POINT ( 'NONE',  ( -5.200000000000020606, 2.500000000000000000, 3.983716857408420964 ) ) ;
#59043 = CARTESIAN_POINT ( 'NONE',  ( -11.64999999999999858, 2.500000000000000000, -1.472243186433546125 ) ) ;
#59044 = ADVANCED_FACE ( 'NONE', ( #34446 ), #27977, .T. ) ;
#59045 = CIRCLE ( 'NONE', #104989, 0.1000000000000000472 ) ;
#59046 = ORIENTED_EDGE ( 'NONE', *, *, #51653, .F. ) ;
#59047 = DIRECTION ( 'NONE',  ( 0.000000000000000000, 1.000000000000000000, 0.000000000000000000 ) ) ;
#59048 = DIRECTION ( 'NONE',  ( 0.000000000000000000, 0.000000000000000000, -1.000000000000000000 ) ) ;
#59049 = EDGE_CURVE ( 'NONE', #121438, #99874, #25901, .T. ) ;
#59050 = DIRECTION ( 'NONE',  ( -0.000000000000000000, 1.000000000000000000, -0.000000000000000000 ) ) ;
#59051 = FACE_OUTER_BOUND ( 'NONE', #92802, .T. ) ;
#59052 = ORIENTED_EDGE ( 'NONE', *, *, #71720, .T. ) ;
#59053 = ADVANCED_FACE ( 'NONE', ( #78884 ), #108317, .T. ) ;
#59054 = LINE ( 'NONE', #98972, #116707 ) ;
#59055 = VERTEX_POINT ( 'NONE', #48124 ) ;
#59056 = AXIS2_PLACEMENT_3D ( 'NONE', #19067, #126477, #87173 ) ;
#59057 = CARTESIAN_POINT ( 'NONE',  ( 7.299999999999926104, 12.50000000000000000, 4.611443907251934426 ) ) ;
#59058 = CARTESIAN_POINT ( 'NONE',  ( -0.4500000000000402012, 12.50000000000000000, 6.560283801567334372 ) ) ;
#59059 = DIRECTION ( 'NONE',  ( 0.000000000000000000, 1.000000000000000000, 0.000000000000000000 ) ) ;
#59060 = ORIENTED_EDGE ( 'NONE', *, *, #69786, .T. ) ;
#59061 = CARTESIAN_POINT ( 'NONE',  ( -5.400000000000020783, 2.500000000000000000, 5.122947341949749323 ) ) ;
#59062 = AXIS2_PLACEMENT_3D ( 'NONE', #58609, #79533, #78904 ) ;
#59063 = CIRCLE ( 'NONE', #63258, 0.06509327318403745899 ) ;
#59064 = AXIS2_PLACEMENT_3D ( 'NONE', #106015, #75899, #86355 ) ;
#59065 = ORIENTED_EDGE ( 'NONE', *, *, #26286, .T. ) ;
#59066 = CARTESIAN_POINT ( 'NONE',  ( -3.750000000000025757, 12.50000000000000000, -2.857883832488653741 ) ) ;
#59067 = DIRECTION ( 'NONE',  ( 0.000000000000000000, 1.000000000000000000, 0.000000000000000000 ) ) ;
#59068 = CARTESIAN_POINT ( 'NONE',  ( 4.349999999999936584, 2.500000000000000000, 6.148780366869520009 ) ) ;
#59069 = ORIENTED_EDGE ( 'NONE', *, *, #47377, .T. ) ;
#59071 = CARTESIAN_POINT ( 'NONE',  ( 13.34999999999990017, 2.500000000000000000, 2.857883832488649301 ) ) ;
#59070 = AXIS2_PLACEMENT_3D ( 'NONE', #121135, #102148, #91033 ) ;
#59072 = AXIS2_PLACEMENT_3D ( 'NONE', #68031, #40537, #117758 ) ;
#59073 = AXIS2_PLACEMENT_3D ( 'NONE', #91016, #117883, #78638 ) ;
#59074 = DIRECTION ( 'NONE',  ( 0.000000000000000000, 0.000000000000000000, 1.000000000000000000 ) ) ;
#59075 = AXIS2_PLACEMENT_3D ( 'NONE', #119647, #78470, #109176 ) ;
#59076 = VERTEX_POINT ( 'NONE', #107683 ) ;
#59077 = AXIS2_PLACEMENT_3D ( 'NONE', #55598, #115801, #26145 ) ;
#59078 = DIRECTION ( 'NONE',  ( -0.000000000000000000, -1.000000000000000000, -0.000000000000000000 ) ) ;
#59079 = ORIENTED_EDGE ( 'NONE', *, *, #64332, .T. ) ;
#59080 = CONICAL_SURFACE ( 'NONE', #44496, 0.09999999999999999167, 0.003490658503988666988 ) ;
#59081 = CARTESIAN_POINT ( 'NONE',  ( 0.3999999999999568345, 2.500000000000000000, -5.022947341949754119 ) ) ;
#59082 = ADVANCED_FACE ( 'NONE', ( #8812 ), #111360, .T. ) ;
#59083 = EDGE_LOOP ( 'NONE', ( #54724, #38303, #4542, #111919 ) ) ;
#59084 = CARTESIAN_POINT ( 'NONE',  ( 176.5000000000000000, 0.000000000000000000, 0.000000000000000000 ) ) ;
#59085 = DIRECTION ( 'NONE',  ( 0.000000000000000000, -0.000000000000000000, 1.000000000000000000 ) ) ;
#59086 = ADVANCED_FACE ( 'NONE', ( #97214 ), #121984, .T. ) ;
#59087 = ORIENTED_EDGE ( 'NONE', *, *, #81347, .F. ) ;
#59088 = VERTEX_POINT ( 'NONE', #58592 ) ;
#59089 = CARTESIAN_POINT ( 'NONE',  ( 6.699999999999930012, 2.500000000000000000, -4.330127018922201643 ) ) ;
#59090 = DIRECTION ( 'NONE',  ( -0.000000000000000000, -1.000000000000000000, -0.000000000000000000 ) ) ;
#59091 = ORIENTED_EDGE ( 'NONE', *, *, #2434, .T. ) ;
#59092 = AXIS2_PLACEMENT_3D ( 'NONE', #78874, #38967, #108937 ) ;
#59093 = CARTESIAN_POINT ( 'NONE',  ( 185.5000000000000000, 0.000000000000000000, 7.700000000000000178 ) ) ;
#59094 = DIRECTION ( 'NONE',  ( 0.000000000000000000, 0.000000000000000000, -1.000000000000000000 ) ) ;
#59095 = CARTESIAN_POINT ( 'NONE',  ( 7.099999999999928590, 12.50000000000000000, -4.330127018922201643 ) ) ;
#59096 = CARTESIAN_POINT ( 'NONE',  ( 105.4748215620571301, 7.550127796438022010, 4.327541908659619629 ) ) ;
#59097 = DIRECTION ( 'NONE',  ( -4.274815082592931898E-19, -0.9999939076577903929, -0.003490651415223739937 ) ) ;
#59098 = DIRECTION ( 'NONE',  ( 0.000000000000000000, 0.000000000000000000, 1.000000000000000000 ) ) ;
#59099 = CARTESIAN_POINT ( 'NONE',  ( -8.550000000000007816, 2.500000000000000000, 6.148780366869520009 ) ) ;
#59100 = CONICAL_SURFACE ( 'NONE', #125881, 0.1000000000000000472, 0.003490658503988666988 ) ;
#59101 = AXIS2_PLACEMENT_3D ( 'NONE', #101752, #42187, #91281 ) ;
#59102 = CIRCLE ( 'NONE', #96731, 0.06509327318403745899 ) ;
#59103 = ORIENTED_EDGE ( 'NONE', *, *, #2679, .T. ) ;
#59104 = ORIENTED_EDGE ( 'NONE', *, *, #97906, .F. ) ;
#59105 = VERTEX_POINT ( 'NONE', #48772 ) ;
#59106 = ORIENTED_EDGE ( 'NONE', *, *, #35455, .T. ) ;
#59107 = DIRECTION ( 'NONE',  ( 0.000000000000000000, -0.9999939076577903929, 0.003490651415223739937 ) ) ;
#59108 = CARTESIAN_POINT ( 'NONE',  ( 0.1999999999999576006, 12.50000000000000000, -4.676537180435978769 ) ) ;
#59109 = DIRECTION ( 'NONE',  ( 0.000000000000000000, 1.000000000000000000, 0.000000000000000000 ) ) ;
#59110 = EDGE_LOOP ( 'NONE', ( #20128, #101882, #99228, #76282 ) ) ;
#59111 = FACE_BOUND ( 'NONE', #69994, .T. ) ;
#59112 = ORIENTED_EDGE ( 'NONE', *, *, #1024, .F. ) ;
#59113 = VECTOR ( 'NONE', #117155, 1000.000000000000000 ) ;
#59114 = CARTESIAN_POINT ( 'NONE',  ( -5.400000000000020783, 2.500000000000000000, 0.7928203230275495672 ) ) ;
#59115 = DIRECTION ( 'NONE',  ( 0.000000000000000000, -0.000000000000000000, 1.000000000000000000 ) ) ;
#59116 = AXIS2_PLACEMENT_3D ( 'NONE', #28740, #117730, #79136 ) ;
#59118 = CARTESIAN_POINT ( 'NONE',  ( -1.250000000000035749, 2.500000000000000000, -7.288010851410854585 ) ) ;
#59117 = AXIS2_PLACEMENT_3D ( 'NONE', #93096, #123199, #63631 ) ;
#59119 = AXIS2_PLACEMENT_3D ( 'NONE', #123264, #33602, #91874 ) ;
#59120 = CARTESIAN_POINT ( 'NONE',  ( 5.649999999999934630, 2.500000000000000000, 6.148780366869520897 ) ) ;
#59121 = FACE_OUTER_BOUND ( 'NONE', #33846, .T. ) ;
#59122 = FACE_OUTER_BOUND ( 'NONE', #62210, .T. ) ;
#59123 = CARTESIAN_POINT ( 'NONE',  ( -0.8500000000000386136, 2.500000000000000000, 7.288010851410849256 ) ) ;
#59124 = FACE_OUTER_BOUND ( 'NONE', #33760, .T. ) ;
#59125 = DIRECTION ( 'NONE',  ( 0.000000000000000000, -0.9999939076577903929, 0.003490651415223739937 ) ) ;
#59126 = VECTOR ( 'NONE', #59580, 1000.000000000000000 ) ;
#59127 = CARTESIAN_POINT ( 'NONE',  ( 1.899999999999951283, 2.500000000000000000, -0.3464101615137782364 ) ) ;
#59128 = EDGE_CURVE ( 'NONE', #89644, #9662, #117459, .T. ) ;
#59129 = ORIENTED_EDGE ( 'NONE', *, *, #96084, .F. ) ;
#59130 = VERTEX_POINT ( 'NONE', #17999 ) ;
#59131 = ORIENTED_EDGE ( 'NONE', *, *, #20934, .F. ) ;
#59133 = ORIENTED_EDGE ( 'NONE', *, *, #62288, .T. ) ;
#59132 = VECTOR ( 'NONE', #111805, 1000.000000000000000 ) ;
#59134 = CIRCLE ( 'NONE', #4810, 0.1000000000000000472 ) ;
#59135 = CIRCLE ( 'NONE', #73681, 0.06509327318403745899 ) ;
#59136 = PLANE ( 'NONE',  #3720 ) ;
#59137 = FACE_OUTER_BOUND ( 'NONE', #59943, .T. ) ;
#59139 = EDGE_LOOP ( 'NONE', ( #95270, #8850 ) ) ;
#59138 = ORIENTED_EDGE ( 'NONE', *, *, #121057, .T. ) ;
#59140 = ORIENTED_EDGE ( 'NONE', *, *, #77750, .F. ) ;
#59141 = AXIS2_PLACEMENT_3D ( 'NONE', #76481, #115741, #46355 ) ;
#59142 = DIRECTION ( 'NONE',  ( 0.000000000000000000, -0.000000000000000000, 1.000000000000000000 ) ) ;
#59143 = ADVANCED_FACE ( 'NONE', ( #101568 ), #86745, .T. ) ;
#59144 = CARTESIAN_POINT ( 'NONE',  ( -10.65000000000000391, 12.50000000000000000, -2.511473670974873951 ) ) ;
#59145 = CONICAL_SURFACE ( 'NONE', #75837, 0.1000000000000000472, 0.003490658503988666988 ) ;
#59146 = LINE ( 'NONE', #119992, #18312 ) ;
#59147 = CARTESIAN_POINT ( 'NONE',  ( 6.249999999999930722, 2.500000000000000000, -1.472243186433550122 ) ) ;
#59148 = LINE ( 'NONE', #129197, #53461 ) ;
#59149 = DIRECTION ( 'NONE',  ( -4.274815082592931898E-19, -0.9999939076577903929, -0.003490651415223739937 ) ) ;
#59150 = ADVANCED_FACE ( 'NONE', ( #76935 ), #47475, .T. ) ;
#59151 = FACE_OUTER_BOUND ( 'NONE', #49133, .T. ) ;
#59152 = EDGE_CURVE ( 'NONE', #110699, #73698, #84410, .T. ) ;
#59153 = ORIENTED_EDGE ( 'NONE', *, *, #125392, .F. ) ;
#59154 = DIRECTION ( 'NONE',  ( 0.000000000000000000, 0.000000000000000000, -1.000000000000000000 ) ) ;
#59155 = ORIENTED_EDGE ( 'NONE', *, *, #68995, .F. ) ;
#59156 = ORIENTED_EDGE ( 'NONE', *, *, #19104, .F. ) ;
#59157 = VERTEX_POINT ( 'NONE', #37014 ) ;
#59158 = PLANE ( 'NONE',  #50476 ) ;
#59159 = CONICAL_SURFACE ( 'NONE', #2684, 0.1000000000000000472, 0.003490658503988666988 ) ;
#59160 = VERTEX_POINT ( 'NONE', #27181 ) ;
#59161 = EDGE_CURVE ( 'NONE', #70290, #10609, #57222, .T. ) ;
#59162 = EDGE_LOOP ( 'NONE', ( #33522, #101944 ) ) ;
#59163 = LINE ( 'NONE', #48050, #86175 ) ;
#59165 = LINE ( 'NONE', #80083, #1528 ) ;
#59164 = AXIS2_PLACEMENT_3D ( 'NONE', #16825, #47619, #98623 ) ;
#59166 = DIRECTION ( 'NONE',  ( 0.000000000000000000, 1.000000000000000000, 0.000000000000000000 ) ) ;
#59168 = CARTESIAN_POINT ( 'NONE',  ( -6.650000000000018119, 2.500000000000000000, -7.188010851410854052 ) ) ;
#59167 = AXIS2_PLACEMENT_3D ( 'NONE', #21579, #111899, #61523 ) ;
#59169 = CIRCLE ( 'NONE', #50839, 0.1000000000000000472 ) ;
#59170 = DIRECTION ( 'NONE',  ( -0.000000000000000000, -1.000000000000000000, -0.000000000000000000 ) ) ;
#59171 = ORIENTED_EDGE ( 'NONE', *, *, #68463, .F. ) ;
#59172 = DIRECTION ( 'NONE',  ( 0.000000000000000000, 0.000000000000000000, -1.000000000000000000 ) ) ;
#59173 = AXIS2_PLACEMENT_3D ( 'NONE', #32814, #21694, #2033 ) ;
#59175 = ORIENTED_EDGE ( 'NONE', *, *, #109533, .T. ) ;
#59174 = AXIS2_PLACEMENT_3D ( 'NONE', #18126, #29263, #27960 ) ;
#59176 = CARTESIAN_POINT ( 'NONE',  ( -0.4000000000000392131, 2.500000000000000000, -5.022947341949754119 ) ) ;
#59177 = CIRCLE ( 'NONE', #107275, 0.1000000000000002554 ) ;
#59178 = VERTEX_POINT ( 'NONE', #98485 ) ;
#59179 = CARTESIAN_POINT ( 'NONE',  ( 112.9994817707945032, 8.699702167353846605, -0.3436818946302461764 ) ) ;
#59180 = LINE ( 'NONE', #2168, #27366 ) ;
#59181 = AXIS2_PLACEMENT_3D ( 'NONE', #38551, #50280, #48341 ) ;
#59182 = ORIENTED_EDGE ( 'NONE', *, *, #122033, .T. ) ;
#59183 = CIRCLE ( 'NONE', #2715, 0.06509327318403745899 ) ;
#59184 = FACE_OUTER_BOUND ( 'NONE', #4685, .T. ) ;
#59185 = CARTESIAN_POINT ( 'NONE',  ( -2.100000000000033396, 2.500000000000000000, -3.737306695894649700 ) ) ;
#59186 = ORIENTED_EDGE ( 'NONE', *, *, #52372, .T. ) ;
#59187 = VECTOR ( 'NONE', #50482, 1000.000000000000000 ) ;
#59188 = EDGE_CURVE ( 'NONE', #48804, #92562, #778, .T. ) ;
#59189 = DIRECTION ( 'NONE',  ( 0.000000000000000000, -0.000000000000000000, 1.000000000000000000 ) ) ;
#59190 = ORIENTED_EDGE ( 'NONE', *, *, #23169, .F. ) ;
#59191 = ORIENTED_EDGE ( 'NONE', *, *, #21071, .T. ) ;
#59192 = DIRECTION ( 'NONE',  ( 0.000000000000000000, -0.000000000000000000, 1.000000000000000000 ) ) ;
#59193 = CARTESIAN_POINT ( 'NONE',  ( -9.400000000000007461, 2.500000000000000000, 4.676537180435972552 ) ) ;
#59194 = EDGE_CURVE ( 'NONE', #43418, #116689, #88010, .T. ) ;
#59195 = PLANE ( 'NONE',  #10399 ) ;
#59196 = PLANE ( 'NONE',  #42907 ) ;
#59197 = EDGE_CURVE ( 'NONE', #60736, #20798, #105246, .T. ) ;
#59198 = VECTOR ( 'NONE', #93198, 1000.000000000000000 ) ;
#59199 = DIRECTION ( 'NONE',  ( -0.000000000000000000, -1.000000000000000000, -0.000000000000000000 ) ) ;
#59200 = ORIENTED_EDGE ( 'NONE', *, *, #118745, .T. ) ;
#59201 = CARTESIAN_POINT ( 'NONE',  ( 13.09999999999990195, 2.500000000000000000, -3.983716857408426293 ) ) ;
#59202 = EDGE_CURVE ( 'NONE', #122805, #117378, #118785, .T. ) ;
#59203 = EDGE_CURVE ( 'NONE', #116703, #58176, #78058, .T. ) ;
#59204 = EDGE_CURVE ( 'NONE', #48991, #29616, #29138, .T. ) ;
#59205 = EDGE_CURVE ( 'NONE', #125412, #84079, #9101, .T. ) ;
#59206 = AXIS2_PLACEMENT_3D ( 'NONE', #102979, #44065, #101706 ) ;
#59207 = ORIENTED_EDGE ( 'NONE', *, *, #123836, .F. ) ;
#59208 = AXIS2_PLACEMENT_3D ( 'NONE', #15270, #64394, #85322 ) ;
#59209 = CARTESIAN_POINT ( 'NONE',  ( 9.999999999999916511, 2.500000000000000000, -0.5928203230275541635 ) ) ;
#59210 = DIRECTION ( 'NONE',  ( 0.000000000000000000, 1.000000000000000000, 0.000000000000000000 ) ) ;
#59211 = AXIS2_PLACEMENT_3D ( 'NONE', #120871, #1732, #42991 ) ;
#59212 = ADVANCED_FACE ( 'NONE', ( #41376 ), #75995, .T. ) ;
#59213 = CARTESIAN_POINT ( 'NONE',  ( 5.649999999999932854, 2.500000000000000000, 2.611473670974873151 ) ) ;
#59214 = DIRECTION ( 'NONE',  ( 0.000000000000000000, 0.000000000000000000, 1.000000000000000000 ) ) ;
#59215 = CARTESIAN_POINT ( 'NONE',  ( -2.950000000000029932, 2.500000000000000000, 2.065063509461097624 ) ) ;
#59216 = DIRECTION ( 'NONE',  ( -1.000000000000000000, 0.000000000000000000, 0.000000000000000000 ) ) ;
#59217 = AXIS2_PLACEMENT_3D ( 'NONE', #40902, #104142, #110888 ) ;
#59219 = AXIS2_PLACEMENT_3D ( 'NONE', #75728, #46944, #105193 ) ;
#59218 = CARTESIAN_POINT ( 'NONE',  ( -11.84999999999999787, 12.50000000000000000, -6.841600689897074261 ) ) ;
#59220 = ORIENTED_EDGE ( 'NONE', *, *, #66978, .T. ) ;
#59221 = EDGE_CURVE ( 'NONE', #73869, #38720, #82584, .T. ) ;
#59222 = CIRCLE ( 'NONE', #19480, 0.1000000000000002554 ) ;
#59223 = AXIS2_PLACEMENT_3D ( 'NONE', #5412, #76099, #85268 ) ;
#59224 = DIRECTION ( 'NONE',  ( -0.000000000000000000, -1.000000000000000000, -0.000000000000000000 ) ) ;
#59225 = LINE ( 'NONE', #80137, #78597 ) ;
#59226 = CARTESIAN_POINT ( 'NONE',  ( -7.499999999999976907, 12.50000000000000000, 4.330127018922196314 ) ) ;
#59227 = CIRCLE ( 'NONE', #117664, 0.06509327318403745899 ) ;
#59228 = EDGE_LOOP ( 'NONE', ( #68667, #44382, #90244, #8194 ) ) ;
#59229 = CARTESIAN_POINT ( 'NONE',  ( -3.350000000000031619, 12.50000000000000000, -7.253104124594891289 ) ) ;
#59230 = ORIENTED_EDGE ( 'NONE', *, *, #5389, .F. ) ;
#59231 = AXIS2_PLACEMENT_3D ( 'NONE', #110275, #100456, #19970 ) ;
#59233 = ORIENTED_EDGE ( 'NONE', *, *, #6028, .T. ) ;
#59232 = CONICAL_SURFACE ( 'NONE', #109384, 0.1000000000000002554, 0.003490658503988666988 ) ;
#59234 = AXIS2_PLACEMENT_3D ( 'NONE', #39831, #30002, #127548 ) ;
#59235 = CARTESIAN_POINT ( 'NONE',  ( -8.750000000000010658, 12.50000000000000000, -1.537336459617587581 ) ) ;
#59237 = EDGE_LOOP ( 'NONE', ( #31358, #81980 ) ) ;
#59236 = AXIS2_PLACEMENT_3D ( 'NONE', #65184, #95956, #45579 ) ;
#59238 = CARTESIAN_POINT ( 'NONE',  ( 14.39999999999989555, 12.50000000000000000, 0.3464101615137736845 ) ) ;
#59239 = DIRECTION ( 'NONE',  ( 0.000000000000000000, 1.000000000000000000, 0.000000000000000000 ) ) ;
#59240 = ORIENTED_EDGE ( 'NONE', *, *, #76878, .F. ) ;
#59241 = CARTESIAN_POINT ( 'NONE',  ( -11.05000000000000071, 12.50000000000000000, -6.906693963081112386 ) ) ;
#59242 = VECTOR ( 'NONE', #45601, 1000.000000000000000 ) ;
#59244 = ORIENTED_EDGE ( 'NONE', *, *, #5950, .T. ) ;
#59243 = CARTESIAN_POINT ( 'NONE',  ( -4.600000000000024514, 2.500000000000000000, 0.7928203230275495672 ) ) ;
#59245 = DIRECTION ( 'NONE',  ( 0.000000000000000000, 1.000000000000000000, 0.000000000000000000 ) ) ;
#59246 = DIRECTION ( 'NONE',  ( 0.000000000000000000, 0.000000000000000000, 1.000000000000000000 ) ) ;
#59247 = ORIENTED_EDGE ( 'NONE', *, *, #29899, .F. ) ;
#59249 = ORIENTED_EDGE ( 'NONE', *, *, #44817, .T. ) ;
#59248 = EDGE_CURVE ( 'NONE', #123049, #106610, #51830, .T. ) ;
#59250 = VERTEX_POINT ( 'NONE', #81913 ) ;
#59251 = FACE_OUTER_BOUND ( 'NONE', #74809, .T. ) ;
#59252 = DIRECTION ( 'NONE',  ( 0.000000000000000000, 0.000000000000000000, 1.000000000000000000 ) ) ;
#59254 = LINE ( 'NONE', #39623, #75561 ) ;
#59253 = AXIS2_PLACEMENT_3D ( 'NONE', #59506, #108573, #79128 ) ;
#59255 = FACE_BOUND ( 'NONE', #52169, .T. ) ;
#59256 = ORIENTED_EDGE ( 'NONE', *, *, #9374, .F. ) ;
#59257 = CARTESIAN_POINT ( 'NONE',  ( -6.850000000000017408, 2.500000000000000000, -2.511473670974877948 ) ) ;
#59258 = DIRECTION ( 'NONE',  ( -4.274815082592931898E-19, -0.9999939076577903929, -0.003490651415223739937 ) ) ;
#59259 = ORIENTED_EDGE ( 'NONE', *, *, #47338, .T. ) ;
#59260 = ADVANCED_FACE ( 'NONE', ( #53117 ), #21724, .T. ) ;
#59261 = DIRECTION ( 'NONE',  ( 0.000000000000000000, 0.000000000000000000, 1.000000000000000000 ) ) ;
#59263 = DIRECTION ( 'NONE',  ( 0.000000000000000000, 1.000000000000000000, 0.000000000000000000 ) ) ;
#59262 = AXIS2_PLACEMENT_3D ( 'NONE', #103153, #122798, #105735 ) ;
#59264 = AXIS2_PLACEMENT_3D ( 'NONE', #58777, #88874, #128837 ) ;
#59266 = AXIS2_PLACEMENT_3D ( 'NONE', #83339, #123252, #95729 ) ;
#59265 = LINE ( 'NONE', #30452, #25586 ) ;
#59267 = DIRECTION ( 'NONE',  ( 0.000000000000000000, 0.000000000000000000, 1.000000000000000000 ) ) ;
#59268 = LINE ( 'NONE', #79535, #21536 ) ;
#59269 = FACE_OUTER_BOUND ( 'NONE', #43522, .T. ) ;
#59270 = DIRECTION ( 'NONE',  ( 1.000000000000000000, 0.000000000000000000, 0.000000000000000000 ) ) ;
#59271 = AXIS2_PLACEMENT_3D ( 'NONE', #15046, #5886, #85106 ) ;
#59272 = CIRCLE ( 'NONE', #6994, 0.06509327318403745899 ) ;
#59273 = AXIS2_PLACEMENT_3D ( 'NONE', #101747, #72295, #23832 ) ;
#59274 = VERTEX_POINT ( 'NONE', #74039 ) ;
#59275 = VERTEX_POINT ( 'NONE', #123143 ) ;
#59276 = ORIENTED_EDGE ( 'NONE', *, *, #38790, .F. ) ;
#59277 = EDGE_LOOP ( 'NONE', ( #88909, #65225 ) ) ;
#59279 = ORIENTED_EDGE ( 'NONE', *, *, #81147, .T. ) ;
#59278 = AXIS2_PLACEMENT_3D ( 'NONE', #64601, #5664, #25302 ) ;
#59280 = DIRECTION ( 'NONE',  ( -0.000000000000000000, -1.000000000000000000, -0.000000000000000000 ) ) ;
#59281 = VECTOR ( 'NONE', #100838, 1000.000000000000000 ) ;
#59282 = FACE_OUTER_BOUND ( 'NONE', #75821, .T. ) ;
#59283 = ORIENTED_EDGE ( 'NONE', *, *, #127594, .F. ) ;
#59284 = FACE_BOUND ( 'NONE', #8405, .T. ) ;
#59285 = AXIS2_PLACEMENT_3D ( 'NONE', #123711, #93635, #113924 ) ;
#59286 = CARTESIAN_POINT ( 'NONE',  ( -11.64999999999999680, 2.500000000000000000, 5.902370205355745192 ) ) ;
#59287 = CARTESIAN_POINT ( 'NONE',  ( -4.600000000000024514, 2.500000000000000000, -0.6928203230275542523 ) ) ;
#59288 = FACE_OUTER_BOUND ( 'NONE', #119174, .T. ) ;
#59289 = CARTESIAN_POINT ( 'NONE',  ( -6.250000000000017764, 12.50000000000000000, 2.792790559304612064 ) ) ;
#59290 = CARTESIAN_POINT ( 'NONE',  ( 3.749999999999978684, 2.500000000000000000, -2.265063509461101798 ) ) ;
#59291 = CARTESIAN_POINT ( 'NONE',  ( -4.550000000000022915, 2.500000000000000000, 2.165063509461097713 ) ) ;
#59292 = EDGE_LOOP ( 'NONE', ( #31219, #8249, #128486, #54327 ) ) ;
#59293 = CIRCLE ( 'NONE', #94865, 0.06509327318403745899 ) ;
#59294 = ORIENTED_EDGE ( 'NONE', *, *, #77516, .F. ) ;
#59295 = ADVANCED_FACE ( 'NONE', ( #4622 ), #71912, .T. ) ;
#59296 = VERTEX_POINT ( 'NONE', #121840 ) ;
#59297 = ORIENTED_EDGE ( 'NONE', *, *, #11507, .T. ) ;
#59298 = CARTESIAN_POINT ( 'NONE',  ( 2.500000000000002220, 2.500000000000000000, 9.000000000000003553 ) ) ;
#59299 = DIRECTION ( 'NONE',  ( 0.000000000000000000, 0.000000000000000000, -1.000000000000000000 ) ) ;
#59300 = ORIENTED_EDGE ( 'NONE', *, *, #5669, .T. ) ;
#59301 = DIRECTION ( 'NONE',  ( 0.000000000000000000, 0.000000000000000000, -1.000000000000000000 ) ) ;
#59302 = VECTOR ( 'NONE', #73213, 1000.000000000000000 ) ;
#59303 = AXIS2_PLACEMENT_3D ( 'NONE', #85803, #24318, #83871 ) ;
#59304 = EDGE_CURVE ( 'NONE', #82327, #76656, #42672, .T. ) ;
#59306 = DIRECTION ( 'NONE',  ( 0.000000000000000000, 1.000000000000000000, 0.000000000000000000 ) ) ;
#59305 = VECTOR ( 'NONE', #61653, 1000.000000000000000 ) ;
#59307 = CARTESIAN_POINT ( 'NONE',  ( 4.149999999999939959, 2.500000000000000000, 1.572243186433545548 ) ) ;
#59308 = CARTESIAN_POINT ( 'NONE',  ( 184.1927083336747160, 6.551208109652275624, -3.782341765624998686 ) ) ;
#59309 = DIRECTION ( 'NONE',  ( -0.000000000000000000, 1.000000000000000000, -0.000000000000000000 ) ) ;
#59310 = FACE_OUTER_BOUND ( 'NONE', #103593, .T. ) ;
#59311 = EDGE_CURVE ( 'NONE', #34432, #17665, #124221, .T. ) ;
#59312 = ADVANCED_FACE ( 'NONE', ( #113314 ), #112033, .T. ) ;
#59313 = FACE_OUTER_BOUND ( 'NONE', #76718, .T. ) ;
#59314 = CONICAL_SURFACE ( 'NONE', #76005, 0.1000000000000000472, 0.003490658503988666988 ) ;
#59315 = ADVANCED_FACE ( 'NONE', ( #93678 ), #13811, .T. ) ;
#59316 = ORIENTED_EDGE ( 'NONE', *, *, #106575, .T. ) ;
#59317 = FACE_OUTER_BOUND ( 'NONE', #52671, .T. ) ;
#59318 = AXIS2_PLACEMENT_3D ( 'NONE', #97317, #89427, #119522 ) ;
#59319 = CIRCLE ( 'NONE', #57136, 0.06509327318403745899 ) ;
#59320 = VERTEX_POINT ( 'NONE', #43945 ) ;
#59321 = AXIS2_PLACEMENT_3D ( 'NONE', #112010, #32177, #102187 ) ;
#59322 = ORIENTED_EDGE ( 'NONE', *, *, #121287, .T. ) ;
#59323 = DIRECTION ( 'NONE',  ( -0.000000000000000000, -1.000000000000000000, -0.000000000000000000 ) ) ;
#59324 = EDGE_CURVE ( 'NONE', #100266, #119869, #7125, .T. ) ;
#59325 = CARTESIAN_POINT ( 'NONE',  ( -5.400000000000023448, 12.50000000000000000, -5.022947341949754119 ) ) ;
#59326 = DIRECTION ( 'NONE',  ( -0.000000000000000000, -1.000000000000000000, -0.000000000000000000 ) ) ;
#59327 = EDGE_CURVE ( 'NONE', #21956, #46048, #5076, .T. ) ;
#59328 = AXIS2_PLACEMENT_3D ( 'NONE', #16101, #45604, #56040 ) ;
#59329 = ORIENTED_EDGE ( 'NONE', *, *, #19104, .T. ) ;
#59330 = VERTEX_POINT ( 'NONE', #44581 ) ;
#59331 = CARTESIAN_POINT ( 'NONE',  ( -1.700000000000035261, 12.50000000000000000, 4.395220292106234439 ) ) ;
#59333 = AXIS2_PLACEMENT_3D ( 'NONE', #78725, #30271, #79362 ) ;
#59332 = DIRECTION ( 'NONE',  ( 0.000000000000000000, 0.000000000000000000, -1.000000000000000000 ) ) ;
#59334 = AXIS2_PLACEMENT_3D ( 'NONE', #16121, #56057, #126093 ) ;
#59335 = CARTESIAN_POINT ( 'NONE',  ( 4.799999999999935874, 12.50000000000000000, 3.983716857408420964 ) ) ;
#59336 = ORIENTED_EDGE ( 'NONE', *, *, #7593, .F. ) ;
#59337 = DIRECTION ( 'NONE',  ( 0.000000000000000000, 0.000000000000000000, -1.000000000000000000 ) ) ;
#59338 = CIRCLE ( 'NONE', #44649, 0.09999999999999982514 ) ;
#59339 = VERTEX_POINT ( 'NONE', #83845 ) ;
#59340 = CARTESIAN_POINT ( 'NONE',  ( 12.49999999999990585, 12.50000000000000000, -5.088040615133791356 ) ) ;
#59341 = EDGE_LOOP ( 'NONE', ( #58277, #20826 ) ) ;
#59342 = FACE_OUTER_BOUND ( 'NONE', #57207, .T. ) ;
#59343 = DIRECTION ( 'NONE',  ( -0.000000000000000000, 1.000000000000000000, -0.000000000000000000 ) ) ;
#59344 = DIRECTION ( 'NONE',  ( 0.000000000000000000, 0.000000000000000000, -1.000000000000000000 ) ) ;
#59345 = DIRECTION ( 'NONE',  ( 0.000000000000000000, 1.000000000000000000, 0.000000000000000000 ) ) ;
#59346 = VERTEX_POINT ( 'NONE', #52454 ) ;
#59347 = CARTESIAN_POINT ( 'NONE',  ( 17.50000000000000000, -2.499999999999997335, 4.040567763474973262 ) ) ;
#59348 = ORIENTED_EDGE ( 'NONE', *, *, #2514, .F. ) ;
#59349 = VERTEX_POINT ( 'NONE', #92378 ) ;
#59350 = AXIS2_PLACEMENT_3D ( 'NONE', #122273, #104552, #116287 ) ;
#59351 = AXIS2_PLACEMENT_3D ( 'NONE', #80528, #30791, #70693 ) ;
#59352 = CARTESIAN_POINT ( 'NONE',  ( -8.350000000000012079, 2.500000000000000000, -1.572243186433550211 ) ) ;
#59353 = DIRECTION ( 'NONE',  ( -0.000000000000000000, 1.000000000000000000, -0.000000000000000000 ) ) ;
#59354 = DIRECTION ( 'NONE',  ( -4.274815082592931898E-19, -0.9999939076577903929, -0.003490651415223739937 ) ) ;
#59355 = DIRECTION ( 'NONE',  ( 0.000000000000000000, 0.000000000000000000, -1.000000000000000000 ) ) ;
#59356 = FACE_OUTER_BOUND ( 'NONE', #88141, .T. ) ;
#59357 = CARTESIAN_POINT ( 'NONE',  ( 0.6499999999999561684, 12.50000000000000000, 2.511473670974873507 ) ) ;
#59358 = CIRCLE ( 'NONE', #13255, 0.1000000000000002554 ) ;
#59359 = DIRECTION ( 'NONE',  ( -0.000000000000000000, 1.000000000000000000, -0.000000000000000000 ) ) ;
#59360 = CIRCLE ( 'NONE', #63546, 0.06509327318403741736 ) ;
#59361 = CARTESIAN_POINT ( 'NONE',  ( 11.64999999999990266, 2.500000000000000000, 2.165063509461097713 ) ) ;
#59363 = AXIS2_PLACEMENT_3D ( 'NONE', #100500, #82162, #53352 ) ;
#59362 = CARTESIAN_POINT ( 'NONE',  ( -13.34999999999999076, 2.500000000000000000, -1.372243186433547812 ) ) ;
#59365 = EDGE_CURVE ( 'NONE', #7794, #38720, #80312, .T. ) ;
#59364 = AXIS2_PLACEMENT_3D ( 'NONE', #99598, #9915, #111993 ) ;
#59366 = EDGE_CURVE ( 'NONE', #2388, #75669, #42669, .T. ) ;
#59367 = EDGE_CURVE ( 'NONE', #127628, #55240, #74042, .T. ) ;
#59368 = ADVANCED_FACE ( 'NONE', ( #64212 ), #11348, .T. ) ;
#59369 = CIRCLE ( 'NONE', #82346, 0.06509327318403745899 ) ;
#59370 = CIRCLE ( 'NONE', #126238, 0.06509327318403745899 ) ;
#59371 = CONICAL_SURFACE ( 'NONE', #117812, 0.1000000000000002554, 0.003490658503988666988 ) ;
#59372 = VERTEX_POINT ( 'NONE', #74684 ) ;
#59373 = ADVANCED_FACE ( 'NONE', ( #114593 ), #113764, .T. ) ;
#59374 = DIRECTION ( 'NONE',  ( -0.000000000000000000, -1.000000000000000000, -0.000000000000000000 ) ) ;
#59375 = CIRCLE ( 'NONE', #36381, 0.06509327318403745899 ) ;
#59376 = DIRECTION ( 'NONE',  ( 0.000000000000000000, 1.000000000000000000, 0.000000000000000000 ) ) ;
#59377 = CARTESIAN_POINT ( 'NONE',  ( 184.5000000000000000, 0.000000000000000000, 0.000000000000000000 ) ) ;
#59378 = DIRECTION ( 'NONE',  ( -0.000000000000000000, 1.000000000000000000, -0.000000000000000000 ) ) ;
#59379 = DIRECTION ( 'NONE',  ( 0.000000000000000000, 0.000000000000000000, 1.000000000000000000 ) ) ;
#59380 = VERTEX_POINT ( 'NONE', #55039 ) ;
#59381 = EDGE_CURVE ( 'NONE', #47889, #62993, #104759, .T. ) ;
#59382 = CARTESIAN_POINT ( 'NONE',  ( 1.449999999999951328, 2.500000000000000000, -1.818653347947326138 ) ) ;
#59383 = EDGE_CURVE ( 'NONE', #121302, #108298, #92837, .T. ) ;
#59384 = DIRECTION ( 'NONE',  ( -0.000000000000000000, -1.000000000000000000, -0.000000000000000000 ) ) ;
#59386 = ORIENTED_EDGE ( 'NONE', *, *, #20970, .T. ) ;
#59385 = LINE ( 'NONE', #27963, #86009 ) ;
#59387 =( BOUNDED_SURFACE ( )  B_SPLINE_SURFACE ( 3, 2, ( 
 ( #31075, #3994, #74682 ),
 ( #60538, #114591, #30431 ),
 ( #61157, #93677, #43306 ),
 ( #64209, #103503, #34122 ) ),
 .UNSPECIFIED., .F., .F., .F. ) 
 B_SPLINE_SURFACE_WITH_KNOTS ( ( 4, 4 ),
 ( 3, 3 ),
 ( 0.000000000000000000, 0.002140783231465592188 ),
 ( 0.000000000000000000, 1.000000000000000000 ),
 .UNSPECIFIED. ) 
 GEOMETRIC_REPRESENTATION_ITEM ( )  RATIONAL_B_SPLINE_SURFACE ( (
 ( 1.000000000000000000, 0.7071067811865473507, 1.000000000000000000),
 ( 1.000000000000000000, 0.7083221553718342944, 1.000000000000000000),
 ( 1.000000000000000000, 0.7095583407460057668, 1.000000000000000000),
 ( 1.000000000000000000, 0.7108129114090289136, 1.000000000000000000) ) ) 
 REPRESENTATION_ITEM ( '' )  SURFACE ( )  );
#59388 = ADVANCED_FACE ( 'NONE', ( #126362 ), #84508, .T. ) ;
#59389 = AXIS2_PLACEMENT_3D ( 'NONE', #127012, #6536, #57627 ) ;
#59390 = VERTEX_POINT ( 'NONE', #26871 ) ;
#59391 = CARTESIAN_POINT ( 'NONE',  ( -1.250000000000001554, 12.50000000000000000, 6.495190528383297135 ) ) ;
#59392 = EDGE_LOOP ( 'NONE', ( #100442, #69210, #93766, #112249 ) ) ;
#59393 = EDGE_LOOP ( 'NONE', ( #109278, #63091 ) ) ;
#59394 = EDGE_LOOP ( 'NONE', ( #41365, #11183 ) ) ;
#59395 = DIRECTION ( 'NONE',  ( 0.000000000000000000, 0.000000000000000000, 1.000000000000000000 ) ) ;
#59396 = FACE_OUTER_BOUND ( 'NONE', #120366, .T. ) ;
#59397 = DIRECTION ( 'NONE',  ( -4.274815082592931898E-19, -0.9999939076577903929, -0.003490651415223739937 ) ) ;
#59398 = DIRECTION ( 'NONE',  ( -0.000000000000000000, -1.000000000000000000, -0.000000000000000000 ) ) ;
#59399 = AXIS2_PLACEMENT_3D ( 'NONE', #60225, #39306, #88346 ) ;
#59400 = VERTEX_POINT ( 'NONE', #66780 ) ;
#59401 = DIRECTION ( 'NONE',  ( 0.000000000000000000, 1.000000000000000000, 0.000000000000000000 ) ) ;
#59402 = EDGE_LOOP ( 'NONE', ( #122708, #67360 ) ) ;
#59403 = CARTESIAN_POINT ( 'NONE',  ( 11.89999999999990798, 2.500000000000000000, -3.983716857408426293 ) ) ;
#59404 = DIRECTION ( 'NONE',  ( 0.000000000000000000, 0.000000000000000000, 1.000000000000000000 ) ) ;
#59405 = DIRECTION ( 'NONE',  ( 0.000000000000000000, -0.9999939076577903929, 0.003490651415223739937 ) ) ;
#59406 = VECTOR ( 'NONE', #71803, 1000.000000000000000 ) ;
#59407 = CIRCLE ( 'NONE', #15450, 0.09999999999999999167 ) ;
#59408 = VERTEX_POINT ( 'NONE', #86423 ) ;
#59409 = CIRCLE ( 'NONE', #2958, 0.06509327318403741736 ) ;
#59410 = ORIENTED_EDGE ( 'NONE', *, *, #634, .T. ) ;
#59411 = ORIENTED_EDGE ( 'NONE', *, *, #7037, .T. ) ;
#59412 = ORIENTED_EDGE ( 'NONE', *, *, #40306, .T. ) ;
#59413 = EDGE_LOOP ( 'NONE', ( #102799, #20381 ) ) ;
#59414 = CARTESIAN_POINT ( 'NONE',  ( 4.799999999999937650, 12.50000000000000000, -0.3464101615137782364 ) ) ;
#59415 = DIRECTION ( 'NONE',  ( 0.000000000000000000, 0.000000000000000000, -1.000000000000000000 ) ) ;
#59416 = DIRECTION ( 'NONE',  ( 0.000000000000000000, -0.000000000000000000, 1.000000000000000000 ) ) ;
#59417 = FACE_BOUND ( 'NONE', #115439, .T. ) ;
#59418 = CARTESIAN_POINT ( 'NONE',  ( -9.800000000000007816, 12.50000000000000000, -3.983716857408421852 ) ) ;
#59419 = CARTESIAN_POINT ( 'NONE',  ( 5.599999999999933031, 12.50000000000000000, 0.4115034346978109769 ) ) ;
#59420 = DIRECTION ( 'NONE',  ( 0.000000000000000000, 0.000000000000000000, 1.000000000000000000 ) ) ;
#59421 = CARTESIAN_POINT ( 'NONE',  ( -1.900000000000034994, 2.500000000000000000, -0.3464101615137783474 ) ) ;
#59422 = EDGE_CURVE ( 'NONE', #22780, #29957, #103298, .T. ) ;
#59423 = CONICAL_SURFACE ( 'NONE', #23902, 0.09999999999999982514, 0.003490658503988666988 ) ;
#59424 = VECTOR ( 'NONE', #100774, 1000.000000000000000 ) ;
#59425 = CIRCLE ( 'NONE', #74061, 0.09999999999999982514 ) ;
#59426 = DIRECTION ( 'NONE',  ( 0.000000000000000000, 1.000000000000000000, 0.000000000000000000 ) ) ;
#59427 = CARTESIAN_POINT ( 'NONE',  ( 179.5000000000000000, 1.375000000000002442, -6.000000000000000888 ) ) ;
#59428 = AXIS2_PLACEMENT_3D ( 'NONE', #7404, #39490, #98364 ) ;
#59429 = DIRECTION ( 'NONE',  ( 0.000000000000000000, 0.000000000000000000, -1.000000000000000000 ) ) ;
#59430 = CIRCLE ( 'NONE', #40653, 0.1000000000000002554 ) ;
#59431 = DIRECTION ( 'NONE',  ( 0.000000000000000000, 0.000000000000000000, -1.000000000000000000 ) ) ;
#59432 = ORIENTED_EDGE ( 'NONE', *, *, #126252, .T. ) ;
#59433 = ORIENTED_EDGE ( 'NONE', *, *, #47155, .F. ) ;
#59434 = VERTEX_POINT ( 'NONE', #87711 ) ;
#59435 = ORIENTED_EDGE ( 'NONE', *, *, #105991, .F. ) ;
#59436 = DIRECTION ( 'NONE',  ( 0.000000000000000000, 0.000000000000000000, 1.000000000000000000 ) ) ;
#59437 = DIRECTION ( 'NONE',  ( 0.000000000000000000, 1.000000000000000000, 0.000000000000000000 ) ) ;
#59438 = FACE_BOUND ( 'NONE', #127993, .T. ) ;
#59439 = CARTESIAN_POINT ( 'NONE',  ( -3.100000000000028511, 12.50000000000000000, -3.983716857408426293 ) ) ;
#59440 = CIRCLE ( 'NONE', #44852, 0.06509327318403745899 ) ;
#59442 = VERTEX_POINT ( 'NONE', #17005 ) ;
#59441 = AXIS2_PLACEMENT_3D ( 'NONE', #95379, #105837, #67168 ) ;
#59444 = CIRCLE ( 'NONE', #15489, 0.06509327318403745899 ) ;
#59443 = FACE_OUTER_BOUND ( 'NONE', #99516, .T. ) ;
#59445 = PLANE ( 'NONE',  #28628 ) ;
#59446 = DIRECTION ( 'NONE',  ( 0.000000000000000000, 0.000000000000000000, 1.000000000000000000 ) ) ;
#59447 = DIRECTION ( 'NONE',  ( -0.000000000000000000, 1.000000000000000000, -0.000000000000000000 ) ) ;
#59448 = ORIENTED_EDGE ( 'NONE', *, *, #65791, .F. ) ;
#59449 = DIRECTION ( 'NONE',  ( -0.000000000000000000, -1.000000000000000000, -0.000000000000000000 ) ) ;
#59450 = VECTOR ( 'NONE', #108148, 1000.000000000000000 ) ;
#59451 = AXIS2_PLACEMENT_3D ( 'NONE', #69140, #10850, #9595 ) ;
#59452 = VECTOR ( 'NONE', #51445, 1000.000000000000000 ) ;
#59454 = ORIENTED_EDGE ( 'NONE', *, *, #104769, .T. ) ;
#59453 = AXIS2_PLACEMENT_3D ( 'NONE', #9242, #89729, #60911 ) ;
#59455 = ORIENTED_EDGE ( 'NONE', *, *, #10115, .F. ) ;
#59456 = DIRECTION ( 'NONE',  ( 0.000000000000000000, 0.000000000000000000, -1.000000000000000000 ) ) ;
#59457 = CARTESIAN_POINT ( 'NONE',  ( 9.199999999999919353, 2.500000000000000000, -2.276824562219559311E-15 ) ) ;
#59458 = ORIENTED_EDGE ( 'NONE', *, *, #40242, .F. ) ;
#59459 = CIRCLE ( 'NONE', #25694, 0.1000000000000002554 ) ;
#59460 = AXIS2_PLACEMENT_3D ( 'NONE', #27428, #107935, #17613 ) ;
#59462 = EDGE_CURVE ( 'NONE', #115836, #105649, #86556, .T. ) ;
#59461 = VECTOR ( 'NONE', #107386, 1000.000000000000000 ) ;
#59463 = CARTESIAN_POINT ( 'NONE',  ( 2.499999999999983569, 2.500000000000000000, -4.330127018922201643 ) ) ;
#59464 = DIRECTION ( 'NONE',  ( 0.000000000000000000, 0.000000000000000000, -1.000000000000000000 ) ) ;
#59465 = VERTEX_POINT ( 'NONE', #36054 ) ;
#59466 = CARTESIAN_POINT ( 'NONE',  ( 9.349999999999916156, 12.50000000000000000, -1.753560074763288679 ) ) ;
#59468 = ORIENTED_EDGE ( 'NONE', *, *, #2589, .T. ) ;
#59467 = AXIS2_PLACEMENT_3D ( 'NONE', #31979, #129549, #9748 ) ;
#59469 = EDGE_CURVE ( 'NONE', #97052, #6303, #884, .T. ) ;
#59470 = PLANE ( 'NONE',  #57911 ) ;
#59471 = ADVANCED_FACE ( 'NONE', ( #15745 ), #126278, .T. ) ;
#59472 = EDGE_LOOP ( 'NONE', ( #69974, #63110 ) ) ;
#59473 = DIRECTION ( 'NONE',  ( 0.000000000000000000, 0.000000000000000000, 1.000000000000000000 ) ) ;
#59474 = FACE_BOUND ( 'NONE', #45580, .T. ) ;
#59475 = ORIENTED_EDGE ( 'NONE', *, *, #51530, .T. ) ;
#59476 = CARTESIAN_POINT ( 'NONE',  ( 6.699999999999930012, 2.500000000000000000, 4.430127018922196847 ) ) ;
#59477 = ORIENTED_EDGE ( 'NONE', *, *, #40414, .F. ) ;
#59478 = FACE_OUTER_BOUND ( 'NONE', #90374, .T. ) ;
#59479 = DIRECTION ( 'NONE',  ( 1.000000000000000000, 0.000000000000000000, 0.000000000000000000 ) ) ;
#59480 = EDGE_CURVE ( 'NONE', #108547, #26951, #96891, .T. ) ;
#59481 = ADVANCED_FACE ( 'NONE', ( #77890 ), #46861, .T. ) ;
#59482 = DIRECTION ( 'NONE',  ( -0.000000000000000000, -1.000000000000000000, -0.000000000000000000 ) ) ;
#59483 = EDGE_CURVE ( 'NONE', #35498, #109299, #55681, .T. ) ;
#59484 = CARTESIAN_POINT ( 'NONE',  ( -5.200000000000022382, 12.50000000000000000, 0.4115034346978109769 ) ) ;
#59485 = ADVANCED_FACE ( 'NONE', ( #7863 ), #17593, .T. ) ;
#59486 = EDGE_CURVE ( 'NONE', #5786, #12706, #96239, .T. ) ;
#59487 = LINE ( 'NONE', #39195, #3527 ) ;
#59488 = VECTOR ( 'NONE', #15852, 1000.000000000000000 ) ;
#59489 = EDGE_LOOP ( 'NONE', ( #18277, #57732, #92641, #4978 ) ) ;
#59490 = VERTEX_POINT ( 'NONE', #67406 ) ;
#59491 = ORIENTED_EDGE ( 'NONE', *, *, #98930, .T. ) ;
#59492 = DIRECTION ( 'NONE',  ( -0.000000000000000000, 1.000000000000000000, -0.000000000000000000 ) ) ;
#59493 = PLANE ( 'NONE',  #5546 ) ;
#59494 = DIRECTION ( 'NONE',  ( -4.274815082592931898E-19, -0.9999939076577903929, -0.003490651415223739937 ) ) ;
#59496 = VERTEX_POINT ( 'NONE', #115889 ) ;
#59495 = ORIENTED_EDGE ( 'NONE', *, *, #13017, .F. ) ;
#59497 = ORIENTED_EDGE ( 'NONE', *, *, #107139, .T. ) ;
#59498 = EDGE_CURVE ( 'NONE', #70678, #76293, #61532, .T. ) ;
#59499 = CARTESIAN_POINT ( 'NONE',  ( -4.150000000000024336, 2.500000000000000000, -2.957883832488653830 ) ) ;
#59500 = AXIS2_PLACEMENT_3D ( 'NONE', #105788, #26588, #65855 ) ;
#59501 = DIRECTION ( 'NONE',  ( -0.000000000000000000, 1.000000000000000000, -0.000000000000000000 ) ) ;
#59502 = ITEM_DEFINED_TRANSFORMATION ( 'NONE', 'NONE', #38001,  #108296 ) ;
#59503 = FACE_OUTER_BOUND ( 'NONE', #83171, .T. ) ;
#59504 = CARTESIAN_POINT ( 'NONE',  ( 8.749999999999920064, 12.50000000000000000, -2.857883832488653741 ) ) ;
#59505 = CARTESIAN_POINT ( 'NONE',  ( -10.60000000000000320, 12.50000000000000000, -3.983716857408421852 ) ) ;
#59506 = CARTESIAN_POINT ( 'NONE',  ( 0.5999999999999555689, 12.50000000000000000, 4.676537180435972552 ) ) ;
#59507 = CARTESIAN_POINT ( 'NONE',  ( -12.89999999999999147, 12.50000000000000000, 1.843143693225357538E-15 ) ) ;
#59508 = ORIENTED_EDGE ( 'NONE', *, *, #72228, .T. ) ;
#59509 = ORIENTED_EDGE ( 'NONE', *, *, #110417, .T. ) ;
#59510 = AXIS2_PLACEMENT_3D ( 'NONE', #103653, #23801, #22530 ) ;
#59511 = DIRECTION ( 'NONE',  ( 0.000000000000000000, 1.000000000000000000, 0.000000000000000000 ) ) ;
#59512 = AXIS2_PLACEMENT_3D ( 'NONE', #64868, #113989, #17027 ) ;
#59513 = DIRECTION ( 'NONE',  ( -0.000000000000000000, -1.000000000000000000, -0.000000000000000000 ) ) ;
#59514 = ORIENTED_EDGE ( 'NONE', *, *, #17923, .T. ) ;
#59515 = ORIENTED_EDGE ( 'NONE', *, *, #73148, .T. ) ;
#59516 = CARTESIAN_POINT ( 'NONE',  ( 185.5260416670080588, -6.551208109652273848, -3.782341765625003571 ) ) ;
#59517 = DIRECTION ( 'NONE',  ( 0.000000000000000000, 0.000000000000000000, -1.000000000000000000 ) ) ;
#59518 = DIRECTION ( 'NONE',  ( 0.000000000000000000, 0.000000000000000000, -1.000000000000000000 ) ) ;
#59519 = DIRECTION ( 'NONE',  ( -0.000000000000000000, -1.000000000000000000, -0.000000000000000000 ) ) ;
#59520 = CIRCLE ( 'NONE', #7232, 0.1000000000000000472 ) ;
#59521 = CARTESIAN_POINT ( 'NONE',  ( 4.399999999999939071, 2.500000000000000000, -0.3464101615137782364 ) ) ;
#59522 = CONICAL_SURFACE ( 'NONE', #53242, 0.1000000000000000056, 0.003490658503988666988 ) ;
#59523 = PLANE ( 'NONE',  #122152 ) ;
#59524 = DIRECTION ( 'NONE',  ( 0.000000000000000000, 0.000000000000000000, -1.000000000000000000 ) ) ;
#59525 = AXIS2_PLACEMENT_3D ( 'NONE', #125108, #5958, #34158 ) ;
#59526 = ADVANCED_FACE ( 'NONE', ( #75318 ), #90759, .T. ) ;
#59527 = ADVANCED_FACE ( 'NONE', ( #107361 ), #95614, .T. ) ;
#59528 = CARTESIAN_POINT ( 'NONE',  ( -8.300000000000011369, 2.500000000000000000, -4.430127018922202176 ) ) ;
#59529 = ORIENTED_EDGE ( 'NONE', *, *, #54994, .T. ) ;
#59530 = EDGE_CURVE ( 'NONE', #33059, #10801, #65627, .T. ) ;
#59531 = ORIENTED_EDGE ( 'NONE', *, *, #107367, .F. ) ;
#59532 = VERTEX_POINT ( 'NONE', #119120 ) ;
#59533 = EDGE_CURVE ( 'NONE', #21628, #82736, #69839, .T. ) ;
#59534 = EDGE_LOOP ( 'NONE', ( #93122, #36432 ) ) ;
#59535 = FACE_OUTER_BOUND ( 'NONE', #115308, .T. ) ;
#59536 = CARTESIAN_POINT ( 'NONE',  ( -6.050000000000018474, 2.500000000000000000, 6.841600689897072485 ) ) ;
#59537 = EDGE_CURVE ( 'NONE', #35519, #1307, #5816, .T. ) ;
#59538 = VERTEX_POINT ( 'NONE', #70026 ) ;
#59539 = ADVANCED_FACE ( 'NONE', ( #1275 ), #78354, .T. ) ;
#59540 = CARTESIAN_POINT ( 'NONE',  ( 7.049999999999928768, 2.500000000000000000, -2.265063509461101798 ) ) ;
#59541 = DIRECTION ( 'NONE',  ( -4.274815082592931898E-19, -0.9999939076577903929, -0.003490651415223739937 ) ) ;
#59542 = ADVANCED_FACE ( 'NONE', ( #58276 ), #79831, .T. ) ;
#59543 = AXIS2_PLACEMENT_3D ( 'NONE', #56881, #87009, #65432 ) ;
#59544 = CIRCLE ( 'NONE', #78398, 0.06509327318403745899 ) ;
#59545 = LINE ( 'NONE', #9766, #42829 ) ;
#59547 = EDGE_LOOP ( 'NONE', ( #43860, #112434 ) ) ;
#59546 = CARTESIAN_POINT ( 'NONE',  ( 10.84999999999991260, 2.500000000000000000, 6.395190528383296602 ) ) ;
#59548 = AXIS2_PLACEMENT_3D ( 'NONE', #48066, #119363, #67682 ) ;
#59549 = AXIS2_PLACEMENT_3D ( 'NONE', #87439, #118201, #48833 ) ;
#59550 = DIRECTION ( 'NONE',  ( 0.000000000000000000, 0.000000000000000000, 1.000000000000000000 ) ) ;
#59551 = EDGE_CURVE ( 'NONE', #11954, #74899, #105440, .T. ) ;
#59552 = DIRECTION ( 'NONE',  ( 0.000000000000000000, 0.000000000000000000, -1.000000000000000000 ) ) ;
#59553 = VERTEX_POINT ( 'NONE', #48441 ) ;
#59554 = CONICAL_SURFACE ( 'NONE', #72051, 0.09999999999999982514, 0.003490658503988666988 ) ;
#59555 = CONICAL_SURFACE ( 'NONE', #24017, 0.09999999999999982514, 0.003490658503988666988 ) ;
#59556 = AXIS2_PLACEMENT_3D ( 'NONE', #87946, #106952, #17264 ) ;
#59557 = ORIENTED_EDGE ( 'NONE', *, *, #96781, .T. ) ;
#59558 = ORIENTED_EDGE ( 'NONE', *, *, #28440, .T. ) ;
#59559 = ORIENTED_EDGE ( 'NONE', *, *, #63851, .T. ) ;
#59560 = DIRECTION ( 'NONE',  ( -0.000000000000000000, -1.000000000000000000, -0.000000000000000000 ) ) ;
#59561 = DIRECTION ( 'NONE',  ( 0.000000000000000000, 0.000000000000000000, -1.000000000000000000 ) ) ;
#59562 = CONICAL_SURFACE ( 'NONE', #80476, 0.1000000000000002554, 0.003490658503988666988 ) ;
#59563 = CIRCLE ( 'NONE', #42836, 0.09999999999999982514 ) ;
#59564 = VECTOR ( 'NONE', #90068, 1000.000000000000000 ) ;
#59565 = ORIENTED_EDGE ( 'NONE', *, *, #98739, .T. ) ;
#59566 = LINE ( 'NONE', #90926, #41221 ) ;
#59567 = CARTESIAN_POINT ( 'NONE',  ( -4.150000000000027889, 12.50000000000000000, -6.495190528383302464 ) ) ;
#59568 = CARTESIAN_POINT ( 'NONE',  ( -12.49999999999995737, 2.500000000000000000, 4.230127018922196669 ) ) ;
#59569 = DIRECTION ( 'NONE',  ( -0.000000000000000000, -1.000000000000000000, -0.000000000000000000 ) ) ;
#59570 = EDGE_CURVE ( 'NONE', #55527, #95554, #80409, .T. ) ;
#59571 = EDGE_LOOP ( 'NONE', ( #58075, #75522, #4738, #41900 ) ) ;
#59572 = DIRECTION ( 'NONE',  ( 0.000000000000000000, -0.9999939076577903929, 0.003490651415223739937 ) ) ;
#59573 = VERTEX_POINT ( 'NONE', #81139 ) ;
#59574 = EDGE_LOOP ( 'NONE', ( #32147, #115219, #106934, #27579 ) ) ;
#59575 = CARTESIAN_POINT ( 'NONE',  ( -2.950000000000030376, 12.50000000000000000, 6.495190528383297135 ) ) ;
#59576 = DIRECTION ( 'NONE',  ( 0.000000000000000000, 0.000000000000000000, 1.000000000000000000 ) ) ;
#59577 = FACE_BOUND ( 'NONE', #85920, .T. ) ;
#59578 = CARTESIAN_POINT ( 'NONE',  ( -6.505213034913026604E-15, 2.500000000000000000, 4.430127018922196847 ) ) ;
#59579 = CIRCLE ( 'NONE', #45077, 0.1000000000000000472 ) ;
#59580 = DIRECTION ( 'NONE',  ( 0.000000000000000000, -0.9999939076577903929, 0.003490651415223739937 ) ) ;
#59581 = CARTESIAN_POINT ( 'NONE',  ( 3.299999999999942979, 12.50000000000000000, 4.265033745738159077 ) ) ;
#59582 = ADVANCED_FACE ( 'NONE', ( #89662 ), #111698, .T. ) ;
#59583 = VERTEX_POINT ( 'NONE', #59587 ) ;
#59584 = CARTESIAN_POINT ( 'NONE',  ( -3.550000000000028244, 2.500000000000000000, -1.818653347947326138 ) ) ;
#59585 = DIRECTION ( 'NONE',  ( -0.000000000000000000, -1.000000000000000000, -0.000000000000000000 ) ) ;
#59586 = DIRECTION ( 'NONE',  ( 0.000000000000000000, 1.000000000000000000, 0.000000000000000000 ) ) ;
#59587 = CARTESIAN_POINT ( 'NONE',  ( 6.649999999999931966, 2.500000000000000000, -7.088010851410853519 ) ) ;
#59588 = ORIENTED_EDGE ( 'NONE', *, *, #113424, .T. ) ;
#59589 = CIRCLE ( 'NONE', #76279, 0.06509327318403745899 ) ;
#59590 = AXIS2_PLACEMENT_3D ( 'NONE', #112375, #3695, #2385 ) ;
#59591 = DIRECTION ( 'NONE',  ( -0.000000000000000000, -1.000000000000000000, -0.000000000000000000 ) ) ;
#59592 = DIRECTION ( 'NONE',  ( -0.000000000000000000, -1.000000000000000000, -0.000000000000000000 ) ) ;
#59593 = ORIENTED_EDGE ( 'NONE', *, *, #34857, .T. ) ;
#59594 = VERTEX_POINT ( 'NONE', #119759 ) ;
#59595 = DIRECTION ( 'NONE',  ( 0.000000000000000000, 1.000000000000000000, 0.000000000000000000 ) ) ;
#59596 = EDGE_CURVE ( 'NONE', #36965, #6322, #92926, .T. ) ;
#59597 = CARTESIAN_POINT ( 'NONE',  ( -12.09999999999999609, 2.500000000000000000, -4.230127018922199333 ) ) ;
#59598 = FACE_BOUND ( 'NONE', #11063, .T. ) ;
#59599 = CARTESIAN_POINT ( 'NONE',  ( -14.14999999999998792, 2.500000000000000000, 2.857883832488652853 ) ) ;
#59600 = AXIS2_PLACEMENT_3D ( 'NONE', #4772, #93192, #114741 ) ;
#59601 = DIRECTION ( 'NONE',  ( 0.000000000000000000, -0.9999939076577903929, 0.003490651415223739937 ) ) ;
#59602 = AXIS2_PLACEMENT_3D ( 'NONE', #51700, #122374, #71316 ) ;
#59603 = ORIENTED_EDGE ( 'NONE', *, *, #90237, .T. ) ;
#59604 = DIRECTION ( 'NONE',  ( -0.000000000000000000, 1.000000000000000000, -0.000000000000000000 ) ) ;
#59605 = CARTESIAN_POINT ( 'NONE',  ( 184.2083333333333144, -4.445597072760115509, -7.700000000000001954 ) ) ;
#59606 = ORIENTED_EDGE ( 'NONE', *, *, #46619, .F. ) ;
#59607 = LINE ( 'NONE', #117174, #44777 ) ;
#59608 = DIRECTION ( 'NONE',  ( 0.000000000000000000, 0.000000000000000000, 1.000000000000000000 ) ) ;
#59609 = AXIS2_PLACEMENT_3D ( 'NONE', #120416, #44919, #114288 ) ;
#59610 = VECTOR ( 'NONE', #21263, 1000.000000000000000 ) ;
#59611 = DIRECTION ( 'NONE',  ( 0.000000000000000000, -0.000000000000000000, 1.000000000000000000 ) ) ;
#59612 = CARTESIAN_POINT ( 'NONE',  ( -6.850000000000013856, 2.500000000000000000, 2.611473670974873151 ) ) ;
#59613 = VERTEX_POINT ( 'NONE', #51041 ) ;
#59614 = ADVANCED_FACE ( 'NONE', ( #99492 ), #26025, .T. ) ;
#59615 =( NAMED_UNIT ( * ) SI_UNIT ( $, .STERADIAN. ) SOLID_ANGLE_UNIT ( ) );
#59616 = CARTESIAN_POINT ( 'NONE',  ( -10.85000000000000142, 12.50000000000000000, -7.122917578226813262 ) ) ;
#59617 = CARTESIAN_POINT ( 'NONE',  ( -5.850000000000019185, 12.50000000000000000, 6.495190528383297135 ) ) ;
#59618 = DIRECTION ( 'NONE',  ( 0.000000000000000000, 0.000000000000000000, -1.000000000000000000 ) ) ;
#59619 = EDGE_LOOP ( 'NONE', ( #32213, #85282 ) ) ;
#59620 = ORIENTED_EDGE ( 'NONE', *, *, #70368, .T. ) ;
#59621 = PLANE ( 'NONE',  #118314 ) ;
#59622 = CONICAL_SURFACE ( 'NONE', #49151, 0.09999999999999982514, 0.003490658503988666988 ) ;
#59623 = ORIENTED_EDGE ( 'NONE', *, *, #25323, .T. ) ;
#59624 = DIRECTION ( 'NONE',  ( 0.000000000000000000, 1.000000000000000000, 0.000000000000000000 ) ) ;
#59625 = PLANE ( 'NONE',  #49497 ) ;
#59627 = DIRECTION ( 'NONE',  ( 0.000000000000000000, 0.000000000000000000, 1.000000000000000000 ) ) ;
#59626 = CIRCLE ( 'NONE', #70065, 0.1000000000000002554 ) ;
#59628 = VERTEX_POINT ( 'NONE', #18969 ) ;
#59629 = CARTESIAN_POINT ( 'NONE',  ( 13.94999999999989448, 12.50000000000000000, -2.576566944158915184 ) ) ;
#59630 = DIRECTION ( 'NONE',  ( 0.000000000000000000, 0.000000000000000000, 1.000000000000000000 ) ) ;
#59631 = LINE ( 'NONE', #128369, #102860 ) ;
#59632 = EDGE_CURVE ( 'NONE', #45780, #31546, #15534, .T. ) ;
#59633 = EDGE_CURVE ( 'NONE', #106056, #105502, #49757, .T. ) ;
#59634 = CARTESIAN_POINT ( 'NONE',  ( 88.00000000000001421, 0.000000000000000000, 0.000000000000000000 ) ) ;
#59635 = CARTESIAN_POINT ( 'NONE',  ( -9.800000000000006040, 2.500000000000000000, -4.576537180435973795 ) ) ;
#59636 = EDGE_CURVE ( 'NONE', #88688, #72798, #21830, .T. ) ;
#59637 = EDGE_CURVE ( 'NONE', #25624, #95786, #50376, .T. ) ;
#59638 = DIRECTION ( 'NONE',  ( 0.000000000000000000, -0.000000000000000000, 1.000000000000000000 ) ) ;
#59639 = AXIS2_PLACEMENT_3D ( 'NONE', #91842, #128057, #1512 ) ;
#59640 = ORIENTED_EDGE ( 'NONE', *, *, #75384, .T. ) ;
#59642 = ORIENTED_EDGE ( 'NONE', *, *, #83433, .F. ) ;
#59641 = CIRCLE ( 'NONE', #103527, 0.06509327318403745899 ) ;
#59644 = FACE_OUTER_BOUND ( 'NONE', #99707, .T. ) ;
#59643 = AXIS2_PLACEMENT_3D ( 'NONE', #68168, #88449, #7308 ) ;
#59645 = VERTEX_POINT ( 'NONE', #121047 ) ;
#59646 = CARTESIAN_POINT ( 'NONE',  ( 105.7578401975872282, 6.263922221111824840, 4.480854580342004567 ) ) ;
#59649 = ORIENTED_EDGE ( 'NONE', *, *, #95607, .T. ) ;
#59648 = VERTEX_POINT ( 'NONE', #80501 ) ;
#59647 = AXIS2_PLACEMENT_3D ( 'NONE', #45041, #103308, #14882 ) ;
#59650 = ORIENTED_EDGE ( 'NONE', *, *, #33077, .T. ) ;
#59651 = ADVANCED_FACE ( 'NONE', ( #120414 ), #36503, .T. ) ;
#59652 = CARTESIAN_POINT ( 'NONE',  ( 87.49999999999998579, 1.433398978532516743, -7.395196794792771477 ) ) ;
#59653 = ADVANCED_FACE ( 'NONE', ( #33341 ), #31398, .T. ) ;
#59654 = AXIS2_PLACEMENT_3D ( 'NONE', #45509, #4251, #73646 ) ;
#59656 = AXIS2_PLACEMENT_3D ( 'NONE', #125272, #8064, #95169 ) ;
#59655 = DIRECTION ( 'NONE',  ( -0.000000000000000000, 1.000000000000000000, -0.000000000000000000 ) ) ;
#59657 = EDGE_CURVE ( 'NONE', #79041, #93285, #82464, .T. ) ;
#59658 = CARTESIAN_POINT ( 'NONE',  ( -0.8000000000000315747, 12.50000000000000000, 0.06509327318403743123 ) ) ;
#59659 = DIRECTION ( 'NONE',  ( -0.000000000000000000, -1.000000000000000000, -0.000000000000000000 ) ) ;
#59660 = CARTESIAN_POINT ( 'NONE',  ( 12.29999999999990656, 2.500000000000000000, -4.776537180435977525 ) ) ;
#59661 = CARTESIAN_POINT ( 'NONE',  ( 6.049999999999935874, 12.50000000000000000, -6.906693963081115051 ) ) ;
#59662 = CIRCLE ( 'NONE', #111861, 0.06509327318403745899 ) ;
#59663 = DIRECTION ( 'NONE',  ( 0.000000000000000000, 0.000000000000000000, 1.000000000000000000 ) ) ;
#59664 = LINE ( 'NONE', #128392, #3004 ) ;
#59665 = CARTESIAN_POINT ( 'NONE',  ( -5.800000000000022027, 2.500000000000000000, -4.230127018922201998 ) ) ;
#59666 = ORIENTED_EDGE ( 'NONE', *, *, #3046, .T. ) ;
#59667 = EDGE_LOOP ( 'NONE', ( #64119, #49892 ) ) ;
#59668 = DIRECTION ( 'NONE',  ( -0.000000000000000000, -1.000000000000000000, -0.000000000000000000 ) ) ;
#59669 = ORIENTED_EDGE ( 'NONE', *, *, #97851, .F. ) ;
#59670 = EDGE_LOOP ( 'NONE', ( #8367, #110890 ) ) ;
#59671 = DIRECTION ( 'NONE',  ( -4.274815082592931898E-19, -0.9999939076577903929, -0.003490651415223739937 ) ) ;
#59672 = CARTESIAN_POINT ( 'NONE',  ( -4.200000000000025935, 12.50000000000000000, 4.395220292106234439 ) ) ;
#59673 = DIRECTION ( 'NONE',  ( -0.000000000000000000, -1.000000000000000000, -0.000000000000000000 ) ) ;
#59674 = DIRECTION ( 'NONE',  ( 0.000000000000000000, 1.000000000000000000, 0.000000000000000000 ) ) ;
#59675 = DIRECTION ( 'NONE',  ( 0.000000000000000000, 0.000000000000000000, 1.000000000000000000 ) ) ;
#59676 = ORIENTED_EDGE ( 'NONE', *, *, #122145, .F. ) ;
#59677 = AXIS2_PLACEMENT_3D ( 'NONE', #13858, #74724, #123807 ) ;
#59678 = VECTOR ( 'NONE', #111565, 1000.000000000000000 ) ;
#59679 = EDGE_LOOP ( 'NONE', ( #73629, #125948, #18140, #36036 ) ) ;
#59680 = DIRECTION ( 'NONE',  ( 0.000000000000000000, 0.000000000000000000, 1.000000000000000000 ) ) ;
#59681 = ORIENTED_EDGE ( 'NONE', *, *, #40293, .T. ) ;
#59682 = CARTESIAN_POINT ( 'NONE',  ( 1.449999999999951328, 2.500000000000000000, 2.511473670974873507 ) ) ;
#59683 = EDGE_LOOP ( 'NONE', ( #122723, #69065 ) ) ;
#59684 = EDGE_CURVE ( 'NONE', #29124, #50358, #44420, .T. ) ;
#59685 = ORIENTED_EDGE ( 'NONE', *, *, #85425, .F. ) ;
#59686 = DIRECTION ( 'NONE',  ( 0.000000000000000000, -0.000000000000000000, 1.000000000000000000 ) ) ;
#59687 = CARTESIAN_POINT ( 'NONE',  ( -2.500000000000030642, 2.500000000000000000, -5.122947341949753763 ) ) ;
#59688 = AXIS2_PLACEMENT_3D ( 'NONE', #83834, #11873, #102822 ) ;
#59689 = ADVANCED_FACE ( 'NONE', ( #93526 ), #84350, .T. ) ;
#59690 = CARTESIAN_POINT ( 'NONE',  ( -7.500000000000001776, 1.500000000000000000, -8.999999999999998224 ) ) ;
#59691 = LINE ( 'NONE', #6653, #109211 ) ;
#59693 = ADVANCED_FACE ( 'NONE', ( #83074 ), #109645, .T. ) ;
#59692 = AXIS2_PLACEMENT_3D ( 'NONE', #16095, #64569, #44946 ) ;
#59694 = DIRECTION ( 'NONE',  ( -4.274815082592931898E-19, -0.9999939076577903929, -0.003490651415223739937 ) ) ;
#59695 = VERTEX_POINT ( 'NONE', #82438 ) ;
#59696 = CARTESIAN_POINT ( 'NONE',  ( 8.549999999999922551, 12.50000000000000000, -6.148780366869526226 ) ) ;
#59697 = DIRECTION ( 'NONE',  ( 0.000000000000000000, 0.000000000000000000, 1.000000000000000000 ) ) ;
#59698 = DIRECTION ( 'NONE',  ( -0.000000000000000000, -1.000000000000000000, -0.000000000000000000 ) ) ;
#59699 = DIRECTION ( 'NONE',  ( 0.000000000000000000, 1.000000000000000000, 0.000000000000000000 ) ) ;
#59700 = ADVANCED_FACE ( 'NONE', ( #92221 ), #78264, .T. ) ;
#59701 = DIRECTION ( 'NONE',  ( -4.274815082592931898E-19, -0.9999939076577903929, -0.003490651415223739937 ) ) ;
#59702 = VERTEX_POINT ( 'NONE', #102688 ) ;
#59703 = CONICAL_SURFACE ( 'NONE', #76404, 0.1000000000000000056, 0.003490658503988666988 ) ;
#59704 = AXIS2_PLACEMENT_3D ( 'NONE', #12572, #82631, #61038 ) ;
#59705 = ORIENTED_EDGE ( 'NONE', *, *, #119741, .F. ) ;
#59706 = DIRECTION ( 'NONE',  ( 0.000000000000000000, -0.9999939076577903929, 0.003490651415223739937 ) ) ;
#59707 = EDGE_LOOP ( 'NONE', ( #16567, #28715 ) ) ;
#59708 = CARTESIAN_POINT ( 'NONE',  ( 17.50000000000010658, -2.262047038896518369, 3.993694673355226321 ) ) ;
#59709 = CARTESIAN_POINT ( 'NONE',  ( 11.24999999999990585, 2.500000000000000000, 2.857883832488649301 ) ) ;
#59710 = AXIS2_PLACEMENT_3D ( 'NONE', #11633, #41763, #111096 ) ;
#59711 = ORIENTED_EDGE ( 'NONE', *, *, #108203, .T. ) ;
#59712 = CARTESIAN_POINT ( 'NONE',  ( 0.6499999999999561684, 2.500000000000000000, -2.511473670974877948 ) ) ;
#59713 = DIRECTION ( 'NONE',  ( 0.000000000000000000, 0.000000000000000000, -1.000000000000000000 ) ) ;
#59714 = CARTESIAN_POINT ( 'NONE',  ( 5.449999999999936229, 12.50000000000000000, -2.165063509461101710 ) ) ;
#59715 = AXIS2_PLACEMENT_3D ( 'NONE', #96164, #88936, #88262 ) ;
#59716 = FACE_OUTER_BOUND ( 'NONE', #75704, .T. ) ;
#59717 = CIRCLE ( 'NONE', #95383, 0.06509327318403745899 ) ;
#59718 = DIRECTION ( 'NONE',  ( 0.000000000000000000, 1.000000000000000000, 0.000000000000000000 ) ) ;
#59719 = AXIS2_PLACEMENT_3D ( 'NONE', #99114, #43432, #2181 ) ;
#59720 = ORIENTED_EDGE ( 'NONE', *, *, #86683, .T. ) ;
#59721 = CARTESIAN_POINT ( 'NONE',  ( -8.750000000000008882, 2.500000000000000000, -2.957883832488653830 ) ) ;
#59722 = DIRECTION ( 'NONE',  ( 0.000000000000000000, 0.000000000000000000, 1.000000000000000000 ) ) ;
#59723 = DIRECTION ( 'NONE',  ( -4.274815082592931898E-19, -0.9999939076577903929, -0.003490651415223739937 ) ) ;
#59724 = AXIS2_PLACEMENT_3D ( 'NONE', #117908, #28252, #68165 ) ;
#59725 = VERTEX_POINT ( 'NONE', #113815 ) ;
#59726 = CARTESIAN_POINT ( 'NONE',  ( -10.60000000000000142, 2.500000000000000000, 4.676537180435972552 ) ) ;
#59727 = EDGE_CURVE ( 'NONE', #56812, #63511, #91593, .T. ) ;
#59728 = AXIS2_PLACEMENT_3D ( 'NONE', #103140, #43600, #123417 ) ;
#59729 = ORIENTED_EDGE ( 'NONE', *, *, #68527, .T. ) ;
#59730 = DIRECTION ( 'NONE',  ( -4.274815082592931898E-19, -0.9999939076577903929, -0.003490651415223739937 ) ) ;
#59731 = DIRECTION ( 'NONE',  ( 0.000000000000000000, 1.000000000000000000, 0.000000000000000000 ) ) ;
#59732 = CARTESIAN_POINT ( 'NONE',  ( 3.749999999999942268, 2.500000000000000000, -1.372243186433550033 ) ) ;
#59733 = VERTEX_POINT ( 'NONE', #73242 ) ;
#59734 = AXIS2_PLACEMENT_3D ( 'NONE', #108900, #110842, #90563 ) ;
#59735 = CIRCLE ( 'NONE', #53459, 0.06509327318403745899 ) ;
#59736 = DIRECTION ( 'NONE',  ( 0.000000000000000000, 0.000000000000000000, -1.000000000000000000 ) ) ;
#59737 = AXIS2_PLACEMENT_3D ( 'NONE', #117374, #79435, #41451 ) ;
#59738 = CARTESIAN_POINT ( 'NONE',  ( -3.350000000000028511, 2.500000000000000000, -2.857883832488653741 ) ) ;
#59739 = AXIS2_PLACEMENT_3D ( 'NONE', #114547, #55644, #45193 ) ;
#59740 = EDGE_CURVE ( 'NONE', #120245, #66596, #67864, .T. ) ;
#59741 = EDGE_LOOP ( 'NONE', ( #9676, #62025 ) ) ;
#59742 = CARTESIAN_POINT ( 'NONE',  ( -10.60000000000000142, 12.50000000000000000, 4.676537180435972552 ) ) ;
#59743 = EDGE_CURVE ( 'NONE', #58412, #85724, #124306, .T. ) ;
#59744 = EDGE_LOOP ( 'NONE', ( #118239, #81633 ) ) ;
#59745 = FACE_OUTER_BOUND ( 'NONE', #66502, .T. ) ;
#59746 = ORIENTED_EDGE ( 'NONE', *, *, #81631, .T. ) ;
#59747 = DIRECTION ( 'NONE',  ( 0.000000000000000000, 1.000000000000000000, 0.000000000000000000 ) ) ;
#59748 = DIRECTION ( 'NONE',  ( 0.000000000000000000, 0.000000000000000000, 1.000000000000000000 ) ) ;
#59749 = ORIENTED_EDGE ( 'NONE', *, *, #1697, .T. ) ;
#59750 = EDGE_CURVE ( 'NONE', #59274, #17587, #99183, .T. ) ;
#59751 = EDGE_LOOP ( 'NONE', ( #121423, #58746 ) ) ;
#59752 = DIRECTION ( 'NONE',  ( -0.000000000000000000, 1.000000000000000000, -0.000000000000000000 ) ) ;
#59753 = DIRECTION ( 'NONE',  ( -0.000000000000000000, 1.000000000000000000, -0.000000000000000000 ) ) ;
#59754 = CIRCLE ( 'NONE', #17859, 0.06509327318403745899 ) ;
#59755 = ORIENTED_EDGE ( 'NONE', *, *, #26387, .F. ) ;
#59756 = DIRECTION ( 'NONE',  ( -0.000000000000000000, 1.000000000000000000, -0.000000000000000000 ) ) ;
#59757 = CARTESIAN_POINT ( 'NONE',  ( 187.3593750003414016, 0.000000000000000000, 7.564683531250000925 ) ) ;
#59758 = CARTESIAN_POINT ( 'NONE',  ( -2.499999999999996447, 2.500000000000000000, 4.330127018922196314 ) ) ;
#59759 = CARTESIAN_POINT ( 'NONE',  ( 9.349999999999916156, 2.500000000000000000, -2.611473670974877592 ) ) ;
#59760 = CARTESIAN_POINT ( 'NONE',  ( 9.149999999999916866, 2.500000000000000000, -2.957883832488653830 ) ) ;
#59761 = FACE_OUTER_BOUND ( 'NONE', #115968, .T. ) ;
#59762 = CIRCLE ( 'NONE', #13750, 0.1000000000000002554 ) ;
#59763 = FACE_OUTER_BOUND ( 'NONE', #110314, .T. ) ;
#59764 = CIRCLE ( 'NONE', #36774, 0.06509327318403745899 ) ;
#59765 = VECTOR ( 'NONE', #52014, 1000.000000000000000 ) ;
#59766 = ORIENTED_EDGE ( 'NONE', *, *, #125101, .T. ) ;
#59768 = ORIENTED_EDGE ( 'NONE', *, *, #50922, .T. ) ;
#59767 = EDGE_CURVE ( 'NONE', #73054, #60265, #63682, .T. ) ;
#59769 = ORIENTED_EDGE ( 'NONE', *, *, #4004, .F. ) ;
#59770 = ORIENTED_EDGE ( 'NONE', *, *, #17863, .F. ) ;
#59771 = B_SPLINE_CURVE_WITH_KNOTS ( 'NONE', 3,
 ( #32964, #64962, #33595, #44050 ),
 .UNSPECIFIED., .F., .F.,
 ( 4, 4 ),
 ( 0.2000000000000000666, 0.7999999999999999334 ),
 .UNSPECIFIED. ) ;
#59772 = DIRECTION ( 'NONE',  ( 0.000000000000000000, 1.000000000000000000, 0.000000000000000000 ) ) ;
#59773 = CARTESIAN_POINT ( 'NONE',  ( 6.649999999999930189, 12.50000000000000000, 5.737276932171707422 ) ) ;
#59774 = DIRECTION ( 'NONE',  ( -0.000000000000000000, 1.000000000000000000, -0.000000000000000000 ) ) ;
#59775 = ORIENTED_EDGE ( 'NONE', *, *, #60518, .F. ) ;
#59776 = FACE_BOUND ( 'NONE', #64525, .T. ) ;
#59777 = EDGE_LOOP ( 'NONE', ( #53812, #93269 ) ) ;
#59778 = DIRECTION ( 'NONE',  ( 0.000000000000000000, 1.000000000000000000, 0.000000000000000000 ) ) ;
#59779 = CARTESIAN_POINT ( 'NONE',  ( -0.4000000000000396572, 12.50000000000000000, 4.330127018922196314 ) ) ;
#59781 = ADVANCED_FACE ( 'NONE', ( #122355 ), #111882, .T. ) ;
#59780 = CARTESIAN_POINT ( 'NONE',  ( 9.149999999999920419, 2.500000000000000000, -5.802370205355749988 ) ) ;
#59782 = DIRECTION ( 'NONE',  ( -0.000000000000000000, -1.000000000000000000, -0.000000000000000000 ) ) ;
#59784 = VECTOR ( 'NONE', #23698, 1000.000000000000000 ) ;
#59783 = AXIS2_PLACEMENT_3D ( 'NONE', #106137, #5982, #85837 ) ;
#59785 = CARTESIAN_POINT ( 'NONE',  ( -15.59999999999998010, 2.500000000000000000, -0.3464101615137759604 ) ) ;
#59786 = CARTESIAN_POINT ( 'NONE',  ( 1.849999999999950573, 12.50000000000000000, -1.883746621131363597 ) ) ;
#59787 = DIRECTION ( 'NONE',  ( 0.000000000000000000, 0.000000000000000000, 1.000000000000000000 ) ) ;
#59788 = FACE_OUTER_BOUND ( 'NONE', #40836, .T. ) ;
#59789 = EDGE_CURVE ( 'NONE', #80777, #84307, #102063, .T. ) ;
#59790 = EDGE_CURVE ( 'NONE', #52044, #127925, #52313, .T. ) ;
#59791 = DIRECTION ( 'NONE',  ( 0.000000000000000000, 0.000000000000000000, -1.000000000000000000 ) ) ;
#59792 = EDGE_CURVE ( 'NONE', #72896, #75229, #22872, .T. ) ;
#59793 = EDGE_CURVE ( 'NONE', #88292, #48784, #122992, .T. ) ;
#59794 = DIRECTION ( 'NONE',  ( 0.000000000000000000, 1.000000000000000000, 0.000000000000000000 ) ) ;
#59795 = CIRCLE ( 'NONE', #49324, 0.06509327318403745899 ) ;
#59796 = ORIENTED_EDGE ( 'NONE', *, *, #12716, .T. ) ;
#59797 = VERTEX_POINT ( 'NONE', #83714 ) ;
#59798 = CIRCLE ( 'NONE', #80708, 0.1000000000000002554 ) ;
#59799 = EDGE_LOOP ( 'NONE', ( #62337, #71892 ) ) ;
#59800 = ORIENTED_EDGE ( 'NONE', *, *, #80513, .F. ) ;
#59801 = PLANE ( 'NONE',  #106407 ) ;
#59802 = EDGE_CURVE ( 'NONE', #69160, #62906, #42773, .T. ) ;
#59803 = DIRECTION ( 'NONE',  ( 0.000000000000000000, 0.000000000000000000, 1.000000000000000000 ) ) ;
#59806 = EDGE_LOOP ( 'NONE', ( #118303, #6368 ) ) ;
#59805 = ORIENTED_EDGE ( 'NONE', *, *, #71190, .T. ) ;
#59804 = EDGE_CURVE ( 'NONE', #97882, #22999, #86260, .T. ) ;
#59807 = ORIENTED_EDGE ( 'NONE', *, *, #10283, .F. ) ;
#59808 = CARTESIAN_POINT ( 'NONE',  ( 10.84999999999990905, 2.500000000000000000, -7.288010851410854585 ) ) ;
#59809 = ADVANCED_FACE ( 'NONE', ( #57476 ), #74532, .T. ) ;
#59810 = ADVANCED_FACE ( 'NONE', ( #36559 ), #35266, .T. ) ;
#59811 = FACE_OUTER_BOUND ( 'NONE', #15827, .T. ) ;
#59812 = DIRECTION ( 'NONE',  ( -4.274815082592931898E-19, -0.9999939076577903929, -0.003490651415223739937 ) ) ;
#59813 = DIRECTION ( 'NONE',  ( 0.000000000000000000, 1.000000000000000000, 0.000000000000000000 ) ) ;
#59814 = CARTESIAN_POINT ( 'NONE',  ( 6.649999999999930189, 2.500000000000000000, 7.288010851410849256 ) ) ;
#59815 = CARTESIAN_POINT ( 'NONE',  ( 2.500000000000002220, 1.761799387799150018, 10.00000000000000000 ) ) ;
#59816 = CARTESIAN_POINT ( 'NONE',  ( 7.099999999999928590, 2.500000000000000000, 3.637306695894644726 ) ) ;
#59817 = ADVANCED_FACE ( 'NONE', ( #76471 ), #16227, .T. ) ;
#59818 = ORIENTED_EDGE ( 'NONE', *, *, #43814, .T. ) ;
#59819 = ADVANCED_FACE ( 'NONE', ( #5134 ), #27338, .T. ) ;
#59820 = DIRECTION ( 'NONE',  ( 0.000000000000000000, 1.000000000000000000, 0.000000000000000000 ) ) ;
#59821 = ORIENTED_EDGE ( 'NONE', *, *, #25748, .T. ) ;
#59823 = EDGE_LOOP ( 'NONE', ( #61000, #45183 ) ) ;
#59822 = AXIS2_PLACEMENT_3D ( 'NONE', #119972, #30323, #100337 ) ;
#59824 = ORIENTED_EDGE ( 'NONE', *, *, #46181, .F. ) ;
#59825 = AXIS2_PLACEMENT_3D ( 'NONE', #19756, #117934, #89128 ) ;
#59826 = DIRECTION ( 'NONE',  ( -0.000000000000000000, -1.000000000000000000, -0.000000000000000000 ) ) ;
#59827 = ORIENTED_EDGE ( 'NONE', *, *, #27522, .T. ) ;
#59828 = EDGE_LOOP ( 'NONE', ( #25771, #52344, #4446, #110769 ) ) ;
#59829 = DIRECTION ( 'NONE',  ( 0.000000000000000000, 0.000000000000000000, -1.000000000000000000 ) ) ;
#59830 = AXIS2_PLACEMENT_3D ( 'NONE', #66631, #98666, #7059 ) ;
#59831 = FACE_OUTER_BOUND ( 'NONE', #109723, .T. ) ;
#59832 = CARTESIAN_POINT ( 'NONE',  ( -15.39999999999997904, 2.500000000000000000, 0.000000000000000000 ) ) ;
#59833 = DIRECTION ( 'NONE',  ( -0.000000000000000000, -1.000000000000000000, -0.000000000000000000 ) ) ;
#59834 = PLANE ( 'NONE',  #56656 ) ;
#59835 = VERTEX_POINT ( 'NONE', #75174 ) ;
#59836 = DIRECTION ( 'NONE',  ( 0.000000000000000000, 0.000000000000000000, -1.000000000000000000 ) ) ;
#59837 = CIRCLE ( 'NONE', #45232, 0.1000000000000002554 ) ;
#59838 = EDGE_LOOP ( 'NONE', ( #61003, #61481 ) ) ;
#59839 = CARTESIAN_POINT ( 'NONE',  ( 18.45986577996939104, -0.7763546025154367536, 4.045836809868020190 ) ) ;
#59840 = AXIS2_PLACEMENT_3D ( 'NONE', #95690, #8564, #48517 ) ;
#59841 = ORIENTED_EDGE ( 'NONE', *, *, #51437, .F. ) ;
#59842 = FACE_OUTER_BOUND ( 'NONE', #117670, .T. ) ;
#59843 = PLANE ( 'NONE',  #1017 ) ;
#59844 = VERTEX_POINT ( 'NONE', #45084 ) ;
#59845 = DIRECTION ( 'NONE',  ( -0.000000000000000000, 1.000000000000000000, -0.000000000000000000 ) ) ;
#59846 = FACE_OUTER_BOUND ( 'NONE', #76640, .T. ) ;
#59847 = EDGE_LOOP ( 'NONE', ( #70788, #48279, #53420, #56858 ) ) ;
#59848 = ADVANCED_FACE ( 'NONE', ( #84982 ), #11434, .T. ) ;
#59849 = DIRECTION ( 'NONE',  ( 0.000000000000000000, 0.000000000000000000, 1.000000000000000000 ) ) ;
#59850 = EDGE_CURVE ( 'NONE', #64883, #112256, #17685, .T. ) ;
#59851 = ORIENTED_EDGE ( 'NONE', *, *, #69047, .F. ) ;
#59852 = VERTEX_POINT ( 'NONE', #96097 ) ;
#59853 = DIRECTION ( 'NONE',  ( 0.000000000000000000, -0.000000000000000000, 1.000000000000000000 ) ) ;
#59854 = CARTESIAN_POINT ( 'NONE',  ( 8.949999999999921130, 12.50000000000000000, 1.883746621131358934 ) ) ;
#59855 = DIRECTION ( 'NONE',  ( -4.274815082592931898E-19, -0.9999939076577903929, -0.003490651415223739937 ) ) ;
#59856 = AXIS2_PLACEMENT_3D ( 'NONE', #84382, #44457, #56200 ) ;
#59857 = CARTESIAN_POINT ( 'NONE',  ( -5.600000000000023626, 2.500000000000000000, -4.576537180435977348 ) ) ;
#59858 = DIRECTION ( 'NONE',  ( 0.000000000000000000, 0.000000000000000000, 1.000000000000000000 ) ) ;
#59859 = EDGE_LOOP ( 'NONE', ( #105182, #113775, #94385, #85373 ) ) ;
#59860 = AXIS2_PLACEMENT_3D ( 'NONE', #44511, #37916, #117100 ) ;
#59861 = FACE_OUTER_BOUND ( 'NONE', #70929, .T. ) ;
#59862 = AXIS2_PLACEMENT_3D ( 'NONE', #91473, #100637, #81651 ) ;
#59863 = CIRCLE ( 'NONE', #51525, 0.09999999999999999167 ) ;
#59864 = ORIENTED_EDGE ( 'NONE', *, *, #53265, .T. ) ;
#59865 = AXIS2_PLACEMENT_3D ( 'NONE', #91769, #23035, #121229 ) ;
#59866 = DIRECTION ( 'NONE',  ( 0.000000000000000000, 0.000000000000000000, 1.000000000000000000 ) ) ;
#59867 = DIRECTION ( 'NONE',  ( 0.000000000000000000, -0.9999939076577903929, 0.003490651415223739937 ) ) ;
#59868 = CIRCLE ( 'NONE', #109927, 0.06509327318403745899 ) ;
#59869 = CARTESIAN_POINT ( 'NONE',  ( 187.2968750003414300, 8.734944146203032389, 5.348610694689227483E-16 ) ) ;
#59870 = CARTESIAN_POINT ( 'NONE',  ( 9.349999999999919709, 2.500000000000000000, -6.741600689897078169 ) ) ;
#59871 = FACE_OUTER_BOUND ( 'NONE', #121344, .T. ) ;
#59872 = FACE_OUTER_BOUND ( 'NONE', #114198, .T. ) ;
#59873 = FACE_OUTER_BOUND ( 'NONE', #84713, .T. ) ;
#59874 = ORIENTED_EDGE ( 'NONE', *, *, #27834, .F. ) ;
#59875 = CIRCLE ( 'NONE', #5445, 0.06509327318403745899 ) ;
#59876 = DIRECTION ( 'NONE',  ( 0.000000000000000000, 0.000000000000000000, -1.000000000000000000 ) ) ;
#59878 = CIRCLE ( 'NONE', #76577, 0.1000000000000002554 ) ;
#59877 = CONICAL_SURFACE ( 'NONE', #105816, 0.1000000000000002554, 0.003490658503988666988 ) ;
#59879 = DIRECTION ( 'NONE',  ( 0.000000000000000000, 0.000000000000000000, 1.000000000000000000 ) ) ;
#59880 = DIRECTION ( 'NONE',  ( -0.000000000000000000, 1.000000000000000000, -0.000000000000000000 ) ) ;
#59881 = ORIENTED_EDGE ( 'NONE', *, *, #105700, .F. ) ;
#59882 = DIRECTION ( 'NONE',  ( 0.000000000000000000, 0.000000000000000000, -1.000000000000000000 ) ) ;
#59883 = ADVANCED_FACE ( 'NONE', ( #16858 ), #61628, .T. ) ;
#59884 = VERTEX_POINT ( 'NONE', #25407 ) ;
#59885 = ORIENTED_EDGE ( 'NONE', *, *, #129392, .F. ) ;
#59886 = CARTESIAN_POINT ( 'NONE',  ( 3.549999999999942091, 12.50000000000000000, 2.576566944158910744 ) ) ;
#59887 = ORIENTED_EDGE ( 'NONE', *, *, #6803, .T. ) ;
#59888 = DIRECTION ( 'NONE',  ( 0.000000000000000000, 1.000000000000000000, 0.000000000000000000 ) ) ;
#59889 = CARTESIAN_POINT ( 'NONE',  ( 8.149999999999923972, 2.500000000000000000, -6.941600689897077459 ) ) ;
#59890 = ORIENTED_EDGE ( 'NONE', *, *, #9857, .F. ) ;
#59891 = PLANE ( 'NONE',  #88535 ) ;
#59892 = CARTESIAN_POINT ( 'NONE',  ( 3.749999999999938716, 2.500000000000000000, 7.188010851410848723 ) ) ;
#59893 = EDGE_CURVE ( 'NONE', #137, #115201, #118042, .T. ) ;
#59894 = DIRECTION ( 'NONE',  ( 0.000000000000000000, 1.000000000000000000, 0.000000000000000000 ) ) ;
#59895 = EDGE_CURVE ( 'NONE', #124839, #24998, #55353, .T. ) ;
#59896 = EDGE_LOOP ( 'NONE', ( #110813, #102259 ) ) ;
#59897 = VECTOR ( 'NONE', #24197, 1000.000000000000000 ) ;
#59898 = EDGE_LOOP ( 'NONE', ( #38917, #83992, #19454, #100031 ) ) ;
#59899 = AXIS2_PLACEMENT_3D ( 'NONE', #119083, #128272, #118427 ) ;
#59900 = ORIENTED_EDGE ( 'NONE', *, *, #125665, .F. ) ;
#59901 = DIRECTION ( 'NONE',  ( 0.000000000000000000, 0.000000000000000000, 1.000000000000000000 ) ) ;
#59902 = DIRECTION ( 'NONE',  ( 0.000000000000000000, -0.9999939076577903929, 0.003490651415223739937 ) ) ;
#59903 = CARTESIAN_POINT ( 'NONE',  ( -8.750000000000008882, 2.500000000000000000, 1.572243186433545548 ) ) ;
#59904 = EDGE_CURVE ( 'NONE', #72819, #85157, #64701, .T. ) ;
#59905 = FACE_BOUND ( 'NONE', #73461, .T. ) ;
#59906 = ORIENTED_EDGE ( 'NONE', *, *, #70420, .T. ) ;
#59907 = DIRECTION ( 'NONE',  ( -0.000000000000000000, 1.000000000000000000, -0.000000000000000000 ) ) ;
#59908 = CARTESIAN_POINT ( 'NONE',  ( -3.749999999999991118, 12.50000000000000000, -2.165063509461101710 ) ) ;
#59909 = EDGE_LOOP ( 'NONE', ( #128421, #11689, #35598, #120128 ) ) ;
#59911 = CIRCLE ( 'NONE', #80738, 0.09999999999999999167 ) ;
#59910 = AXIS2_PLACEMENT_3D ( 'NONE', #100261, #89141, #21042 ) ;
#59912 = DIRECTION ( 'NONE',  ( 0.000000000000000000, 0.000000000000000000, 1.000000000000000000 ) ) ;
#59913 = DIRECTION ( 'NONE',  ( 0.000000000000000000, -0.000000000000000000, 1.000000000000000000 ) ) ;
#59914 = DIRECTION ( 'NONE',  ( -0.000000000000000000, -1.000000000000000000, -0.000000000000000000 ) ) ;
#59915 = PLANE ( 'NONE',  #36143 ) ;
#59916 = CARTESIAN_POINT ( 'NONE',  ( -2.499999999999996003, 12.50000000000000000, -2.276824562219559311E-15 ) ) ;
#59917 = CARTESIAN_POINT ( 'NONE',  ( 11.24999999999990585, 12.50000000000000000, 2.857883832488649301 ) ) ;
#59918 = CARTESIAN_POINT ( 'NONE',  ( 11.84999999999990372, 2.500000000000000000, -6.048780366869526581 ) ) ;
#59920 = VECTOR ( 'NONE', #91747, 1000.000000000000000 ) ;
#59919 = AXIS2_PLACEMENT_3D ( 'NONE', #91706, #53070, #43269 ) ;
#59921 = AXIS2_PLACEMENT_3D ( 'NONE', #111274, #61575, #101489 ) ;
#59922 = ORIENTED_EDGE ( 'NONE', *, *, #72617, .T. ) ;
#59923 = ORIENTED_EDGE ( 'NONE', *, *, #91159, .F. ) ;
#59924 = ORIENTED_EDGE ( 'NONE', *, *, #7565, .T. ) ;
#59925 = ORIENTED_EDGE ( 'NONE', *, *, #87927, .F. ) ;
#59926 = ORIENTED_EDGE ( 'NONE', *, *, #128472, .F. ) ;
#59927 = CARTESIAN_POINT ( 'NONE',  ( 13.54999999999990123, 2.500000000000000000, 1.818653347947321475 ) ) ;
#59928 = LINE ( 'NONE', #88039, #124055 ) ;
#59929 = EDGE_LOOP ( 'NONE', ( #50880, #29393 ) ) ;
#59930 = FACE_BOUND ( 'NONE', #74795, .T. ) ;
#59931 = DIRECTION ( 'NONE',  ( 0.000000000000000000, 0.000000000000000000, 1.000000000000000000 ) ) ;
#59932 = EDGE_CURVE ( 'NONE', #111598, #3394, #63768, .T. ) ;
#59933 = CARTESIAN_POINT ( 'NONE',  ( -1.700000000000034817, 2.500000000000000000, -4.430127018922202176 ) ) ;
#59934 = CARTESIAN_POINT ( 'NONE',  ( -10.85000000000000142, 12.50000000000000000, -6.495190528383298911 ) ) ;
#59935 = CARTESIAN_POINT ( 'NONE',  ( 184.5000000000000000, -0.3110874738271938167, 7.694949878671636156 ) ) ;
#59936 = DIRECTION ( 'NONE',  ( -0.000000000000000000, -1.000000000000000000, -0.000000000000000000 ) ) ;
#59937 = EDGE_CURVE ( 'NONE', #81531, #59613, #65335, .T. ) ;
#59938 = DIRECTION ( 'NONE',  ( 0.000000000000000000, 0.000000000000000000, -1.000000000000000000 ) ) ;
#59940 = VERTEX_POINT ( 'NONE', #125551 ) ;
#59939 = AXIS2_PLACEMENT_3D ( 'NONE', #5163, #45114, #85019 ) ;
#59941 = EDGE_CURVE ( 'NONE', #45135, #77998, #82558, .T. ) ;
#59942 = AXIS2_PLACEMENT_3D ( 'NONE', #118028, #68928, #8072 ) ;
#59943 = EDGE_LOOP ( 'NONE', ( #54795, #114518 ) ) ;
#59944 = EDGE_LOOP ( 'NONE', ( #127699, #46821 ) ) ;
#59946 = VERTEX_POINT ( 'NONE', #15594 ) ;
#59945 = VECTOR ( 'NONE', #37011, 1000.000000000000000 ) ;
#59947 = ORIENTED_EDGE ( 'NONE', *, *, #64339, .T. ) ;
#59948 = VERTEX_POINT ( 'NONE', #75803 ) ;
#59949 = EDGE_CURVE ( 'NONE', #123441, #100484, #22016, .T. ) ;
#59951 = ADVANCED_FACE ( 'NONE', ( #47017 ), #3133, .T. ) ;
#59950 = DIRECTION ( 'NONE',  ( 1.000000000000000000, 0.000000000000000000, 0.000000000000000000 ) ) ;
#59952 = CARTESIAN_POINT ( 'NONE',  ( 6.249999999999967137, 12.50000000000000000, 6.560283801567334372 ) ) ;
#59954 = VERTEX_POINT ( 'NONE', #58124 ) ;
#59953 = EDGE_CURVE ( 'NONE', #114987, #40225, #40425, .T. ) ;
#59955 = CARTESIAN_POINT ( 'NONE',  ( 4.599999999999939249, 12.50000000000000000, -3.637306695894650055 ) ) ;
#59956 = VECTOR ( 'NONE', #15105, 1000.000000000000000 ) ;
#59957 = AXIS2_PLACEMENT_3D ( 'NONE', #29327, #40447, #50897 ) ;
#59958 = DIRECTION ( 'NONE',  ( 0.000000000000000000, 0.000000000000000000, 1.000000000000000000 ) ) ;
#59959 = CIRCLE ( 'NONE', #3493, 0.1000000000000002554 ) ;
#59961 = ADVANCED_FACE ( 'NONE', ( #117644 ), #115988, .T. ) ;
#59960 = PLANE ( 'NONE',  #78807 ) ;
#59962 = CARTESIAN_POINT ( 'NONE',  ( 185.6510416670080303, 4.367472073101518859, -7.564683531249999149 ) ) ;
#59963 = DIRECTION ( 'NONE',  ( 0.000000000000000000, 0.000000000000000000, -1.000000000000000000 ) ) ;
#59964 = CARTESIAN_POINT ( 'NONE',  ( -5.650000000000023448, 12.50000000000000000, -2.446380397790840266 ) ) ;
#59965 = DIRECTION ( 'NONE',  ( -0.000000000000000000, 1.000000000000000000, -0.000000000000000000 ) ) ;
#59966 = CONICAL_SURFACE ( 'NONE', #51628, 0.1000000000000002554, 0.003490658503988666988 ) ;
#59967 = EDGE_LOOP ( 'NONE', ( #59775, #69911, #55485, #93746 ) ) ;
#59968 = FACE_OUTER_BOUND ( 'NONE', #103787, .T. ) ;
#59969 = EDGE_CURVE ( 'NONE', #32170, #70149, #7311, .T. ) ;
#59970 = AXIS2_PLACEMENT_3D ( 'NONE', #126532, #28981, #38148 ) ;
#59971 = VERTEX_POINT ( 'NONE', #128145 ) ;
#59973 = AXIS2_PLACEMENT_3D ( 'NONE', #25446, #94858, #16898 ) ;
#59972 = CIRCLE ( 'NONE', #124782, 0.1000000000000002554 ) ;
#59974 = ORIENTED_EDGE ( 'NONE', *, *, #92511, .F. ) ;
#59975 = DIRECTION ( 'NONE',  ( 0.000000000000000000, 0.000000000000000000, -1.000000000000000000 ) ) ;
#59976 = DIRECTION ( 'NONE',  ( -0.000000000000000000, -1.000000000000000000, -0.000000000000000000 ) ) ;
#59977 = FACE_OUTER_BOUND ( 'NONE', #126977, .T. ) ;
#59978 = EDGE_LOOP ( 'NONE', ( #37238, #58022, #103460, #89964 ) ) ;
#59979 = EDGE_LOOP ( 'NONE', ( #125862, #106286, #84666, #124976 ) ) ;
#59980 = DIRECTION ( 'NONE',  ( 0.000000000000000000, 1.000000000000000000, 0.000000000000000000 ) ) ;
#59981 = DIRECTION ( 'NONE',  ( -0.000000000000000000, 1.000000000000000000, -0.000000000000000000 ) ) ;
#59982 = FACE_OUTER_BOUND ( 'NONE', #113549, .T. ) ;
#59983 = DIRECTION ( 'NONE',  ( 0.000000000000000000, 0.000000000000000000, 1.000000000000000000 ) ) ;
#59984 = ORIENTED_EDGE ( 'NONE', *, *, #21441, .F. ) ;
#59985 = DIRECTION ( 'NONE',  ( -0.000000000000000000, 1.000000000000000000, -0.000000000000000000 ) ) ;
#59986 = CIRCLE ( 'NONE', #114412, 0.1000000000000000056 ) ;
#59987 = ORIENTED_EDGE ( 'NONE', *, *, #107531, .F. ) ;
#59988 = LINE ( 'NONE', #38407, #68738 ) ;
#59989 = VERTEX_POINT ( 'NONE', #28664 ) ;
#59990 = DIRECTION ( 'NONE',  ( 0.000000000000000000, 0.000000000000000000, -1.000000000000000000 ) ) ;
#59991 = DIRECTION ( 'NONE',  ( -0.000000000000000000, 1.000000000000000000, -0.000000000000000000 ) ) ;
#59992 = CARTESIAN_POINT ( 'NONE',  ( 10.44999999999991047, 12.50000000000000000, 2.230156782645134950 ) ) ;
#59993 = DIRECTION ( 'NONE',  ( -0.000000000000000000, 1.000000000000000000, -0.000000000000000000 ) ) ;
#59994 = ORIENTED_EDGE ( 'NONE', *, *, #17941, .T. ) ;
#59995 = DIRECTION ( 'NONE',  ( 0.000000000000000000, 0.000000000000000000, 1.000000000000000000 ) ) ;
#59996 = VECTOR ( 'NONE', #43209, 1000.000000000000000 ) ;
#59997 = EDGE_CURVE ( 'NONE', #105793, #15915, #120265, .T. ) ;
#59998 = ORIENTED_EDGE ( 'NONE', *, *, #114763, .T. ) ;
#59999 = ORIENTED_EDGE ( 'NONE', *, *, #57819, .T. ) ;
#60000 = CARTESIAN_POINT ( 'NONE',  ( -1.650000000000034328, 2.500000000000000000, -2.957883832488653830 ) ) ;
#60001 = CARTESIAN_POINT ( 'NONE',  ( 5.799999999999933209, 2.500000000000000000, -2.385244779468109755E-15 ) ) ;
#60002 = PLANE ( 'NONE',  #32389 ) ;
#60003 = FILL_AREA_STYLE ('',( #12150 ) ) ;
#60004 = FACE_OUTER_BOUND ( 'NONE', #11020, .T. ) ;
#60007 = CONICAL_SURFACE ( 'NONE', #32808, 0.09999999999999982514, 0.003490658503988666988 ) ;
#60006 = DIRECTION ( 'NONE',  ( 0.000000000000000000, 0.000000000000000000, 1.000000000000000000 ) ) ;
#60005 = CONICAL_SURFACE ( 'NONE', #95479, 0.1000000000000000472, 0.003490658503988666988 ) ;
#60008 = ADVANCED_FACE ( 'NONE', ( #39782 ), #109738, .T. ) ;
#60009 = DIRECTION ( 'NONE',  ( -0.000000000000000000, 1.000000000000000000, -0.000000000000000000 ) ) ;
#60010 = CARTESIAN_POINT ( 'NONE',  ( -10.85000000000000142, 2.500000000000000000, 2.265063509461097357 ) ) ;
#60011 = CARTESIAN_POINT ( 'NONE',  ( 6.449999999999928235, 2.500000000000000000, 2.611473670974873151 ) ) ;
#60013 = CIRCLE ( 'NONE', #108004, 0.09999999999999982514 ) ;
#60012 = CIRCLE ( 'NONE', #101844, 0.1000000000000002554 ) ;
#60014 = AXIS2_PLACEMENT_3D ( 'NONE', #59927, #6901, #46867 ) ;
#60015 = EDGE_LOOP ( 'NONE', ( #57887, #40758 ) ) ;
#60016 = CARTESIAN_POINT ( 'NONE',  ( 13.54999999999989591, 12.50000000000000000, -1.883746621131363597 ) ) ;
#60017 = DIRECTION ( 'NONE',  ( -0.000000000000000000, 1.000000000000000000, -0.000000000000000000 ) ) ;
#60018 = DIRECTION ( 'NONE',  ( 0.000000000000000000, 0.000000000000000000, 1.000000000000000000 ) ) ;
#60019 = CARTESIAN_POINT ( 'NONE',  ( -3.100000000000028511, 2.500000000000000000, -4.576537180435977348 ) ) ;
#60020 = FACE_OUTER_BOUND ( 'NONE', #98826, .T. ) ;
#60021 = VERTEX_POINT ( 'NONE', #98031 ) ;
#60022 = DIRECTION ( 'NONE',  ( 0.000000000000000000, -0.9999939076577903929, 0.003490651415223739937 ) ) ;
#60023 = CARTESIAN_POINT ( 'NONE',  ( -7.700000000000012612, 2.500000000000000000, 4.676537180435972552 ) ) ;
#60025 = EDGE_LOOP ( 'NONE', ( #106561, #97370, #115746, #129580 ) ) ;
#60024 = DIRECTION ( 'NONE',  ( 0.000000000000000000, -0.9999939076577903929, 0.003490651415223739937 ) ) ;
#60026 = VECTOR ( 'NONE', #100175, 1000.000000000000000 ) ;
#60027 = VERTEX_POINT ( 'NONE', #129462 ) ;
#60028 = CARTESIAN_POINT ( 'NONE',  ( 6.849999999999927702, 2.500000000000000000, 1.918653347947321564 ) ) ;
#60029 = EDGE_CURVE ( 'NONE', #56111, #53781, #113940, .T. ) ;
#60030 = CIRCLE ( 'NONE', #30784, 0.1000000000000000056 ) ;
#60031 = ORIENTED_EDGE ( 'NONE', *, *, #129287, .F. ) ;
#60032 = ORIENTED_EDGE ( 'NONE', *, *, #86361, .T. ) ;
#60033 = CARTESIAN_POINT ( 'NONE',  ( 7.899999999999924860, 12.50000000000000000, 3.637306695894644726 ) ) ;
#60034 = AXIS2_PLACEMENT_3D ( 'NONE', #124131, #52816, #23339 ) ;
#60035 = DIRECTION ( 'NONE',  ( 0.000000000000000000, 1.000000000000000000, 0.000000000000000000 ) ) ;
#60036 = CARTESIAN_POINT ( 'NONE',  ( 13.14999999999989733, 2.500000000000000000, -2.611473670974877592 ) ) ;
#60037 = VECTOR ( 'NONE', #102554, 1000.000000000000000 ) ;
#60038 = DIRECTION ( 'NONE',  ( 0.000000000000000000, 0.000000000000000000, 1.000000000000000000 ) ) ;
#60039 = EDGE_CURVE ( 'NONE', #35443, #114904, #67952, .T. ) ;
#60040 = VERTEX_POINT ( 'NONE', #454 ) ;
#60041 = CARTESIAN_POINT ( 'NONE',  ( 13.74999999999993427, 12.50000000000000000, 2.165063509461097713 ) ) ;
#60042 = EDGE_LOOP ( 'NONE', ( #101274, #88325 ) ) ;
#60043 = CARTESIAN_POINT ( 'NONE',  ( 8.749999999999957367, 12.50000000000000000, -6.495190528383302464 ) ) ;
#60044 = EDGE_CURVE ( 'NONE', #27533, #29548, #49601, .T. ) ;
#60045 = CARTESIAN_POINT ( 'NONE',  ( -5.800000000000022027, 12.50000000000000000, -4.330127018922201643 ) ) ;
#60046 = AXIS2_PLACEMENT_3D ( 'NONE', #98088, #59492, #8406 ) ;
#60047 = DIRECTION ( 'NONE',  ( 0.000000000000000000, 0.000000000000000000, -1.000000000000000000 ) ) ;
#60048 = EDGE_CURVE ( 'NONE', #117860, #109761, #42863, .T. ) ;
#60049 = CONICAL_SURFACE ( 'NONE', #62099, 0.1000000000000002554, 0.003490658503988666988 ) ;
#60050 = EDGE_LOOP ( 'NONE', ( #128366, #94479, #11825, #53223 ) ) ;
#60051 = ORIENTED_EDGE ( 'NONE', *, *, #57397, .F. ) ;
#60053 = ORIENTED_EDGE ( 'NONE', *, *, #118244, .T. ) ;
#60052 = EDGE_CURVE ( 'NONE', #128668, #53584, #57504, .T. ) ;
#60054 = ORIENTED_EDGE ( 'NONE', *, *, #122595, .F. ) ;
#60055 = ORIENTED_EDGE ( 'NONE', *, *, #76454, .T. ) ;
#60056 = DIRECTION ( 'NONE',  ( -0.000000000000000000, 1.000000000000000000, -0.000000000000000000 ) ) ;
#60057 = CARTESIAN_POINT ( 'NONE',  ( 15.62882261213669999, 2.499999999999999556, 5.624357572923773141 ) ) ;
#60058 = DIRECTION ( 'NONE',  ( 0.000000000000000000, 0.000000000000000000, -1.000000000000000000 ) ) ;
#60059 = EDGE_CURVE ( 'NONE', #104314, #19521, #30337, .T. ) ;
#60060 = FACE_BOUND ( 'NONE', #1329, .T. ) ;
#60061 = CARTESIAN_POINT ( 'NONE',  ( 11.64999999999990443, 2.500000000000000000, 1.372243186433545370 ) ) ;
#60062 = CARTESIAN_POINT ( 'NONE',  ( 186.4479166673494603, -6.668395609140176816, -3.850000000000003642 ) ) ;
#60063 = CARTESIAN_POINT ( 'NONE',  ( 10.84999999999991260, 2.500000000000000000, -2.265063509461101798 ) ) ;
#60064 = LINE ( 'NONE', #99971, #96070 ) ;
#60065 = CARTESIAN_POINT ( 'NONE',  ( -5.000000000000022204, 12.50000000000000000, 3.637306695894644726 ) ) ;
#60066 = DIRECTION ( 'NONE',  ( -0.000000000000000000, -1.000000000000000000, -0.000000000000000000 ) ) ;
#60067 = CIRCLE ( 'NONE', #62213, 0.06509327318403743123 ) ;
#60068 = DIRECTION ( 'NONE',  ( -0.000000000000000000, 1.000000000000000000, -0.000000000000000000 ) ) ;
#60069 = DIRECTION ( 'NONE',  ( 0.000000000000000000, -0.9999939076577903929, 0.003490651415223739937 ) ) ;
#60070 = EDGE_LOOP ( 'NONE', ( #75283, #118676 ) ) ;
#60071 = EDGE_LOOP ( 'NONE', ( #26465, #102924, #92245, #33980 ) ) ;
#60072 = EDGE_LOOP ( 'NONE', ( #10177, #32505, #52450, #10306 ) ) ;
#60073 = ORIENTED_EDGE ( 'NONE', *, *, #76093, .F. ) ;
#60074 = CARTESIAN_POINT ( 'NONE',  ( -5.650000000000023448, 2.500000000000000000, -6.841600689897078702 ) ) ;
#60075 = DIRECTION ( 'NONE',  ( -4.274815082592931898E-19, -0.9999939076577903929, -0.003490651415223739937 ) ) ;
#60076 = FACE_BOUND ( 'NONE', #79707, .T. ) ;
#60077 = DIRECTION ( 'NONE',  ( -0.000000000000000000, -1.000000000000000000, -0.000000000000000000 ) ) ;
#60078 = AXIS2_PLACEMENT_3D ( 'NONE', #120943, #101319, #31933 ) ;
#60079 = CONICAL_SURFACE ( 'NONE', #32983, 0.1000000000000000472, 0.003490658503988666988 ) ;
#60080 = EDGE_LOOP ( 'NONE', ( #4194, #32685, #70701, #88727 ) ) ;
#60081 = DIRECTION ( 'NONE',  ( 0.000000000000000000, 0.000000000000000000, 1.000000000000000000 ) ) ;
#60082 = CARTESIAN_POINT ( 'NONE',  ( 105.5000000000000142, -1.500000000000000222, -1.322875655532295136 ) ) ;
#60083 = CARTESIAN_POINT ( 'NONE',  ( 12.29999999999990301, 2.500000000000000000, -0.2464101615137782308 ) ) ;
#60084 = CARTESIAN_POINT ( 'NONE',  ( 8.349999999999923261, 2.500000000000000000, -7.188010851410854052 ) ) ;
#60085 = ORIENTED_EDGE ( 'NONE', *, *, #80658, .F. ) ;
#60086 = DIRECTION ( 'NONE',  ( 0.000000000000000000, 0.000000000000000000, -1.000000000000000000 ) ) ;
#60088 = EDGE_CURVE ( 'NONE', #7453, #61323, #1059, .T. ) ;
#60087 = AXIS2_PLACEMENT_3D ( 'NONE', #48402, #18924, #79171 ) ;
#60089 = VECTOR ( 'NONE', #64284, 1000.000000000000000 ) ;
#60090 = ORIENTED_EDGE ( 'NONE', *, *, #50891, .F. ) ;
#60091 = VERTEX_POINT ( 'NONE', #18177 ) ;
#60092 = EDGE_CURVE ( 'NONE', #98931, #36138, #90125, .T. ) ;
#60093 = DIRECTION ( 'NONE',  ( 0.000000000000000000, 0.000000000000000000, -1.000000000000000000 ) ) ;
#60094 = DIRECTION ( 'NONE',  ( 0.000000000000000000, -0.000000000000000000, 1.000000000000000000 ) ) ;
#60096 = VERTEX_POINT ( 'NONE', #108492 ) ;
#60095 = ADVANCED_FACE ( 'NONE', ( #19466 ), #15620, .T. ) ;
#60099 = EDGE_CURVE ( 'NONE', #122658, #98888, #17779, .T. ) ;
#60098 = AXIS2_PLACEMENT_3D ( 'NONE', #75178, #35269, #124285 ) ;
#60097 = VECTOR ( 'NONE', #15377, 1000.000000000000000 ) ;
#60100 = VECTOR ( 'NONE', #94345, 1000.000000000000000 ) ;
#60101 = CARTESIAN_POINT ( 'NONE',  ( -7.500000000000016875, 12.50000000000000000, -3.637306695894650055 ) ) ;
#60102 = DIRECTION ( 'NONE',  ( 0.000000000000000000, -0.000000000000000000, 1.000000000000000000 ) ) ;
#60104 = EDGE_CURVE ( 'NONE', #53570, #1964, #98663, .T. ) ;
#60103 = FACE_OUTER_BOUND ( 'NONE', #30484, .T. ) ;
#60105 = ORIENTED_EDGE ( 'NONE', *, *, #115605, .F. ) ;
#60106 = FACE_OUTER_BOUND ( 'NONE', #274, .T. ) ;
#60107 = ORIENTED_EDGE ( 'NONE', *, *, #23526, .F. ) ;
#60108 = CARTESIAN_POINT ( 'NONE',  ( 12.04999999999990479, 2.500000000000000000, -6.395190528383301931 ) ) ;
#60109 = EDGE_CURVE ( 'NONE', #36539, #72573, #13573, .T. ) ;
#60110 = ADVANCED_FACE ( 'NONE', ( #72448 ), #111798, .T. ) ;
#60111 = ORIENTED_EDGE ( 'NONE', *, *, #27070, .F. ) ;
#60112 = CARTESIAN_POINT ( 'NONE',  ( 112.9920263949885566, 7.694814134679670126, 0.3288087409775817815 ) ) ;
#60113 = VERTEX_POINT ( 'NONE', #52161 ) ;
#60114 = DIRECTION ( 'NONE',  ( 0.000000000000000000, 0.000000000000000000, 1.000000000000000000 ) ) ;
#60115 = AXIS2_PLACEMENT_3D ( 'NONE', #32584, #81649, #22757 ) ;
#60116 = PLANE ( 'NONE',  #121946 ) ;
#60117 = PLANE ( 'NONE',  #119852 ) ;
#60118 = CARTESIAN_POINT ( 'NONE',  ( -4.999999999999990230, 2.500000000000000000, -4.230127018922201998 ) ) ;
#60120 = AXIS2_PLACEMENT_3D ( 'NONE', #29357, #39826, #119641 ) ;
#60119 = DIRECTION ( 'NONE',  ( -0.000000000000000000, -1.000000000000000000, -0.000000000000000000 ) ) ;
#60121 = ORIENTED_EDGE ( 'NONE', *, *, #48469, .T. ) ;
#60122 = CIRCLE ( 'NONE', #22471, 0.06509327318403745899 ) ;
#60123 = ORIENTED_EDGE ( 'NONE', *, *, #26019, .T. ) ;
#60124 = ORIENTED_EDGE ( 'NONE', *, *, #28186, .F. ) ;
#60125 = CARTESIAN_POINT ( 'NONE',  ( 1.249999999999988898, 12.50000000000000000, -6.560283801567339701 ) ) ;
#60126 = AXIS2_PLACEMENT_3D ( 'NONE', #81432, #22525, #23142 ) ;
#60127 = CARTESIAN_POINT ( 'NONE',  ( 9.349999999999919709, 2.500000000000000000, 1.818653347947321475 ) ) ;
#60128 = LINE ( 'NONE', #70562, #110724 ) ;
#60130 = ORIENTED_EDGE ( 'NONE', *, *, #111932, .F. ) ;
#60129 = ORIENTED_EDGE ( 'NONE', *, *, #101603, .T. ) ;
#60131 = VERTEX_POINT ( 'NONE', #12847 ) ;
#60132 = CARTESIAN_POINT ( 'NONE',  ( -9.350000000000004974, 2.500000000000000000, 6.941600689897073018 ) ) ;
#60133 = CIRCLE ( 'NONE', #35001, 0.06509327318403745899 ) ;
#60134 = CONICAL_SURFACE ( 'NONE', #53854, 0.1000000000000002554, 0.003490658503988666988 ) ;
#60135 = ORIENTED_EDGE ( 'NONE', *, *, #50162, .F. ) ;
#60136 = CARTESIAN_POINT ( 'NONE',  ( 9.149999999999915090, 2.500000000000000000, 6.495190528383297135 ) ) ;
#60137 = AXIS2_PLACEMENT_3D ( 'NONE', #125639, #16318, #114531 ) ;
#60138 = CONICAL_SURFACE ( 'NONE', #39214, 0.09999999999999982514, 0.003490658503988666988 ) ;
#60139 = CARTESIAN_POINT ( 'NONE',  ( -10.45000000000000462, 2.500000000000000000, -6.495190528383298911 ) ) ;
#60140 = CARTESIAN_POINT ( 'NONE',  ( -8.750000000000010658, 12.50000000000000000, -1.407149913249512663 ) ) ;
#60141 = CARTESIAN_POINT ( 'NONE',  ( -1.900000000000034106, 2.500000000000000000, -3.883716857408426648 ) ) ;
#60142 = DIRECTION ( 'NONE',  ( 0.000000000000000000, 0.000000000000000000, -1.000000000000000000 ) ) ;
#60143 = DIRECTION ( 'NONE',  ( -1.084202172485504434E-16, 0.000000000000000000, -1.000000000000000000 ) ) ;
#60144 = VECTOR ( 'NONE', #17583, 1000.000000000000000 ) ;
#60145 = DIRECTION ( 'NONE',  ( 0.000000000000000000, -0.000000000000000000, 1.000000000000000000 ) ) ;
#60146 = EDGE_LOOP ( 'NONE', ( #40471, #89006, #7961, #85291 ) ) ;
#60147 = ORIENTED_EDGE ( 'NONE', *, *, #27415, .F. ) ;
#60148 = DIRECTION ( 'NONE',  ( 0.000000000000000000, 0.000000000000000000, 1.000000000000000000 ) ) ;
#60149 = AXIS2_PLACEMENT_3D ( 'NONE', #80219, #128019, #107735 ) ;
#60150 = VERTEX_POINT ( 'NONE', #101905 ) ;
#60151 =( BOUNDED_CURVE ( )  B_SPLINE_CURVE ( 2, ( #34836, #66193, #83897, #35466, #114022, #74738, #75364, #5974, #36760, #53800, #104815, #95028, #106128, #55098, #115267, #64262, #56373, #5338, #45287, #45933, #6595, #85827, #46548, #25617, #65554, #36106, #63636, #86478, #126417, #113364, #123817, #13869, #93734, #4049, #14505, #74095, #94362, #4674, #69411, #38029, #97590, #18383, #89071, #19017, #28868, #39349, #98877, #58334, #26924, #117864, #89706, #7264, #67460, #66829, #98232, #68772, #68123, #127068, #7913, #108701, #79259, #129021, #37400, #47215, #17060, #58965, #78621, #49164, #8546, #57680, #109344 ),
 .UNSPECIFIED., .F., .F. ) 
 B_SPLINE_CURVE_WITH_KNOTS ( ( 3, 2, 2, 2, 2, 2, 2, 2, 2, 2, 2, 2, 2, 2, 2, 2, 2, 2, 2, 2, 2, 2, 2, 2, 2, 2, 2, 2, 2, 2, 2, 2, 2, 2, 2, 3 ),
 ( 0.000000000000000000, 0.02380952380952380820, 0.04761904761904761640, 0.07142857142857142461, 0.09523809523809523281, 0.1190476190476190271, 0.1428571428571428492, 0.1666666666666666574, 0.1904761904761904656, 0.2142857142857142738, 0.2380952380952380543, 0.2619047619047619180, 0.2857142857142856984, 0.3095238095238095344, 0.3333333333333333148, 0.3571428571428571508, 0.3809523809523809312, 0.4047619047619048227, 0.4285714285714285476, 0.4523809523809523836, 0.4761904761904761085, 0.5000000000000000000, 0.5238095238095238360, 0.5476190476190476719, 0.5714285714285713969, 0.5952380952380952328, 0.6190476190476190688, 0.6428571428571429047, 0.6666666666666666297, 0.6904761904761904656, 0.7142857142857143016, 0.7380952380952382486, 0.7619047619047618625, 0.7857142857142856984, 0.8095238095238096454, 0.8172260697265570917 ),
 .UNSPECIFIED. ) 
 CURVE ( )  GEOMETRIC_REPRESENTATION_ITEM ( )  RATIONAL_B_SPLINE_CURVE ( ( 1.000000000000000000, 0.8660254037844387076, 1.000000000000000000, 0.8660254037844387076, 1.000000000000000000, 0.8660254037844387076, 1.000000000000000000, 0.8660254037844387076, 1.000000000000000000, 0.8660254037844387076, 1.000000000000000000, 0.8660254037844387076, 1.000000000000000000, 0.8660254037844387076, 1.000000000000000000, 0.8660254037844387076, 1.000000000000000000, 0.8660254037844387076, 1.000000000000000000, 0.8660254037844387076, 1.000000000000000000, 0.8660254037844387076, 1.000000000000000000, 0.8660254037844387076, 1.000000000000000000, 0.8660254037844387076, 1.000000000000000000, 0.8660254037844387076, 1.000000000000000000, 0.8660254037844387076, 1.000000000000000000, 0.8660254037844387076, 1.000000000000000000, 0.8660254037844387076, 1.000000000000000000, 0.8660254037844387076, 1.000000000000000000, 0.8660254037844387076, 1.000000000000000000, 0.8660254037844387076, 1.000000000000000000, 0.8660254037844387076, 1.000000000000000000, 0.8660254037844387076, 1.000000000000000000, 0.8660254037844387076, 1.000000000000000000, 0.8660254037844387076, 1.000000000000000000, 0.8660254037844387076, 1.000000000000000000, 0.8660254037844387076, 1.000000000000000000, 0.8660254037844387076, 1.000000000000000000, 0.8660254037844387076, 1.000000000000000000, 0.8660254037844387076, 1.000000000000000000, 0.8660254037844387076, 1.000000000000000000, 0.8660254037844387076, 1.000000000000000000, 0.8660254037844387076, 1.000000000000000000, 0.8660254037844387076, 1.000000000000000000, 0.8660254037844387076, 1.000000000000000000, 0.9566598975743678679, 0.9413604018207953894 ) ) 
 REPRESENTATION_ITEM ( '' )  );
#60152 = VERTEX_POINT ( 'NONE', #122197 ) ;
#60153 = CARTESIAN_POINT ( 'NONE',  ( 186.1093750003413732, 9.264065473108010111E-16, -7.564683531250000925 ) ) ;
#60154 = DIRECTION ( 'NONE',  ( -0.000000000000000000, 1.000000000000000000, -0.000000000000000000 ) ) ;
#60155 = DIRECTION ( 'NONE',  ( 0.000000000000000000, 1.000000000000000000, 0.000000000000000000 ) ) ;
#60156 = DIRECTION ( 'NONE',  ( 0.000000000000000000, 1.000000000000000000, 0.000000000000000000 ) ) ;
#60157 = ADVANCED_FACE ( 'NONE', ( #1753 ), #12218, .T. ) ;
#60158 = CARTESIAN_POINT ( 'NONE',  ( 10.64999999999991331, 2.500000000000000000, -1.818653347947325916 ) ) ;
#60159 = DIRECTION ( 'NONE',  ( -0.000000000000000000, -1.000000000000000000, -0.000000000000000000 ) ) ;
#60160 = DIRECTION ( 'NONE',  ( -0.000000000000000000, -1.000000000000000000, -0.000000000000000000 ) ) ;
#60161 = CIRCLE ( 'NONE', #99860, 0.06509327318403745899 ) ;
#60162 = CARTESIAN_POINT ( 'NONE',  ( 10.64999999999991331, 12.50000000000000000, 6.083687093685483660 ) ) ;
#60163 = ORIENTED_EDGE ( 'NONE', *, *, #126420, .F. ) ;
#60164 = VERTEX_POINT ( 'NONE', #21401 ) ;
#60165 = ORIENTED_EDGE ( 'NONE', *, *, #51232, .T. ) ;
#60166 = ORIENTED_EDGE ( 'NONE', *, *, #111947, .T. ) ;
#60167 = CARTESIAN_POINT ( 'NONE',  ( -4.150000000000027889, 12.50000000000000000, -6.430097255199264339 ) ) ;
#60168 = DIRECTION ( 'NONE',  ( -0.000000000000000000, -1.000000000000000000, -0.000000000000000000 ) ) ;
#60169 = EDGE_LOOP ( 'NONE', ( #96013, #1718, #35478, #115034 ) ) ;
#60170 = AXIS2_PLACEMENT_3D ( 'NONE', #98402, #69597, #80070 ) ;
#60171 = LINE ( 'NONE', #119707, #109225 ) ;
#60173 = CARTESIAN_POINT ( 'NONE',  ( 4.999999999999935163, 2.500000000000000000, 3.537306695894645081 ) ) ;
#60172 = AXIS2_PLACEMENT_3D ( 'NONE', #98308, #7998, #89789 ) ;
#60174 = DIRECTION ( 'NONE',  ( -4.274815082592931898E-19, -0.9999939076577903929, -0.003490651415223739937 ) ) ;
#60176 = VERTEX_POINT ( 'NONE', #61337 ) ;
#60175 = CARTESIAN_POINT ( 'NONE',  ( -9.600000000000008527, 12.50000000000000000, 4.330127018922196314 ) ) ;
#60177 = CARTESIAN_POINT ( 'NONE',  ( -9.350000000000004974, 2.500000000000000000, 6.248780366869521430 ) ) ;
#60178 = AXIS2_PLACEMENT_3D ( 'NONE', #47411, #76866, #87311 ) ;
#60179 = CARTESIAN_POINT ( 'NONE',  ( 11.89999999999990798, 2.500000000000000000, 4.083716857408421497 ) ) ;
#60180 = ORIENTED_EDGE ( 'NONE', *, *, #39381, .F. ) ;
#60181 = CONICAL_SURFACE ( 'NONE', #93612, 0.09999999999999982514, 0.003490658503988666988 ) ;
#60182 = VECTOR ( 'NONE', #128539, 1000.000000000000000 ) ;
#60183 = VERTEX_POINT ( 'NONE', #92732 ) ;
#60184 = ORIENTED_EDGE ( 'NONE', *, *, #5771, .T. ) ;
#60185 = VERTEX_POINT ( 'NONE', #73714 ) ;
#60186 = FACE_OUTER_BOUND ( 'NONE', #12896, .T. ) ;
#60187 = CARTESIAN_POINT ( 'NONE',  ( -4.999999999999986677, 2.500000000000000000, 4.330127018922196314 ) ) ;
#60188 = DIRECTION ( 'NONE',  ( -0.000000000000000000, 1.000000000000000000, -0.000000000000000000 ) ) ;
#60190 = EDGE_CURVE ( 'NONE', #58954, #89885, #113654, .T. ) ;
#60189 = AXIS2_PLACEMENT_3D ( 'NONE', #17710, #37382, #26268 ) ;
#60191 = DIRECTION ( 'NONE',  ( 0.000000000000000000, 0.000000000000000000, 1.000000000000000000 ) ) ;
#60192 = VERTEX_POINT ( 'NONE', #63915 ) ;
#60193 = AXIS2_PLACEMENT_3D ( 'NONE', #32324, #110216, #241 ) ;
#60194 = DIRECTION ( 'NONE',  ( -0.000000000000000000, -1.000000000000000000, -0.000000000000000000 ) ) ;
#60195 = CARTESIAN_POINT ( 'NONE',  ( 11.24999999999994316, 12.50000000000000000, -6.560283801567339701 ) ) ;
#60196 = ADVANCED_FACE ( 'NONE', ( #92067 ), #49110, .T. ) ;
#60197 = DIRECTION ( 'NONE',  ( 0.000000000000000000, 1.000000000000000000, 0.000000000000000000 ) ) ;
#60198 = CARTESIAN_POINT ( 'NONE',  ( 10.84999999999990905, 12.50000000000000000, 1.472243186433545459 ) ) ;
#60199 = EDGE_CURVE ( 'NONE', #9486, #70431, #122267, .T. ) ;
#60200 = ORIENTED_EDGE ( 'NONE', *, *, #49690, .T. ) ;
#60201 = CONICAL_SURFACE ( 'NONE', #97826, 0.1000000000000002554, 0.003490658503988666988 ) ;
#60202 = CARTESIAN_POINT ( 'NONE',  ( 11.24999999999990585, 2.500000000000000000, 2.957883832488649389 ) ) ;
#60203 = AXIS2_PLACEMENT_3D ( 'NONE', #87290, #89873, #127867 ) ;
#60204 = EDGE_LOOP ( 'NONE', ( #84841, #34140, #48171, #10157 ) ) ;
#60205 = ADVANCED_FACE ( 'NONE', ( #103839 ), #82271, .F. ) ;
#60207 = ORIENTED_EDGE ( 'NONE', *, *, #52414, .F. ) ;
#60206 = ADVANCED_FACE ( 'NONE', ( #3066 ), #9391, .T. ) ;
#60208 = DIRECTION ( 'NONE',  ( 0.000000000000000000, 0.000000000000000000, -1.000000000000000000 ) ) ;
#60209 = ADVANCED_FACE ( 'NONE', ( #22071 ), #84683, .T. ) ;
#60210 = DIRECTION ( 'NONE',  ( 0.000000000000000000, 0.000000000000000000, -1.000000000000000000 ) ) ;
#60211 = EDGE_CURVE ( 'NONE', #6145, #46603, #11526, .T. ) ;
#60212 = FACE_BOUND ( 'NONE', #57934, .T. ) ;
#60213 = VECTOR ( 'NONE', #59149, 1000.000000000000000 ) ;
#60214 = DIRECTION ( 'NONE',  ( 0.000000000000000000, -1.000000000000000000, 0.000000000000000000 ) ) ;
#60215 = DIRECTION ( 'NONE',  ( 0.000000000000000000, 1.000000000000000000, 0.000000000000000000 ) ) ;
#60216 = VECTOR ( 'NONE', #8562, 1000.000000000000000 ) ;
#60217 = CARTESIAN_POINT ( 'NONE',  ( 6.249999999999928946, 2.500000000000000000, 2.857883832488649301 ) ) ;
#60218 = CONICAL_SURFACE ( 'NONE', #47682, 0.09999999999999982514, 0.003490658503988666988 ) ;
#60219 = DIRECTION ( 'NONE',  ( 0.000000000000000000, -0.000000000000000000, 1.000000000000000000 ) ) ;
#60220 = DIRECTION ( 'NONE',  ( 0.000000000000000000, -0.000000000000000000, 1.000000000000000000 ) ) ;
#60221 = EDGE_CURVE ( 'NONE', #13533, #35640, #102537, .T. ) ;
#60223 = DIRECTION ( 'NONE',  ( 0.000000000000000000, 0.000000000000000000, -1.000000000000000000 ) ) ;
#60222 = CIRCLE ( 'NONE', #72722, 0.06509327318403745899 ) ;
#60225 = CARTESIAN_POINT ( 'NONE',  ( 9.599999999999917932, 2.500000000000000000, 0.6928203230275494784 ) ) ;
#60224 = AXIS2_PLACEMENT_3D ( 'NONE', #4192, #74248, #124637 ) ;
#60226 = ORIENTED_EDGE ( 'NONE', *, *, #108514, .F. ) ;
#60227 = FACE_OUTER_BOUND ( 'NONE', #3700, .T. ) ;
#60228 = VECTOR ( 'NONE', #101074, 1000.000000000000000 ) ;
#60229 = DIRECTION ( 'NONE',  ( -0.4999999999999471534, -0.000000000000000000, 0.8660254037844692387 ) ) ;
#60230 = ORIENTED_EDGE ( 'NONE', *, *, #38758, .T. ) ;
#60231 = EDGE_LOOP ( 'NONE', ( #118855, #117963, #87621, #112125 ) ) ;
#60232 = DIRECTION ( 'NONE',  ( -0.000000000000000000, 1.000000000000000000, -0.000000000000000000 ) ) ;
#60233 = VECTOR ( 'NONE', #23383, 1000.000000000000000 ) ;
#60234 = CARTESIAN_POINT ( 'NONE',  ( -14.14999999999998614, 2.500000000000000000, -2.065063509461099844 ) ) ;
#60235 = FACE_BOUND ( 'NONE', #32748, .T. ) ;
#60236 = DIRECTION ( 'NONE',  ( 0.000000000000000000, 1.000000000000000000, 0.000000000000000000 ) ) ;
#60238 = CIRCLE ( 'NONE', #85345, 0.06509327318403745899 ) ;
#60237 = CIRCLE ( 'NONE', #76938, 0.06509327318403745899 ) ;
#60239 = CARTESIAN_POINT ( 'NONE',  ( -2.500000000000032863, 2.500000000000000000, 5.122947341949749323 ) ) ;
#60240 = EDGE_LOOP ( 'NONE', ( #60090, #128234, #88438, #50362 ) ) ;
#60242 = EDGE_CURVE ( 'NONE', #77368, #87565, #95256, .T. ) ;
#60241 = DIRECTION ( 'NONE',  ( -0.000000000000000000, -1.000000000000000000, -0.000000000000000000 ) ) ;
#60243 = CARTESIAN_POINT ( 'NONE',  ( 87.50000000000001421, 9.429780353434619030E-16, -7.700000000000000178 ) ) ;
#60244 = ORIENTED_EDGE ( 'NONE', *, *, #123171, .T. ) ;
#60245 = DIRECTION ( 'NONE',  ( 0.000000000000000000, 0.000000000000000000, 1.000000000000000000 ) ) ;
#60246 = CARTESIAN_POINT ( 'NONE',  ( 2.949999999999943334, 2.500000000000000000, 6.495190528383297135 ) ) ;
#60247 = EDGE_CURVE ( 'NONE', #66080, #128722, #81609, .T. ) ;
#60248 = EDGE_CURVE ( 'NONE', #2963, #84112, #84781, .T. ) ;
#60249 = CARTESIAN_POINT ( 'NONE',  ( -14.19999999999998685, 2.500000000000000000, -1.084202172485504434E-16 ) ) ;
#60250 = DIRECTION ( 'NONE',  ( 1.000000000000000000, -0.000000000000000000, -0.000000000000000000 ) ) ;
#60251 = EDGE_CURVE ( 'NONE', #116584, #105882, #71804, .T. ) ;
#60252 = ORIENTED_EDGE ( 'NONE', *, *, #70570, .F. ) ;
#60253 = EDGE_CURVE ( 'NONE', #125089, #63009, #53457, .T. ) ;
#60254 = DIRECTION ( 'NONE',  ( -0.000000000000000000, 1.000000000000000000, -0.000000000000000000 ) ) ;
#60255 = AXIS2_PLACEMENT_3D ( 'NONE', #11127, #31442, #120455 ) ;
#60256 = DIRECTION ( 'NONE',  ( 0.000000000000000000, 0.000000000000000000, 1.000000000000000000 ) ) ;
#60257 = DIRECTION ( 'NONE',  ( -0.000000000000000000, 1.000000000000000000, -0.000000000000000000 ) ) ;
#60258 = EDGE_CURVE ( 'NONE', #92344, #101832, #19946, .T. ) ;
#60259 = ORIENTED_EDGE ( 'NONE', *, *, #16594, .F. ) ;
#60260 = AXIS2_PLACEMENT_3D ( 'NONE', #31909, #71837, #62018 ) ;
#60261 = ORIENTED_EDGE ( 'NONE', *, *, #20947, .F. ) ;
#60262 = ADVANCED_FACE ( 'NONE', ( #55382 ), #55446, .T. ) ;
#60263 = DIRECTION ( 'NONE',  ( 0.000000000000000000, 0.000000000000000000, -1.000000000000000000 ) ) ;
#60265 = VERTEX_POINT ( 'NONE', #105108 ) ;
#60264 = EDGE_CURVE ( 'NONE', #6155, #55060, #76954, .T. ) ;
#60266 = DIRECTION ( 'NONE',  ( -0.000000000000000000, -1.000000000000000000, -0.000000000000000000 ) ) ;
#60267 = CARTESIAN_POINT ( 'NONE',  ( 17.50000000000000000, -2.499999999999999556, -2.333333333333329040 ) ) ;
#60269 = EDGE_CURVE ( 'NONE', #63941, #98238, #126553, .T. ) ;
#60268 = CIRCLE ( 'NONE', #53893, 0.1000000000000002554 ) ;
#60270 = AXIS2_PLACEMENT_3D ( 'NONE', #33249, #51596, #23393 ) ;
#60271 = EDGE_CURVE ( 'NONE', #99984, #54010, #66476, .T. ) ;
#60272 = CARTESIAN_POINT ( 'NONE',  ( 108.0000000000000142, 8.500000000000000000, 0.000000000000000000 ) ) ;
#60273 = ORIENTED_EDGE ( 'NONE', *, *, #52068, .F. ) ;
#60274 = CARTESIAN_POINT ( 'NONE',  ( 7.099999999999928590, 12.50000000000000000, 4.265033745738159077 ) ) ;
#60275 = DIRECTION ( 'NONE',  ( 0.000000000000000000, -0.000000000000000000, 1.000000000000000000 ) ) ;
#60276 = DIRECTION ( 'NONE',  ( 0.000000000000000000, 0.000000000000000000, -1.000000000000000000 ) ) ;
#60277 = DIRECTION ( 'NONE',  ( 0.000000000000000000, 0.000000000000000000, 1.000000000000000000 ) ) ;
#60278 = LINE ( 'NONE', #119167, #19398 ) ;
#60280 = EDGE_CURVE ( 'NONE', #21509, #91809, #107766, .T. ) ;
#60279 = CARTESIAN_POINT ( 'NONE',  ( -10.65000000000000213, 12.50000000000000000, 6.841600689897072485 ) ) ;
#60281 = CONICAL_SURFACE ( 'NONE', #79144, 0.1000000000000002554, 0.003490658503988666988 ) ;
#60282 = ORIENTED_EDGE ( 'NONE', *, *, #47485, .F. ) ;
#60284 = EDGE_LOOP ( 'NONE', ( #13103, #96356 ) ) ;
#60283 = AXIS2_PLACEMENT_3D ( 'NONE', #83802, #72072, #41329 ) ;
#60285 = CARTESIAN_POINT ( 'NONE',  ( -1.250000000000036193, 12.50000000000000000, 5.802370205355744659 ) ) ;
#60286 = ORIENTED_EDGE ( 'NONE', *, *, #60627, .T. ) ;
#60287 = CARTESIAN_POINT ( 'NONE',  ( 7.099999999999928590, 2.500000000000000000, -4.330127018922201643 ) ) ;
#60289 = ORIENTED_EDGE ( 'NONE', *, *, #87978, .F. ) ;
#60288 = VERTEX_POINT ( 'NONE', #96571 ) ;
#60290 = VERTEX_POINT ( 'NONE', #76313 ) ;
#60291 = CARTESIAN_POINT ( 'NONE',  ( 87.50000000000001421, -3.974992050023848922, -6.359987280038160051 ) ) ;
#60293 = DIRECTION ( 'NONE',  ( 0.000000000000000000, -0.000000000000000000, 1.000000000000000000 ) ) ;
#60292 = VECTOR ( 'NONE', #13693, 1000.000000000000000 ) ;
#60294 = FACE_OUTER_BOUND ( 'NONE', #107726, .T. ) ;
#60295 =( NAMED_UNIT ( * ) SI_UNIT ( $, .STERADIAN. ) SOLID_ANGLE_UNIT ( ) );
#60296 = FACE_OUTER_BOUND ( 'NONE', #103250, .T. ) ;
#60297 = DIRECTION ( 'NONE',  ( 0.000000000000000000, 0.000000000000000000, -1.000000000000000000 ) ) ;
#60298 = CARTESIAN_POINT ( 'NONE',  ( 1.899999999999949507, 2.500000000000000000, 4.676537180435972552 ) ) ;
#60299 = CARTESIAN_POINT ( 'NONE',  ( 6.049999999999934097, 2.500000000000000000, -6.148780366869526226 ) ) ;
#60300 = DIRECTION ( 'NONE',  ( 0.000000000000000000, 0.000000000000000000, 1.000000000000000000 ) ) ;
#60301 = DIRECTION ( 'NONE',  ( -4.274815082592931898E-19, -0.9999939076577903929, -0.003490651415223739937 ) ) ;
#60302 = AXIS2_PLACEMENT_3D ( 'NONE', #73181, #5709, #84280 ) ;
#60303 = EDGE_LOOP ( 'NONE', ( #32272, #69078, #88732, #108318 ) ) ;
#60304 = DIRECTION ( 'NONE',  ( 0.000000000000000000, 0.000000000000000000, -1.000000000000000000 ) ) ;
#60305 = ORIENTED_EDGE ( 'NONE', *, *, #27082, .F. ) ;
#60306 = ORIENTED_EDGE ( 'NONE', *, *, #119902, .F. ) ;
#60307 = CARTESIAN_POINT ( 'NONE',  ( -10.40000000000000213, 12.50000000000000000, 4.957854068765711553 ) ) ;
#60308 = AXIS2_PLACEMENT_3D ( 'NONE', #34028, #45151, #73954 ) ;
#60309 = DIRECTION ( 'NONE',  ( -0.000000000000000000, -1.000000000000000000, -0.000000000000000000 ) ) ;
#60311 = CONICAL_SURFACE ( 'NONE', #97934, 0.1000000000000000472, 0.003490658503988666988 ) ;
#60310 = CARTESIAN_POINT ( 'NONE',  ( 186.7812500006828031, 0.000000000000000000, 7.700000000000000178 ) ) ;
#60312 = EDGE_CURVE ( 'NONE', #13780, #74146, #80587, .T. ) ;
#60313 = DIRECTION ( 'NONE',  ( 0.000000000000000000, 0.000000000000000000, 1.000000000000000000 ) ) ;
#60314 = DIRECTION ( 'NONE',  ( 0.000000000000000000, 0.000000000000000000, 1.000000000000000000 ) ) ;
#60315 = CARTESIAN_POINT ( 'NONE',  ( 1.249999999999988454, 2.500000000000000000, 2.265063509461097357 ) ) ;
#60316 = EDGE_LOOP ( 'NONE', ( #30248, #102633, #26575, #42575 ) ) ;
#60317 = AXIS2_PLACEMENT_3D ( 'NONE', #77298, #64889, #117188 ) ;
#60318 = VERTEX_POINT ( 'NONE', #105770 ) ;
#60319 = CARTESIAN_POINT ( 'NONE',  ( -4.150000000000025224, 2.500000000000000000, -1.472243186433550122 ) ) ;
#60320 = ORIENTED_EDGE ( 'NONE', *, *, #112518, .T. ) ;
#60321 = CARTESIAN_POINT ( 'NONE',  ( -7.950000000000009059, 2.500000000000000000, 6.595190528383296780 ) ) ;
#60322 = ORIENTED_EDGE ( 'NONE', *, *, #4794, .F. ) ;
#60323 = AXIS2_PLACEMENT_3D ( 'NONE', #63602, #11908, #72133 ) ;
#60324 = ADVANCED_FACE ( 'NONE', ( #4970 ), #72189, .T. ) ;
#60325 = ORIENTED_EDGE ( 'NONE', *, *, #26819, .T. ) ;
#60326 = CARTESIAN_POINT ( 'NONE',  ( 2.899999999999946620, 2.500000000000000000, 0.6928203230275494784 ) ) ;
#60327 = CARTESIAN_POINT ( 'NONE',  ( 26.74601813931272787, -2.978655629156510276, -2.722801754518478390 ) ) ;
#60328 = CARTESIAN_POINT ( 'NONE',  ( 9.149999999999918643, 2.500000000000000000, -6.495190528383302464 ) ) ;
#60329 = FACE_OUTER_BOUND ( 'NONE', #123297, .T. ) ;
#60330 = CARTESIAN_POINT ( 'NONE',  ( 87.50000000000002842, 2.781865847474099152, 7.000342182495696619 ) ) ;
#60331 = VERTEX_POINT ( 'NONE', #116860 ) ;
#60332 = DIRECTION ( 'NONE',  ( -4.274815082592931898E-19, -0.9999939076577903929, -0.003490651415223739937 ) ) ;
#60333 = DIRECTION ( 'NONE',  ( -0.000000000000000000, 1.000000000000000000, -0.000000000000000000 ) ) ;
#60334 = FACE_OUTER_BOUND ( 'NONE', #88762, .T. ) ;
#60335 = CARTESIAN_POINT ( 'NONE',  ( -12.04999999999999716, 12.50000000000000000, -6.495190528383298911 ) ) ;
#60336 = DIRECTION ( 'NONE',  ( 0.000000000000000000, 1.000000000000000000, 0.000000000000000000 ) ) ;
#60337 = VERTEX_POINT ( 'NONE', #6891 ) ;
#60338 = ORIENTED_EDGE ( 'NONE', *, *, #106059, .F. ) ;
#60339 = AXIS2_PLACEMENT_3D ( 'NONE', #119779, #11757, #121072 ) ;
#60340 = CARTESIAN_POINT ( 'NONE',  ( -8.749999999999971578, 2.500000000000000000, 6.495190528383297135 ) ) ;
#60341 = ORIENTED_EDGE ( 'NONE', *, *, #100274, .T. ) ;
#60342 = CARTESIAN_POINT ( 'NONE',  ( -11.44999999999999751, 2.500000000000000000, 6.148780366869520897 ) ) ;
#60343 = CARTESIAN_POINT ( 'NONE',  ( -6.650000000000018119, 2.500000000000000000, -2.757883832488654097 ) ) ;
#60344 = CIRCLE ( 'NONE', #118809, 0.06509327318403745899 ) ;
#60345 = ADVANCED_FACE ( 'NONE', ( #74373 ), #7396, .T. ) ;
#60346 = CIRCLE ( 'NONE', #102192, 0.06509327318403745899 ) ;
#60347 = CIRCLE ( 'NONE', #3882, 0.09999999999999982514 ) ;
#60348 = VERTEX_POINT ( 'NONE', #5609 ) ;
#60349 = CARTESIAN_POINT ( 'NONE',  ( -11.05000000000000071, 12.50000000000000000, 2.511473670974873507 ) ) ;
#60350 = CARTESIAN_POINT ( 'NONE',  ( -10.40000000000000213, 2.500000000000000000, -2.276824562219559311E-15 ) ) ;
#60351 = DIRECTION ( 'NONE',  ( -0.000000000000000000, -1.000000000000000000, -0.000000000000000000 ) ) ;
#60352 = DIRECTION ( 'NONE',  ( 0.000000000000000000, 0.000000000000000000, 1.000000000000000000 ) ) ;
#60353 = ADVANCED_FACE ( 'NONE', ( #25924 ), #16712, .T. ) ;
#60354 = VECTOR ( 'NONE', #7595, 1000.000000000000000 ) ;
#60355 = AXIS2_PLACEMENT_3D ( 'NONE', #43233, #3924, #74604 ) ;
#60356 = CIRCLE ( 'NONE', #93795, 0.09999999999999999167 ) ;
#60357 = DIRECTION ( 'NONE',  ( 0.000000000000000000, 0.000000000000000000, 1.000000000000000000 ) ) ;
#60358 = CIRCLE ( 'NONE', #20639, 0.06509327318403745899 ) ;
#60359 = ORIENTED_EDGE ( 'NONE', *, *, #75707, .T. ) ;
#60360 = ADVANCED_FACE ( 'NONE', ( #106405 ), #86761, .T. ) ;
#60361 = ADVANCED_FACE ( 'NONE', ( #94010 ), #15717, .T. ) ;
#60362 = EDGE_CURVE ( 'NONE', #11624, #14537, #32489, .T. ) ;
#60364 = EDGE_CURVE ( 'NONE', #85762, #46426, #88895, .T. ) ;
#60363 = CARTESIAN_POINT ( 'NONE',  ( 43.31231356391106857, 3.511368398499961963, -3.941707252993503552 ) ) ;
#60365 = EDGE_CURVE ( 'NONE', #29752, #30275, #76383, .T. ) ;
#60366 = LINE ( 'NONE', #30900, #83307 ) ;
#60367 = VECTOR ( 'NONE', #8822, 1000.000000000000000 ) ;
#60368 = DIRECTION ( 'NONE',  ( 0.000000000000000000, -0.000000000000000000, 1.000000000000000000 ) ) ;
#60369 = CARTESIAN_POINT ( 'NONE',  ( -12.49999999999999289, 2.500000000000000000, -0.5928203230275499447 ) ) ;
#60370 = AXIS2_PLACEMENT_3D ( 'NONE', #115170, #109233, #98775 ) ;
#60371 = EDGE_LOOP ( 'NONE', ( #24049, #2131, #77614, #98881 ) ) ;
#60372 = ORIENTED_EDGE ( 'NONE', *, *, #87527, .F. ) ;
#60373 = FACE_OUTER_BOUND ( 'NONE', #84208, .T. ) ;
#60374 = DIRECTION ( 'NONE',  ( 0.000000000000000000, 1.000000000000000000, 0.000000000000000000 ) ) ;
#60375 = ADVANCED_FACE ( 'NONE', ( #94644 ), #124507, .T. ) ;
#60376 = DIRECTION ( 'NONE',  ( 0.000000000000000000, 1.000000000000000000, 0.000000000000000000 ) ) ;
#60377 = ORIENTED_EDGE ( 'NONE', *, *, #122981, .T. ) ;
#60378 = ADVANCED_FACE ( 'NONE', ( #116218 ), #107041, .T. ) ;
#60380 = EDGE_CURVE ( 'NONE', #114224, #113778, #97873, .T. ) ;
#60379 = PLANE ( 'NONE',  #128376 ) ;
#60381 = DIRECTION ( 'NONE',  ( -0.000000000000000000, 1.000000000000000000, -0.000000000000000000 ) ) ;
#60382 = AXIS2_PLACEMENT_3D ( 'NONE', #119228, #36817, #29559 ) ;
#60383 = VERTEX_POINT ( 'NONE', #10149 ) ;
#60384 = CARTESIAN_POINT ( 'NONE',  ( 5.849999999999932143, 12.50000000000000000, 1.537336459617582918 ) ) ;
#60385 = VERTEX_POINT ( 'NONE', #99827 ) ;
#60386 = CARTESIAN_POINT ( 'NONE',  ( 13.09999999999990195, 2.500000000000000000, -3.983716857408426293 ) ) ;
#60387 = ORIENTED_EDGE ( 'NONE', *, *, #129498, .F. ) ;
#60388 = VECTOR ( 'NONE', #26504, 1000.000000000000000 ) ;
#60389 = CARTESIAN_POINT ( 'NONE',  ( 2.049999999999948308, 12.50000000000000000, 6.430097255199259010 ) ) ;
#60390 = DIRECTION ( 'NONE',  ( 0.000000000000000000, 0.000000000000000000, -1.000000000000000000 ) ) ;
#60391 = ORIENTED_EDGE ( 'NONE', *, *, #66047, .T. ) ;
#60392 = ORIENTED_EDGE ( 'NONE', *, *, #48595, .T. ) ;
#60393 = CARTESIAN_POINT ( 'NONE',  ( 9.149999999999920419, 2.500000000000000000, 2.757883832488649656 ) ) ;
#60394 = CARTESIAN_POINT ( 'NONE',  ( -1.322875655532295136, -2.500000000000000444, -5.000000000000004441 ) ) ;
#60395 = CIRCLE ( 'NONE', #91476, 0.06509327318403745899 ) ;
#60396 = VERTEX_POINT ( 'NONE', #127986 ) ;
#60397 = DIRECTION ( 'NONE',  ( 0.000000000000000000, -0.000000000000000000, 1.000000000000000000 ) ) ;
#60398 = CARTESIAN_POINT ( 'NONE',  ( 187.2760416670080588, 6.551208109652274736, 3.782341765625001351 ) ) ;
#60399 = AXIS2_PLACEMENT_3D ( 'NONE', #112662, #64834, #55015 ) ;
#60400 = FACE_OUTER_BOUND ( 'NONE', #21974, .T. ) ;
#60401 = CARTESIAN_POINT ( 'NONE',  ( 107.6624854834585250, 7.119691004531023992, 5.000000000000003553 ) ) ;
#60402 = CARTESIAN_POINT ( 'NONE',  ( 7.099999999999925926, 2.500000000000000000, 0.6928203230275494784 ) ) ;
#60403 = CARTESIAN_POINT ( 'NONE',  ( 4.799999999999937650, 2.500000000000000000, -0.2464101615137782308 ) ) ;
#60404 = DIRECTION ( 'NONE',  ( 0.000000000000000000, 1.000000000000000000, 0.000000000000000000 ) ) ;
#60405 = ORIENTED_EDGE ( 'NONE', *, *, #55756, .T. ) ;
#60406 = EDGE_LOOP ( 'NONE', ( #65729, #42670, #99590, #84511 ) ) ;
#60408 = VECTOR ( 'NONE', #128141, 1000.000000000000000 ) ;
#60407 = CIRCLE ( 'NONE', #10217, 0.1000000000000000472 ) ;
#60409 = ORIENTED_EDGE ( 'NONE', *, *, #90299, .T. ) ;
#60410 = LINE ( 'NONE', #90472, #41321 ) ;
#60411 = DIRECTION ( 'NONE',  ( -0.000000000000000000, 1.000000000000000000, -0.000000000000000000 ) ) ;
#60412 = FACE_OUTER_BOUND ( 'NONE', #58802, .T. ) ;
#60413 = CONICAL_SURFACE ( 'NONE', #20690, 0.1000000000000002554, 0.003490658503988666988 ) ;
#60415 = ORIENTED_EDGE ( 'NONE', *, *, #64225, .T. ) ;
#60414 = ORIENTED_EDGE ( 'NONE', *, *, #111334, .F. ) ;
#60416 = FACE_BOUND ( 'NONE', #113104, .T. ) ;
#60417 = ORIENTED_EDGE ( 'NONE', *, *, #15607, .F. ) ;
#60418 = EDGE_CURVE ( 'NONE', #123363, #73897, #45087, .T. ) ;
#60419 = CARTESIAN_POINT ( 'NONE',  ( -8.749999999999971578, 12.50000000000000000, 6.430097255199259010 ) ) ;
#60420 = CARTESIAN_POINT ( 'NONE',  ( 7.299999999999927880, 2.500000000000000000, -4.776537180435977525 ) ) ;
#60421 = ADVANCED_FACE ( 'NONE', ( #59269 ), #57603, .T. ) ;
#60422 = CARTESIAN_POINT ( 'NONE',  ( 8.349999999999923261, 12.50000000000000000, 2.165063509461097713 ) ) ;
#60425 = LINE ( 'NONE', #116244, #128835 ) ;
#60424 = AXIS2_PLACEMENT_3D ( 'NONE', #123588, #42481, #114415 ) ;
#60423 = CIRCLE ( 'NONE', #50053, 0.06509327318403745899 ) ;
#60426 = EDGE_CURVE ( 'NONE', #28650, #64939, #86831, .T. ) ;
#60427 = CARTESIAN_POINT ( 'NONE',  ( -12.09999999999999432, 2.500000000000000000, 3.737306695894644371 ) ) ;
#60428 = DIRECTION ( 'NONE',  ( -0.000000000000000000, 1.000000000000000000, -0.000000000000000000 ) ) ;
#60429 = DIRECTION ( 'NONE',  ( 0.000000000000000000, 0.000000000000000000, 1.000000000000000000 ) ) ;
#60430 = DIRECTION ( 'NONE',  ( -4.274815082592931898E-19, -0.9999939076577903929, -0.003490651415223739937 ) ) ;
#60432 = ADVANCED_FACE ( 'NONE', ( #80180 ), #38998, .T. ) ;
#60431 = CARTESIAN_POINT ( 'NONE',  ( 5.849999999999934808, 2.500000000000000000, -5.802370205355749988 ) ) ;
#60433 = EDGE_LOOP ( 'NONE', ( #64819, #71278, #109671, #89109 ) ) ;
#60434 = EDGE_LOOP ( 'NONE', ( #20831, #30571 ) ) ;
#60435 = VERTEX_POINT ( 'NONE', #50097 ) ;
#60436 = ORIENTED_EDGE ( 'NONE', *, *, #9217, .F. ) ;
#60437 = DIRECTION ( 'NONE',  ( 0.000000000000000000, 0.000000000000000000, -1.000000000000000000 ) ) ;
#60438 = AXIS2_PLACEMENT_3D ( 'NONE', #28029, #46363, #118336 ) ;
#60439 = CARTESIAN_POINT ( 'NONE',  ( -1.650000000000034328, 12.50000000000000000, -7.188010851410854052 ) ) ;
#60441 = VERTEX_POINT ( 'NONE', #40261 ) ;
#60440 = ORIENTED_EDGE ( 'NONE', *, *, #118604, .T. ) ;
#60442 = ORIENTED_EDGE ( 'NONE', *, *, #93887, .F. ) ;
#60443 = DIRECTION ( 'NONE',  ( -4.274815082592931898E-19, -0.9999939076577903929, -0.003490651415223739937 ) ) ;
#60444 = VECTOR ( 'NONE', #116491, 1000.000000000000000 ) ;
#60445 = CIRCLE ( 'NONE', #12383, 0.06509327318403745899 ) ;
#60446 = FACE_OUTER_BOUND ( 'NONE', #31347, .T. ) ;
#60447 = CARTESIAN_POINT ( 'NONE',  ( 186.0000000000000000, 0.000000000000000000, 7.700000000000000178 ) ) ;
#60448 = CARTESIAN_POINT ( 'NONE',  ( 7.899999999999924860, 2.500000000000000000, 3.737306695894644371 ) ) ;
#60449 = DIRECTION ( 'NONE',  ( 0.000000000000000000, 0.000000000000000000, 1.000000000000000000 ) ) ;
#60450 = CARTESIAN_POINT ( 'NONE',  ( -6.700000000000019718, 12.50000000000000000, 0.06509327318403504425 ) ) ;
#60451 = CARTESIAN_POINT ( 'NONE',  ( -15.59999999999998010, 12.50000000000000000, 0.3464101615137759604 ) ) ;
#60452 = ADVANCED_FACE ( 'NONE', ( #78261 ), #91043, .T. ) ;
#60453 = ORIENTED_EDGE ( 'NONE', *, *, #10352, .T. ) ;
#60454 = AXIS2_PLACEMENT_3D ( 'NONE', #66416, #57909, #87972 ) ;
#60456 = DIRECTION ( 'NONE',  ( -0.000000000000000000, -1.000000000000000000, -0.000000000000000000 ) ) ;
#60455 = CIRCLE ( 'NONE', #120974, 0.06509327318403741736 ) ;
#60457 = VERTEX_POINT ( 'NONE', #30455 ) ;
#60458 = AXIS2_PLACEMENT_3D ( 'NONE', #107428, #17075, #57694 ) ;
#60459 = ORIENTED_EDGE ( 'NONE', *, *, #32132, .T. ) ;
#60460 = ORIENTED_EDGE ( 'NONE', *, *, #25619, .F. ) ;
#60461 = DIRECTION ( 'NONE',  ( 0.000000000000000000, 0.000000000000000000, 1.000000000000000000 ) ) ;
#60462 = ORIENTED_EDGE ( 'NONE', *, *, #12258, .T. ) ;
#60463 = ORIENTED_EDGE ( 'NONE', *, *, #82880, .F. ) ;
#60464 = AXIS2_PLACEMENT_3D ( 'NONE', #28338, #98341, #67592 ) ;
#60465 = PRESENTATION_STYLE_ASSIGNMENT (( #21819 ) ) ;
#60466 = AXIS2_PLACEMENT_3D ( 'NONE', #73192, #41819, #52267 ) ;
#60467 = CARTESIAN_POINT ( 'NONE',  ( -5.850000000000019185, 2.500000000000000000, 6.495190528383297135 ) ) ;
#60468 = CARTESIAN_POINT ( 'NONE',  ( 3.749999999999976907, 2.500000000000000000, 2.165063509461097713 ) ) ;
#60469 = EDGE_CURVE ( 'NONE', #36953, #32790, #28354, .T. ) ;
#60470 = CARTESIAN_POINT ( 'NONE',  ( -11.84999999999999787, 2.500000000000000000, -1.818653347947321919 ) ) ;
#60471 = DIRECTION ( 'NONE',  ( 0.000000000000000000, 0.000000000000000000, -1.000000000000000000 ) ) ;
#60472 = CARTESIAN_POINT ( 'NONE',  ( 6.849999999999927702, 12.50000000000000000, 2.446380397790835826 ) ) ;
#60473 = DIRECTION ( 'NONE',  ( 0.000000000000000000, -0.9999939076577903929, 0.003490651415223739937 ) ) ;
#60474 = ORIENTED_EDGE ( 'NONE', *, *, #79692, .F. ) ;
#60475 = DIRECTION ( 'NONE',  ( 0.000000000000000000, 0.000000000000000000, -1.000000000000000000 ) ) ;
#60476 = EDGE_LOOP ( 'NONE', ( #67539, #58302, #88436, #98507 ) ) ;
#60477 = CARTESIAN_POINT ( 'NONE',  ( 112.9654443591792159, 8.680014631837170924, -0.6741253490163554574 ) ) ;
#60478 = CARTESIAN_POINT ( 'NONE',  ( 0.4499999999999569344, 2.500000000000000000, -2.265063509461101798 ) ) ;
#60479 = AXIS2_PLACEMENT_3D ( 'NONE', #66997, #126589, #48035 ) ;
#60480 = ORIENTED_EDGE ( 'NONE', *, *, #116798, .F. ) ;
#60481 = CARTESIAN_POINT ( 'NONE',  ( -6.650000000000015454, 2.500000000000000000, 2.857883832488649301 ) ) ;
#60482 = ADVANCED_FACE ( 'NONE', ( #19972 ), #27848, .T. ) ;
#60483 = DIRECTION ( 'NONE',  ( -0.000000000000000000, -1.000000000000000000, -0.000000000000000000 ) ) ;
#60484 = ORIENTED_EDGE ( 'NONE', *, *, #62978, .F. ) ;
#60485 = DIRECTION ( 'NONE',  ( 0.000000000000000000, 1.000000000000000000, 0.000000000000000000 ) ) ;
#60486 = ORIENTED_EDGE ( 'NONE', *, *, #64937, .T. ) ;
#60487 = EDGE_LOOP ( 'NONE', ( #55482, #40221, #41544, #79664 ) ) ;
#60488 = CARTESIAN_POINT ( 'NONE',  ( 4.149999999999939959, 2.500000000000000000, 1.372243186433545370 ) ) ;
#60489 = DIRECTION ( 'NONE',  ( -0.000000000000000000, 1.000000000000000000, -0.000000000000000000 ) ) ;
#60490 = CARTESIAN_POINT ( 'NONE',  ( 184.9635416670080872, -4.367472073101519747, 7.564683531249999149 ) ) ;
#60492 = CIRCLE ( 'NONE', #62629, 0.06509327318403745899 ) ;
#60491 = LINE ( 'NONE', #83345, #74358 ) ;
#60493 = AXIS2_PLACEMENT_3D ( 'NONE', #12822, #80488, #70643 ) ;
#60494 = DIRECTION ( 'NONE',  ( 0.000000000000000000, 0.000000000000000000, 1.000000000000000000 ) ) ;
#60495 = ORIENTED_EDGE ( 'NONE', *, *, #25960, .F. ) ;
#60496 = CARTESIAN_POINT ( 'NONE',  ( -11.84999999999999787, 2.500000000000000000, -6.148780366869522673 ) ) ;
#60497 = AXIS2_PLACEMENT_3D ( 'NONE', #36927, #29046, #6776 ) ;
#60498 = EDGE_LOOP ( 'NONE', ( #44011, #125722, #28242, #80947 ) ) ;
#60499 = CARTESIAN_POINT ( 'NONE',  ( -10.60000000000000142, 2.500000000000000000, 3.983716857408420964 ) ) ;
#60500 = CARTESIAN_POINT ( 'NONE',  ( 7.499999999999961808, 2.500000000000000000, -4.430127018922202176 ) ) ;
#60501 = ADVANCED_FACE ( 'NONE', ( #29160 ), #61811, .T. ) ;
#60502 = AXIS2_PLACEMENT_3D ( 'NONE', #66581, #47607, #19408 ) ;
#60503 = CARTESIAN_POINT ( 'NONE',  ( 186.2135416670080872, 4.367472073101518859, -7.564683531249999149 ) ) ;
#60504 = DIRECTION ( 'NONE',  ( 0.000000000000000000, 1.000000000000000000, 0.000000000000000000 ) ) ;
#60505 = LINE ( 'NONE', #100413, #71609 ) ;
#60506 = CARTESIAN_POINT ( 'NONE',  ( 107.5000000000000142, 0.000000000000000000, 0.000000000000000000 ) ) ;
#60507 = DIRECTION ( 'NONE',  ( 0.000000000000000000, -0.9999939076577903929, 0.003490651415223739937 ) ) ;
#60508 = EDGE_LOOP ( 'NONE', ( #8640, #83828 ) ) ;
#60509 = EDGE_CURVE ( 'NONE', #41032, #120360, #78545, .T. ) ;
#60511 = AXIS2_PLACEMENT_3D ( 'NONE', #109765, #19431, #39116 ) ;
#60510 = CIRCLE ( 'NONE', #58360, 0.06509327318403745899 ) ;
#60512 = CARTESIAN_POINT ( 'NONE',  ( 184.5000000000000000, 0.000000000000000000, 7.700000000000000178 ) ) ;
#60513 = CARTESIAN_POINT ( 'NONE',  ( 0.5999999999999621192, 2.500000000000000000, 0.3464101615137758494 ) ) ;
#60514 = PLANE ( 'NONE',  #60126 ) ;
#60515 = EDGE_CURVE ( 'NONE', #3042, #96780, #26303, .T. ) ;
#60516 = EDGE_CURVE ( 'NONE', #53654, #90160, #57965, .T. ) ;
#60517 = ADVANCED_FACE ( 'NONE', ( #8201 ), #48144, .T. ) ;
#60518 = EDGE_CURVE ( 'NONE', #55240, #74476, #39638, .T. ) ;
#60519 = VERTEX_POINT ( 'NONE', #98504 ) ;
#60520 = DIRECTION ( 'NONE',  ( 0.000000000000000000, 0.000000000000000000, 1.000000000000000000 ) ) ;
#60521 = ORIENTED_EDGE ( 'NONE', *, *, #23228, .F. ) ;
#60522 = EDGE_LOOP ( 'NONE', ( #49646, #53881, #127856, #77986 ) ) ;
#60523 = DIRECTION ( 'NONE',  ( 0.000000000000000000, 0.000000000000000000, 1.000000000000000000 ) ) ;
#60524 = EDGE_CURVE ( 'NONE', #79739, #74262, #128731, .T. ) ;
#60525 = CIRCLE ( 'NONE', #108522, 0.1000000000000000056 ) ;
#60526 = EDGE_CURVE ( 'NONE', #76809, #57584, #82745, .T. ) ;
#60527 = ORIENTED_EDGE ( 'NONE', *, *, #21332, .T. ) ;
#60528 = DIRECTION ( 'NONE',  ( 0.000000000000000000, 1.000000000000000000, 0.000000000000000000 ) ) ;
#60529 = DIRECTION ( 'NONE',  ( -0.000000000000000000, 1.000000000000000000, -0.000000000000000000 ) ) ;
#60530 = ADVANCED_FACE ( 'NONE', ( #93227 ), #15815, .T. ) ;
#60531 = VERTEX_POINT ( 'NONE', #13356 ) ;
#60532 = EDGE_CURVE ( 'NONE', #85431, #112209, #93200, .T. ) ;
#60533 = AXIS2_PLACEMENT_3D ( 'NONE', #69010, #128618, #79497 ) ;
#60535 = ADVANCED_FACE ( 'NONE', ( #122043 ), #82108, .T. ) ;
#60534 = FACE_OUTER_BOUND ( 'NONE', #7337, .T. ) ;
#60536 = AXIS2_PLACEMENT_3D ( 'NONE', #36500, #17463, #56728 ) ;
#60537 = CARTESIAN_POINT ( 'NONE',  ( -0.6000000000000388356, 2.500000000000000000, 3.983716857408420964 ) ) ;
#60538 = CARTESIAN_POINT ( 'NONE',  ( 16.98713586915526008, -1.503435535905108811, -5.629434499184605478 ) ) ;
#60539 = EDGE_CURVE ( 'NONE', #99244, #93665, #52638, .T. ) ;
#60540 = CIRCLE ( 'NONE', #56297, 0.06509327318403745899 ) ;
#60541 = VERTEX_POINT ( 'NONE', #32397 ) ;
#60542 = AXIS2_PLACEMENT_3D ( 'NONE', #105191, #112456, #44335 ) ;
#60543 = AXIS2_PLACEMENT_3D ( 'NONE', #55114, #95684, #5351 ) ;
#60544 = ORIENTED_EDGE ( 'NONE', *, *, #11419, .F. ) ;
#60545 = ORIENTED_EDGE ( 'NONE', *, *, #106009, .F. ) ;
#60546 = DIRECTION ( 'NONE',  ( 0.000000000000000000, 0.000000000000000000, 1.000000000000000000 ) ) ;
#60547 = PLANE ( 'NONE',  #104350 ) ;
#60548 = DIRECTION ( 'NONE',  ( 0.000000000000000000, 0.000000000000000000, 1.000000000000000000 ) ) ;
#60549 = FACE_BOUND ( 'NONE', #35515, .T. ) ;
#60550 = ORIENTED_EDGE ( 'NONE', *, *, #28645, .T. ) ;
#60551 = AXIS2_PLACEMENT_3D ( 'NONE', #102231, #14463, #125085 ) ;
#60552 = DIRECTION ( 'NONE',  ( 0.000000000000000000, 1.000000000000000000, 0.000000000000000000 ) ) ;
#60553 = DIRECTION ( 'NONE',  ( -4.274815082592931898E-19, -0.9999939076577903929, -0.003490651415223739937 ) ) ;
#60554 = ORIENTED_EDGE ( 'NONE', *, *, #116220, .F. ) ;
#60555 = CARTESIAN_POINT ( 'NONE',  ( -7.500000000000013323, 2.500000000000000000, 5.122947341949749323 ) ) ;
#60556 = DIRECTION ( 'NONE',  ( 0.000000000000000000, 0.000000000000000000, -1.000000000000000000 ) ) ;
#60557 = VECTOR ( 'NONE', #77411, 1000.000000000000000 ) ;
#60558 = CARTESIAN_POINT ( 'NONE',  ( 6.249999999999930722, 2.500000000000000000, -1.472243186433550122 ) ) ;
#60559 = DIRECTION ( 'NONE',  ( 0.000000000000000000, 1.000000000000000000, 0.000000000000000000 ) ) ;
#60560 = DIRECTION ( 'NONE',  ( 0.000000000000000000, 1.000000000000000000, 0.000000000000000000 ) ) ;
#60561 = DIRECTION ( 'NONE',  ( -0.000000000000000000, 1.000000000000000000, -0.000000000000000000 ) ) ;
#60562 = DIRECTION ( 'NONE',  ( 0.000000000000000000, 0.000000000000000000, -1.000000000000000000 ) ) ;
#60563 = EDGE_LOOP ( 'NONE', ( #81977, #36599 ) ) ;
#60564 = ORIENTED_EDGE ( 'NONE', *, *, #43732, .F. ) ;
#60565 = ORIENTED_EDGE ( 'NONE', *, *, #107661, .F. ) ;
#60566 = ORIENTED_EDGE ( 'NONE', *, *, #41056, .F. ) ;
#60567 = AXIS2_PLACEMENT_3D ( 'NONE', #51265, #29669, #851 ) ;
#60568 = FACE_OUTER_BOUND ( 'NONE', #115950, .T. ) ;
#60569 = DIRECTION ( 'NONE',  ( 0.000000000000000000, 1.000000000000000000, 0.000000000000000000 ) ) ;
#60570 = ORIENTED_EDGE ( 'NONE', *, *, #41608, .T. ) ;
#60571 = FACE_BOUND ( 'NONE', #88839, .T. ) ;
#60572 = CARTESIAN_POINT ( 'NONE',  ( -4.600000000000024514, 2.500000000000000000, 5.022947341949748790 ) ) ;
#60573 = EDGE_CURVE ( 'NONE', #39657, #46373, #1601, .T. ) ;
#60574 = LINE ( 'NONE', #37842, #42925 ) ;
#60575 = LINE ( 'NONE', #40940, #59610 ) ;
#60576 = EDGE_CURVE ( 'NONE', #129477, #47052, #61841, .T. ) ;
#60577 = DIRECTION ( 'NONE',  ( 0.000000000000000000, -0.9999939076577903929, 0.003490651415223739937 ) ) ;
#60578 = DIRECTION ( 'NONE',  ( 0.000000000000000000, 1.000000000000000000, 0.000000000000000000 ) ) ;
#60579 = DIRECTION ( 'NONE',  ( -4.274815082592931898E-19, -0.9999939076577903929, -0.003490651415223739937 ) ) ;
#60580 = DIRECTION ( 'NONE',  ( 0.000000000000000000, 0.000000000000000000, 1.000000000000000000 ) ) ;
#60581 = APPLICATION_CONTEXT ( 'automotive_design' ) ;
#60582 = FACE_OUTER_BOUND ( 'NONE', #36620, .T. ) ;
#60583 = VERTEX_POINT ( 'NONE', #112219 ) ;
#60584 = EDGE_CURVE ( 'NONE', #7881, #125498, #13752, .T. ) ;
#60585 = EDGE_LOOP ( 'NONE', ( #19352, #19022 ) ) ;
#60586 = VERTEX_POINT ( 'NONE', #42861 ) ;
#60587 = VERTEX_POINT ( 'NONE', #2912 ) ;
#60588 = ORIENTED_EDGE ( 'NONE', *, *, #80197, .T. ) ;
#60589 = ORIENTED_EDGE ( 'NONE', *, *, #51343, .F. ) ;
#60590 = CARTESIAN_POINT ( 'NONE',  ( -4.350000000000027178, 12.50000000000000000, -6.148780366869526226 ) ) ;
#60591 = AXIS2_PLACEMENT_3D ( 'NONE', #15646, #128876, #80401 ) ;
#60592 = EDGE_LOOP ( 'NONE', ( #92899, #21920 ) ) ;
#60595 = AXIS2_PLACEMENT_3D ( 'NONE', #36395, #57958, #117475 ) ;
#60594 = DIRECTION ( 'NONE',  ( 0.000000000000000000, 0.000000000000000000, -1.000000000000000000 ) ) ;
#60593 = CIRCLE ( 'NONE', #6256, 0.1000000000000002554 ) ;
#60596 = CARTESIAN_POINT ( 'NONE',  ( 186.0677083336747444, -4.367472073101514418, -7.564683531250002702 ) ) ;
#60597 = CARTESIAN_POINT ( 'NONE',  ( -11.69999999999999929, 12.50000000000000000, 1.734723475976807094E-15 ) ) ;
#60598 = CARTESIAN_POINT ( 'NONE',  ( -4.350000000000027178, 2.500000000000000000, -6.148780366869526226 ) ) ;
#60599 = CIRCLE ( 'NONE', #114846, 0.1000000000000000056 ) ;
#60600 = ORIENTED_EDGE ( 'NONE', *, *, #89790, .F. ) ;
#60601 = FACE_OUTER_BOUND ( 'NONE', #78699, .T. ) ;
#60603 = CIRCLE ( 'NONE', #81429, 0.1000000000000000056 ) ;
#60602 = CONICAL_SURFACE ( 'NONE', #119073, 0.09999999999999982514, 0.003490658503988666988 ) ;
#60604 = ORIENTED_EDGE ( 'NONE', *, *, #93804, .T. ) ;
#60605 = ORIENTED_EDGE ( 'NONE', *, *, #126097, .T. ) ;
#60606 = CARTESIAN_POINT ( 'NONE',  ( 14.54999999999989235, 12.50000000000000000, -2.165063509461101710 ) ) ;
#60607 = CARTESIAN_POINT ( 'NONE',  ( 3.349999999999945466, 2.500000000000000000, -7.088010851410853519 ) ) ;
#60608 = DIRECTION ( 'NONE',  ( 0.000000000000000000, 1.000000000000000000, 0.000000000000000000 ) ) ;
#60609 = EDGE_LOOP ( 'NONE', ( #30948, #26890, #122163, #114453 ) ) ;
#60610 = EDGE_LOOP ( 'NONE', ( #59012, #80153, #13024, #126310 ) ) ;
#60611 = ADVANCED_FACE ( 'NONE', ( #101754 ), #62486, .T. ) ;
#60612 = CARTESIAN_POINT ( 'NONE',  ( 1.249999999999988454, 2.500000000000000000, 2.165063509461097713 ) ) ;
#60613 = DIRECTION ( 'NONE',  ( 0.000000000000000000, 0.000000000000000000, 1.000000000000000000 ) ) ;
#60614 = CARTESIAN_POINT ( 'NONE',  ( -3.750000000000027534, 12.50000000000000000, 2.857883832488649301 ) ) ;
#60615 = DIRECTION ( 'NONE',  ( 0.000000000000000000, -0.9999939076577903929, 0.003490651415223739937 ) ) ;
#60616 = ORIENTED_EDGE ( 'NONE', *, *, #121482, .F. ) ;
#60617 = DIRECTION ( 'NONE',  ( -4.274815082592931898E-19, -0.9999939076577903929, -0.003490651415223739937 ) ) ;
#60618 = ORIENTED_EDGE ( 'NONE', *, *, #117330, .T. ) ;
#60619 = CARTESIAN_POINT ( 'NONE',  ( 1.899999999999951283, 2.500000000000000000, 0.3464101615137736845 ) ) ;
#60620 = CIRCLE ( 'NONE', #91903, 0.1000000000000000056 ) ;
#60621 = CIRCLE ( 'NONE', #39784, 0.1000000000000000056 ) ;
#60622 = ORIENTED_EDGE ( 'NONE', *, *, #16024, .T. ) ;
#60623 = FACE_OUTER_BOUND ( 'NONE', #686, .T. ) ;
#60624 = CARTESIAN_POINT ( 'NONE',  ( 48.81613170260295220, -3.619496531216669588, 4.312669415525522965 ) ) ;
#60625 = DIRECTION ( 'NONE',  ( -0.000000000000000000, 1.000000000000000000, -0.000000000000000000 ) ) ;
#60626 = EDGE_CURVE ( 'NONE', #65247, #123233, #53306, .T. ) ;
#60627 = EDGE_CURVE ( 'NONE', #18103, #3294, #105718, .T. ) ;
#60628 = CARTESIAN_POINT ( 'NONE',  ( 12.04999999999990834, 2.500000000000000000, -2.165063509461101710 ) ) ;
#60629 = EDGE_LOOP ( 'NONE', ( #121931, #84454 ) ) ;
#60630 = AXIS2_PLACEMENT_3D ( 'NONE', #57702, #97612, #7933 ) ;
#60631 = CARTESIAN_POINT ( 'NONE',  ( -11.89999999999999503, 2.500000000000000000, 3.983716857408420076 ) ) ;
#60632 = CARTESIAN_POINT ( 'NONE',  ( 0.6499999999999561684, 12.50000000000000000, -2.446380397790840266 ) ) ;
#60633 = EDGE_LOOP ( 'NONE', ( #127318, #94706, #72592, #116714 ) ) ;
#60634 = VERTEX_POINT ( 'NONE', #122674 ) ;
#60636 = VERTEX_POINT ( 'NONE', #72933 ) ;
#60635 = ADVANCED_FACE ( 'NONE', ( #20619 ), #65994, .T. ) ;
#60637 = LINE ( 'NONE', #42276, #1868 ) ;
#60638 = DIRECTION ( 'NONE',  ( 0.000000000000000000, 0.000000000000000000, 1.000000000000000000 ) ) ;
#60639 = DIRECTION ( 'NONE',  ( -0.000000000000000000, -1.000000000000000000, -0.000000000000000000 ) ) ;
#60640 = AXIS2_PLACEMENT_3D ( 'NONE', #55694, #50245, #28670 ) ;
#60641 = DIRECTION ( 'NONE',  ( 0.000000000000000000, 0.000000000000000000, 1.000000000000000000 ) ) ;
#60642 = FACE_OUTER_BOUND ( 'NONE', #85993, .T. ) ;
#60643 = AXIS2_PLACEMENT_3D ( 'NONE', #127144, #38113, #85269 ) ;
#60644 = CARTESIAN_POINT ( 'NONE',  ( -1.250000000000001554, 2.500000000000000000, 6.495190528383297135 ) ) ;
#60645 = DIRECTION ( 'NONE',  ( -4.274815082592931898E-19, -0.9999939076577903929, -0.003490651415223739937 ) ) ;
#60646 = DIRECTION ( 'NONE',  ( -4.274815082592931898E-19, -0.9999939076577903929, -0.003490651415223739937 ) ) ;
#60647 = VECTOR ( 'NONE', #36759, 1000.000000000000000 ) ;
#60648 = CONICAL_SURFACE ( 'NONE', #35511, 0.09999999999999982514, 0.003490658503988666988 ) ;
#60649 = VERTEX_POINT ( 'NONE', #10755 ) ;
#60650 = CONICAL_SURFACE ( 'NONE', #16784, 0.1000000000000002554, 0.003490658503988666988 ) ;
#60651 = DIRECTION ( 'NONE',  ( -0.000000000000000000, 1.000000000000000000, -0.000000000000000000 ) ) ;
#60652 = CARTESIAN_POINT ( 'NONE',  ( 12.09999999999990550, 2.500000000000000000, 5.022947341949748790 ) ) ;
#60653 = LINE ( 'NONE', #88805, #61055 ) ;
#60654 = PLANE ( 'NONE',  #73001 ) ;
#60655 = EDGE_LOOP ( 'NONE', ( #69774, #125883, #6004, #122950 ) ) ;
#60656 = DIRECTION ( 'NONE',  ( -0.000000000000000000, 1.000000000000000000, -0.000000000000000000 ) ) ;
#60657 = EDGE_CURVE ( 'NONE', #60435, #53973, #99466, .T. ) ;
#60658 = DIRECTION ( 'NONE',  ( 0.000000000000000000, 1.000000000000000000, 0.000000000000000000 ) ) ;
#60660 = ORIENTED_EDGE ( 'NONE', *, *, #75964, .T. ) ;
#60659 = DIRECTION ( 'NONE',  ( 0.000000000000000000, 0.000000000000000000, 1.000000000000000000 ) ) ;
#60661 = ADVANCED_FACE ( 'NONE', ( #63106 ), #57696, .T. ) ;
#60662 = EDGE_CURVE ( 'NONE', #121281, #25124, #55628, .T. ) ;
#60663 = EDGE_LOOP ( 'NONE', ( #99352, #109817 ) ) ;
#60664 = DIRECTION ( 'NONE',  ( 0.000000000000000000, 0.000000000000000000, -1.000000000000000000 ) ) ;
#60665 = EDGE_LOOP ( 'NONE', ( #90424, #121582 ) ) ;
#60666 = ORIENTED_EDGE ( 'NONE', *, *, #95915, .F. ) ;
#60667 = CARTESIAN_POINT ( 'NONE',  ( -11.64999999999999680, 12.50000000000000000, -2.857883832488649745 ) ) ;
#60668 = EDGE_CURVE ( 'NONE', #111704, #90001, #70206, .T. ) ;
#60669 = CIRCLE ( 'NONE', #35626, 0.1000000000000000472 ) ;
#60670 = EDGE_CURVE ( 'NONE', #82618, #90496, #74223, .T. ) ;
#60671 = ADVANCED_FACE ( 'NONE', ( #124614 ), #72277, .T. ) ;
#60672 = CARTESIAN_POINT ( 'NONE',  ( 20.25366426269120268, 2.573118374676206521, -4.179292740213720769 ) ) ;
#60673 = CARTESIAN_POINT ( 'NONE',  ( 1.449999999999949551, 12.50000000000000000, 6.776507416713035248 ) ) ;
#60674 = CARTESIAN_POINT ( 'NONE',  ( -10.40000000000000213, 2.500000000000000000, -5.022947341949749678 ) ) ;
#60675 = ORIENTED_EDGE ( 'NONE', *, *, #67722, .T. ) ;
#60678 = ADVANCED_FACE ( 'NONE', ( #26419 ), #84680, .T. ) ;
#60677 = AXIS2_PLACEMENT_3D ( 'NONE', #24468, #31715, #13344 ) ;
#60676 = AXIS2_PLACEMENT_3D ( 'NONE', #55179, #63063, #102980 ) ;
#60679 = CARTESIAN_POINT ( 'NONE',  ( 184.5833333333333144, -6.668395609140180369, 3.849999999999994760 ) ) ;
#60680 = ORIENTED_EDGE ( 'NONE', *, *, #97497, .T. ) ;
#60681 = DIRECTION ( 'NONE',  ( 0.000000000000000000, 1.000000000000000000, 0.000000000000000000 ) ) ;
#60682 = DIRECTION ( 'NONE',  ( 0.000000000000000000, -1.000000000000000000, 0.000000000000000000 ) ) ;
#60683 = EDGE_CURVE ( 'NONE', #9406, #46747, #104945, .T. ) ;
#60684 = CARTESIAN_POINT ( 'NONE',  ( 16.68631762705459565, -1.607367762587846860, 5.954228785335645924 ) ) ;
#60685 = EDGE_CURVE ( 'NONE', #109850, #61759, #34961, .T. ) ;
#60686 = VERTEX_POINT ( 'NONE', #44773 ) ;
#60687 = VECTOR ( 'NONE', #16500, 1000.000000000000000 ) ;
#60688 = EDGE_LOOP ( 'NONE', ( #75859, #34303, #6087, #118816 ) ) ;
#60689 = ORIENTED_EDGE ( 'NONE', *, *, #123662, .T. ) ;
#60690 = ORIENTED_EDGE ( 'NONE', *, *, #118861, .F. ) ;
#60691 = CARTESIAN_POINT ( 'NONE',  ( 12.09999999999990195, 12.50000000000000000, 0.6928203230275494784 ) ) ;
#60692 = CARTESIAN_POINT ( 'NONE',  ( 15.22989033483572996, 1.499999999999839462, 7.180069493258938174 ) ) ;
#60693 = FACE_OUTER_BOUND ( 'NONE', #73016, .T. ) ;
#60694 = FACE_BOUND ( 'NONE', #113638, .T. ) ;
#60695 = CARTESIAN_POINT ( 'NONE',  ( 6.449999999999931788, 2.500000000000000000, 6.248780366869520542 ) ) ;
#60696 = CARTESIAN_POINT ( 'NONE',  ( 186.9895833340161460, -4.445597072760115509, -7.700000000000001954 ) ) ;
#60697 = FACE_OUTER_BOUND ( 'NONE', #119443, .T. ) ;
#60698 = CARTESIAN_POINT ( 'NONE',  ( -2.950000000000029932, 2.500000000000000000, -2.165063509461101710 ) ) ;
#60699 = CARTESIAN_POINT ( 'NONE',  ( 8.349999999999919709, 2.500000000000000000, -2.757883832488654097 ) ) ;
#60700 = CARTESIAN_POINT ( 'NONE',  ( -10.65000000000000391, 2.500000000000000000, -2.611473670974873595 ) ) ;
#60701 = CARTESIAN_POINT ( 'NONE',  ( 9.999999999999916511, 12.50000000000000000, -0.6928203230275541413 ) ) ;
#60702 = CARTESIAN_POINT ( 'NONE',  ( -1.650000000000034772, 12.50000000000000000, 2.230156782645134950 ) ) ;
#60703 = ORIENTED_EDGE ( 'NONE', *, *, #33682, .T. ) ;
#60704 = ORIENTED_EDGE ( 'NONE', *, *, #51468, .F. ) ;
#60705 = ORIENTED_EDGE ( 'NONE', *, *, #30718, .F. ) ;
#60706 = EDGE_LOOP ( 'NONE', ( #18864, #10002, #119136, #26820 ) ) ;
#60707 = CARTESIAN_POINT ( 'NONE',  ( 2.899999999999944844, 12.50000000000000000, 3.637306695894644726 ) ) ;
#60708 = PLANE ( 'NONE',  #19499 ) ;
#60709 = ORIENTED_EDGE ( 'NONE', *, *, #98487, .F. ) ;
#60710 = FACE_BOUND ( 'NONE', #29005, .T. ) ;
#60711 = CIRCLE ( 'NONE', #94148, 0.1000000000000002554 ) ;
#60712 = CARTESIAN_POINT ( 'NONE',  ( 8.149999999999920419, 12.50000000000000000, -1.883746621131363375 ) ) ;
#60713 = EDGE_CURVE ( 'NONE', #10391, #60441, #109926, .T. ) ;
#60714 = ORIENTED_EDGE ( 'NONE', *, *, #64480, .T. ) ;
#60715 = LINE ( 'NONE', #109143, #11205 ) ;
#60716 = CARTESIAN_POINT ( 'NONE',  ( 8.099999999999921485, 2.500000000000000000, 0.2464101615137735679 ) ) ;
#60717 = DIRECTION ( 'NONE',  ( 0.000000000000000000, -0.9999939076577903929, 0.003490651415223739937 ) ) ;
#60718 = DIRECTION ( 'NONE',  ( -0.000000000000000000, -1.000000000000000000, -0.000000000000000000 ) ) ;
#60719 = ORIENTED_EDGE ( 'NONE', *, *, #73193, .F. ) ;
#60720 = CARTESIAN_POINT ( 'NONE',  ( -11.44999999999999751, 2.500000000000000000, 6.048780366869521252 ) ) ;
#60721 = EDGE_CURVE ( 'NONE', #56093, #27833, #74870, .T. ) ;
#60722 = AXIS2_PLACEMENT_3D ( 'NONE', #55654, #26201, #36680 ) ;
#60723 = ORIENTED_EDGE ( 'NONE', *, *, #109906, .F. ) ;
#60724 = ORIENTED_EDGE ( 'NONE', *, *, #96682, .T. ) ;
#60725 = DIRECTION ( 'NONE',  ( -0.000000000000000000, 1.000000000000000000, -0.000000000000000000 ) ) ;
#60726 = DIRECTION ( 'NONE',  ( 0.000000000000000000, 0.000000000000000000, -1.000000000000000000 ) ) ;
#60727 = VERTEX_POINT ( 'NONE', #116071 ) ;
#60728 = LINE ( 'NONE', #117185, #114313 ) ;
#60729 = CONICAL_SURFACE ( 'NONE', #66956, 0.1000000000000000472, 0.003490658503988666988 ) ;
#60730 = DIRECTION ( 'NONE',  ( 0.000000000000000000, 0.000000000000000000, 1.000000000000000000 ) ) ;
#60731 = CARTESIAN_POINT ( 'NONE',  ( -0.6000000000000383915, 12.50000000000000000, -4.611443907251939756 ) ) ;
#60732 = DIRECTION ( 'NONE',  ( 0.000000000000000000, 1.000000000000000000, 0.000000000000000000 ) ) ;
#60733 = VECTOR ( 'NONE', #30124, 1000.000000000000000 ) ;
#60734 = VERTEX_POINT ( 'NONE', #65680 ) ;
#60735 = FACE_OUTER_BOUND ( 'NONE', #35721, .T. ) ;
#60736 = VERTEX_POINT ( 'NONE', #44113 ) ;
#60737 = DIRECTION ( 'NONE',  ( -0.000000000000000000, -1.000000000000000000, -0.000000000000000000 ) ) ;
#60738 = ORIENTED_EDGE ( 'NONE', *, *, #60364, .T. ) ;
#60739 = DIRECTION ( 'NONE',  ( 0.000000000000000000, 0.000000000000000000, -1.000000000000000000 ) ) ;
#60740 = ORIENTED_EDGE ( 'NONE', *, *, #86057, .T. ) ;
#60741 = DIRECTION ( 'NONE',  ( -0.000000000000000000, -1.000000000000000000, -0.000000000000000000 ) ) ;
#60742 = CARTESIAN_POINT ( 'NONE',  ( -0.2000000000000404232, 2.500000000000000000, 3.883716857408421319 ) ) ;
#60743 = CARTESIAN_POINT ( 'NONE',  ( 8.949999999999917577, 2.500000000000000000, 6.248780366869520542 ) ) ;
#60744 = FACE_OUTER_BOUND ( 'NONE', #36915, .T. ) ;
#60745 = CARTESIAN_POINT ( 'NONE',  ( -10.60000000000000142, 2.500000000000000000, -0.3464101615137782364 ) ) ;
#60746 = EDGE_LOOP ( 'NONE', ( #6921, #32079, #19496, #11388 ) ) ;
#60747 = ORIENTED_EDGE ( 'NONE', *, *, #74092, .T. ) ;
#60749 = ORIENTED_EDGE ( 'NONE', *, *, #111327, .F. ) ;
#60748 = EDGE_CURVE ( 'NONE', #52226, #60021, #7498, .T. ) ;
#60750 = DIRECTION ( 'NONE',  ( 0.000000000000000000, 0.000000000000000000, 1.000000000000000000 ) ) ;
#60751 = CARTESIAN_POINT ( 'NONE',  ( 1.449999999999951328, 12.50000000000000000, 2.511473670974873507 ) ) ;
#60752 = DIRECTION ( 'NONE',  ( -0.000000000000000000, 1.000000000000000000, -0.000000000000000000 ) ) ;
#60754 = ORIENTED_EDGE ( 'NONE', *, *, #108778, .T. ) ;
#60753 = VERTEX_POINT ( 'NONE', #14630 ) ;
#60755 = VERTEX_POINT ( 'NONE', #73558 ) ;
#60756 = AXIS2_PLACEMENT_3D ( 'NONE', #18732, #68471, #78964 ) ;
#60757 = DIRECTION ( 'NONE',  ( 0.000000000000000000, 1.000000000000000000, 0.000000000000000000 ) ) ;
#60758 = EDGE_LOOP ( 'NONE', ( #93942, #30521, #100971, #6871 ) ) ;
#60760 = EDGE_CURVE ( 'NONE', #15697, #119380, #126647, .T. ) ;
#60759 = DIRECTION ( 'NONE',  ( 0.000000000000000000, 0.000000000000000000, -1.000000000000000000 ) ) ;
#60761 = AXIS2_PLACEMENT_3D ( 'NONE', #19087, #79344, #30252 ) ;
#60762 = FACE_OUTER_BOUND ( 'NONE', #83837, .T. ) ;
#60763 = DIRECTION ( 'NONE',  ( 0.000000000000000000, 0.000000000000000000, -1.000000000000000000 ) ) ;
#60764 = DIRECTION ( 'NONE',  ( 0.000000000000000000, 0.000000000000000000, 1.000000000000000000 ) ) ;
#60765 = CARTESIAN_POINT ( 'NONE',  ( 185.6249999999999716, -8.891194145520236347, -1.633285867636356299E-15 ) ) ;
#60766 = FACE_OUTER_BOUND ( 'NONE', #121659, .T. ) ;
#60767 = EDGE_CURVE ( 'NONE', #12520, #77015, #30523, .T. ) ;
#60768 = ADVANCED_FACE ( 'NONE', ( #85951 ), #34317, .T. ) ;
#60769 = LINE ( 'NONE', #39861, #49989 ) ;
#60770 = EDGE_LOOP ( 'NONE', ( #92416, #37513, #16951, #96375 ) ) ;
#60771 = EDGE_LOOP ( 'NONE', ( #116409, #108219, #39749, #3474 ) ) ;
#60772 = DIRECTION ( 'NONE',  ( 0.000000000000000000, 1.000000000000000000, 0.000000000000000000 ) ) ;
#60773 = EDGE_CURVE ( 'NONE', #125197, #109336, #107855, .T. ) ;
#60774 = FACE_OUTER_BOUND ( 'NONE', #58296, .T. ) ;
#60775 = ORIENTED_EDGE ( 'NONE', *, *, #31810, .T. ) ;
#60776 = ORIENTED_EDGE ( 'NONE', *, *, #108373, .T. ) ;
#60777 = ADVANCED_FACE ( 'NONE', ( #65017 ), #4170, .T. ) ;
#60778 = CARTESIAN_POINT ( 'NONE',  ( 186.8177083336747160, 4.367472073101515306, 7.564683531250000925 ) ) ;
#60779 = DIRECTION ( 'NONE',  ( 0.000000000000000000, 1.000000000000000000, 0.000000000000000000 ) ) ;
#60780 = DIRECTION ( 'NONE',  ( 0.000000000000000000, 0.000000000000000000, -1.000000000000000000 ) ) ;
#60781 = CARTESIAN_POINT ( 'NONE',  ( 10.64999999999990976, 2.500000000000000000, 2.611473670974873151 ) ) ;
#60782 = DIRECTION ( 'NONE',  ( 0.000000000000000000, 0.000000000000000000, -1.000000000000000000 ) ) ;
#60783 = CARTESIAN_POINT ( 'NONE',  ( 5.199999999999933564, 12.50000000000000000, 3.918623584224382839 ) ) ;
#60784 = LINE ( 'NONE', #1211, #42752 ) ;
#60785 = CARTESIAN_POINT ( 'NONE',  ( -9.350000000000006750, 2.500000000000000000, -1.718653347947325827 ) ) ;
#60786 = CARTESIAN_POINT ( 'NONE',  ( 183.8593750003413732, 0.000000000000000000, 7.564683531250000925 ) ) ;
#60787 = CIRCLE ( 'NONE', #69170, 0.06509327318403745899 ) ;
#60788 = ORIENTED_EDGE ( 'NONE', *, *, #36635, .T. ) ;
#60790 = ORIENTED_EDGE ( 'NONE', *, *, #76784, .F. ) ;
#60789 = AXIS2_PLACEMENT_3D ( 'NONE', #109866, #71217, #89573 ) ;
#60791 = EDGE_CURVE ( 'NONE', #19759, #21177, #114148, .T. ) ;
#60792 = ORIENTED_EDGE ( 'NONE', *, *, #119046, .F. ) ;
#60793 = VERTEX_POINT ( 'NONE', #13993 ) ;
#60794 = EDGE_LOOP ( 'NONE', ( #15929, #103235 ) ) ;
#60795 = CARTESIAN_POINT ( 'NONE',  ( 2.699999999999945555, 2.500000000000000000, 3.983716857408420076 ) ) ;
#60796 = CARTESIAN_POINT ( 'NONE',  ( -2.300000000000033573, 12.50000000000000000, 4.676537180435972552 ) ) ;
#60797 = AXIS2_PLACEMENT_3D ( 'NONE', #58734, #97362, #58094 ) ;
#60798 = VERTEX_POINT ( 'NONE', #86607 ) ;
#60799 = CARTESIAN_POINT ( 'NONE',  ( -10.40000000000000213, 12.50000000000000000, -5.022947341949749678 ) ) ;
#60800 = EDGE_CURVE ( 'NONE', #39517, #34970, #68137, .T. ) ;
#60801 = FACE_OUTER_BOUND ( 'NONE', #74611, .T. ) ;
#60803 = ORIENTED_EDGE ( 'NONE', *, *, #85329, .T. ) ;
#60802 = CARTESIAN_POINT ( 'NONE',  ( 0.6499999999999561684, 12.50000000000000000, -2.511473670974877948 ) ) ;
#60804 = EDGE_CURVE ( 'NONE', #31864, #97088, #28449, .T. ) ;
#60805 = DIRECTION ( 'NONE',  ( 0.000000000000000000, 1.000000000000000000, 0.000000000000000000 ) ) ;
#60806 = ADVANCED_FACE ( 'NONE', ( #4815 ), #38937, .T. ) ;
#60807 = CARTESIAN_POINT ( 'NONE',  ( -1.250000000000037970, 12.50000000000000000, 7.188010851410848723 ) ) ;
#60808 = VECTOR ( 'NONE', #62116, 1000.000000000000000 ) ;
#60809 = ORIENTED_EDGE ( 'NONE', *, *, #125520, .T. ) ;
#60810 = VECTOR ( 'NONE', #105758, 1000.000000000000000 ) ;
#60811 = ORIENTED_EDGE ( 'NONE', *, *, #69034, .T. ) ;
#60812 = ORIENTED_EDGE ( 'NONE', *, *, #74092, .F. ) ;
#60813 = EDGE_LOOP ( 'NONE', ( #3502, #74401, #28300, #83624 ) ) ;
#60814 = CARTESIAN_POINT ( 'NONE',  ( 10.79999999999991367, 2.500000000000000000, 0.09999999999999761857 ) ) ;
#60815 = EDGE_CURVE ( 'NONE', #19198, #50142, #69543, .T. ) ;
#60816 = ADVANCED_FACE ( 'NONE', ( #128505 ), #38839, .F. ) ;
#60818 = ADVANCED_FACE ( 'NONE', ( #59761 ), #80778, .T. ) ;
#60817 = VECTOR ( 'NONE', #10291, 1000.000000000000000 ) ;
#60819 = DIRECTION ( 'NONE',  ( 0.000000000000000000, 0.000000000000000000, 1.000000000000000000 ) ) ;
#60820 = DIRECTION ( 'NONE',  ( 0.000000000000000000, 1.000000000000000000, 0.000000000000000000 ) ) ;
#60821 = EDGE_CURVE ( 'NONE', #100917, #47413, #20124, .T. ) ;
#60822 = AXIS2_PLACEMENT_3D ( 'NONE', #71008, #113496, #21915 ) ;
#60823 = CARTESIAN_POINT ( 'NONE',  ( -8.550000000000007816, 2.500000000000000000, 6.148780366869520009 ) ) ;
#60824 = ORIENTED_EDGE ( 'NONE', *, *, #116079, .T. ) ;
#60825 = DIRECTION ( 'NONE',  ( 0.000000000000000000, 0.000000000000000000, 1.000000000000000000 ) ) ;
#60826 = DIRECTION ( 'NONE',  ( -0.000000000000000000, -1.000000000000000000, -0.000000000000000000 ) ) ;
#60827 = DIRECTION ( 'NONE',  ( 0.000000000000000000, 0.000000000000000000, -1.000000000000000000 ) ) ;
#60828 = FACE_OUTER_BOUND ( 'NONE', #120467, .T. ) ;
#60829 = EDGE_CURVE ( 'NONE', #62165, #31928, #87016, .T. ) ;
#60830 = ORIENTED_EDGE ( 'NONE', *, *, #88120, .F. ) ;
#60831 = EDGE_CURVE ( 'NONE', #90527, #113115, #78754, .T. ) ;
#60832 = VERTEX_POINT ( 'NONE', #99670 ) ;
#60833 = EDGE_LOOP ( 'NONE', ( #99588, #34673 ) ) ;
#60834 = CARTESIAN_POINT ( 'NONE',  ( -0.8000000000000381251, 12.50000000000000000, 4.330127018922196314 ) ) ;
#60835 = DIRECTION ( 'NONE',  ( -0.000000000000000000, -1.000000000000000000, -0.000000000000000000 ) ) ;
#60836 = FACE_BOUND ( 'NONE', #103328, .T. ) ;
#60837 = PLANE ( 'NONE',  #105725 ) ;
#60838 = CARTESIAN_POINT ( 'NONE',  ( 13.14999999999989733, 2.500000000000000000, -1.918653347947325782 ) ) ;
#60839 = CARTESIAN_POINT ( 'NONE',  ( -5.850000000000021849, 2.500000000000000000, -1.372243186433550033 ) ) ;
#60840 = CIRCLE ( 'NONE', #54481, 0.06509327318403745899 ) ;
#60841 = CIRCLE ( 'NONE', #4375, 0.06509327318403743123 ) ;
#60843 = VECTOR ( 'NONE', #42919, 1000.000000000000000 ) ;
#60842 = DIRECTION ( 'NONE',  ( 0.000000000000000000, 0.000000000000000000, 1.000000000000000000 ) ) ;
#60844 = DIRECTION ( 'NONE',  ( 0.000000000000000000, 1.000000000000000000, 0.000000000000000000 ) ) ;
#60845 = DIRECTION ( 'NONE',  ( -0.000000000000000000, -1.000000000000000000, -0.000000000000000000 ) ) ;
#60846 = ORIENTED_EDGE ( 'NONE', *, *, #10373, .T. ) ;
#60847 = DIRECTION ( 'NONE',  ( -0.000000000000000000, 1.000000000000000000, -0.000000000000000000 ) ) ;
#60848 = AXIS2_PLACEMENT_3D ( 'NONE', #125674, #75937, #28144 ) ;
#60849 = CARTESIAN_POINT ( 'NONE',  ( 3.299999999999944755, 12.50000000000000000, -0.06509327318403980434 ) ) ;
#60850 = VERTEX_POINT ( 'NONE', #28998 ) ;
#60851 = ORIENTED_EDGE ( 'NONE', *, *, #8362, .F. ) ;
#60852 = VECTOR ( 'NONE', #2291, 1000.000000000000000 ) ;
#60853 = DIRECTION ( 'NONE',  ( -0.000000000000000000, 1.000000000000000000, -0.000000000000000000 ) ) ;
#60854 = DIRECTION ( 'NONE',  ( 0.000000000000000000, 0.000000000000000000, -1.000000000000000000 ) ) ;
#60855 = FACE_BOUND ( 'NONE', #82065, .T. ) ;
#60856 = CARTESIAN_POINT ( 'NONE',  ( -9.600000000000006750, 12.50000000000000000, 0.6928203230275494784 ) ) ;
#60857 = DIRECTION ( 'NONE',  ( 0.000000000000000000, 0.000000000000000000, -1.000000000000000000 ) ) ;
#60858 = EDGE_CURVE ( 'NONE', #12489, #90022, #66083, .T. ) ;
#60859 = EDGE_LOOP ( 'NONE', ( #86665, #123827 ) ) ;
#60860 = CARTESIAN_POINT ( 'NONE',  ( -11.25000000000000178, 2.500000000000000000, -1.472243186433546125 ) ) ;
#60861 = CARTESIAN_POINT ( 'NONE',  ( 184.9166666666666856, 6.668395609140176816, 3.850000000000000977 ) ) ;
#60862 = ORIENTED_EDGE ( 'NONE', *, *, #46249, .T. ) ;
#60863 = LINE ( 'NONE', #61528, #51137 ) ;
#60864 = CARTESIAN_POINT ( 'NONE',  ( -8.100000000000013856, 12.50000000000000000, -4.611443907251939756 ) ) ;
#60865 = EDGE_CURVE ( 'NONE', #103728, #64891, #99557, .T. ) ;
#60866 = CONICAL_SURFACE ( 'NONE', #118167, 0.1000000000000002554, 0.003490658503988666988 ) ;
#60867 = PLANE ( 'NONE',  #107140 ) ;
#60868 = DIRECTION ( 'NONE',  ( 0.000000000000000000, 0.000000000000000000, -1.000000000000000000 ) ) ;
#60869 = AXIS2_PLACEMENT_3D ( 'NONE', #47759, #118416, #87659 ) ;
#60870 = AXIS2_PLACEMENT_3D ( 'NONE', #95377, #126119, #25328 ) ;
#60871 = EDGE_LOOP ( 'NONE', ( #129028, #3526, #9278, #100939 ) ) ;
#60872 = LINE ( 'NONE', #100778, #88468 ) ;
#60873 = DIRECTION ( 'NONE',  ( 0.000000000000000000, 0.000000000000000000, 1.000000000000000000 ) ) ;
#60874 = CARTESIAN_POINT ( 'NONE',  ( 10.84999999999991260, 2.500000000000000000, -2.065063509461102065 ) ) ;
#60875 = EDGE_LOOP ( 'NONE', ( #22967, #83257, #67885, #10434 ) ) ;
#60876 = ORIENTED_EDGE ( 'NONE', *, *, #60670, .F. ) ;
#60877 = FACE_OUTER_BOUND ( 'NONE', #86847, .T. ) ;
#60878 = CIRCLE ( 'NONE', #108894, 0.06509327318403745899 ) ;
#60879 = ORIENTED_EDGE ( 'NONE', *, *, #105898, .F. ) ;
#60880 = DIRECTION ( 'NONE',  ( 0.000000000000000000, -0.000000000000000000, 1.000000000000000000 ) ) ;
#60881 = VECTOR ( 'NONE', #49202, 1000.000000000000000 ) ;
#60882 = FACE_OUTER_BOUND ( 'NONE', #81217, .T. ) ;
#60883 = CARTESIAN_POINT ( 'NONE',  ( -13.94999999999998685, 2.500000000000000000, 1.818653347947325472 ) ) ;
#60884 = ORIENTED_EDGE ( 'NONE', *, *, #69631, .F. ) ;
#60885 = DIRECTION ( 'NONE',  ( 0.000000000000000000, 0.000000000000000000, -1.000000000000000000 ) ) ;
#60886 = FACE_OUTER_BOUND ( 'NONE', #26311, .T. ) ;
#60887 = DIRECTION ( 'NONE',  ( -0.000000000000000000, -1.000000000000000000, -0.000000000000000000 ) ) ;
#60888 = CARTESIAN_POINT ( 'NONE',  ( 12.09999999999990550, 12.50000000000000000, 4.330127018922196314 ) ) ;
#60889 = DIRECTION ( 'NONE',  ( -0.000000000000000000, 1.000000000000000000, -0.000000000000000000 ) ) ;
#60890 = LINE ( 'NONE', #83756, #36902 ) ;
#60891 = AXIS2_PLACEMENT_3D ( 'NONE', #78382, #79026, #89474 ) ;
#60892 = ORIENTED_EDGE ( 'NONE', *, *, #46707, .T. ) ;
#60893 = ORIENTED_EDGE ( 'NONE', *, *, #32174, .T. ) ;
#60894 = LINE ( 'NONE', #2602, #64132 ) ;
#60895 = ORIENTED_EDGE ( 'NONE', *, *, #99780, .F. ) ;
#60896 = DIRECTION ( 'NONE',  ( -4.274815082592931898E-19, -0.9999939076577903929, -0.003490651415223739937 ) ) ;
#60898 = EDGE_LOOP ( 'NONE', ( #118257, #48481 ) ) ;
#60897 = ORIENTED_EDGE ( 'NONE', *, *, #63455, .T. ) ;
#60899 = ORIENTED_EDGE ( 'NONE', *, *, #104987, .T. ) ;
#60900 = CARTESIAN_POINT ( 'NONE',  ( 3.149999999999946176, 12.50000000000000000, -2.576566944158915184 ) ) ;
#60901 = AXIS2_PLACEMENT_3D ( 'NONE', #50229, #99322, #9643 ) ;
#60903 = EDGE_CURVE ( 'NONE', #18843, #72282, #36858, .T. ) ;
#60902 = DIRECTION ( 'NONE',  ( 0.000000000000000000, 1.000000000000000000, 0.000000000000000000 ) ) ;
#60904 = DIRECTION ( 'NONE',  ( -0.000000000000000000, 1.000000000000000000, -0.000000000000000000 ) ) ;
#60905 = LINE ( 'NONE', #121118, #89049 ) ;
#60906 = AXIS2_PLACEMENT_3D ( 'NONE', #116073, #123956, #95794 ) ;
#60907 = CONICAL_SURFACE ( 'NONE', #33721, 0.09999999999999982514, 0.003490658503988666988 ) ;
#60908 = DIRECTION ( 'NONE',  ( 0.000000000000000000, -0.9999939076577903929, 0.003490651415223739937 ) ) ;
#60909 = CARTESIAN_POINT ( 'NONE',  ( -9.600000000000006750, 2.500000000000000000, 5.022947341949748790 ) ) ;
#60910 = CARTESIAN_POINT ( 'NONE',  ( -13.94999999999998863, 2.500000000000000000, 2.511473670974877503 ) ) ;
#60911 = DIRECTION ( 'NONE',  ( 0.000000000000000000, -0.000000000000000000, 1.000000000000000000 ) ) ;
#60912 = EDGE_CURVE ( 'NONE', #25279, #52919, #19139, .T. ) ;
#60913 = ADVANCED_FACE ( 'NONE', ( #76803 ), #107952, .T. ) ;
#60914 = CARTESIAN_POINT ( 'NONE',  ( -11.89999999999999503, 2.500000000000000000, 4.776537180435972196 ) ) ;
#60915 = VERTEX_POINT ( 'NONE', #49293 ) ;
#60916 = EDGE_CURVE ( 'NONE', #10113, #12902, #70304, .T. ) ;
#60918 = EDGE_CURVE ( 'NONE', #54077, #30501, #55709, .T. ) ;
#60917 = FACE_OUTER_BOUND ( 'NONE', #43708, .T. ) ;
#60919 = ORIENTED_EDGE ( 'NONE', *, *, #73660, .F. ) ;
#60920 = ORIENTED_EDGE ( 'NONE', *, *, #106727, .T. ) ;
#60921 = EDGE_CURVE ( 'NONE', #127834, #100677, #66954, .T. ) ;
#60922 = CARTESIAN_POINT ( 'NONE',  ( -9.800000000000004263, 2.500000000000000000, -0.3464101615137783474 ) ) ;
#60923 = LINE ( 'NONE', #30843, #61217 ) ;
#60924 = LINE ( 'NONE', #128409, #83858 ) ;
#60925 = CARTESIAN_POINT ( 'NONE',  ( 10.84999999999991260, 2.500000000000000000, -2.957883832488653830 ) ) ;
#60926 = LINE ( 'NONE', #79925, #84549 ) ;
#60927 = AXIS2_PLACEMENT_3D ( 'NONE', #45164, #106010, #107288 ) ;
#60928 = DIRECTION ( 'NONE',  ( 0.000000000000000000, -0.000000000000000000, 1.000000000000000000 ) ) ;
#60929 = ORIENTED_EDGE ( 'NONE', *, *, #71233, .T. ) ;
#60930 = AXIS2_PLACEMENT_3D ( 'NONE', #51139, #723, #40685 ) ;
#60931 = VERTEX_POINT ( 'NONE', #57155 ) ;
#60932 = DIRECTION ( 'NONE',  ( 0.000000000000000000, -1.000000000000000000, 0.000000000000000000 ) ) ;
#60933 = AXIS2_PLACEMENT_3D ( 'NONE', #92874, #34611, #81739 ) ;
#60934 = ORIENTED_EDGE ( 'NONE', *, *, #91534, .F. ) ;
#60936 = CARTESIAN_POINT ( 'NONE',  ( 5.599999999999933031, 12.50000000000000000, -0.3464101615137783474 ) ) ;
#60935 = AXIS2_PLACEMENT_3D ( 'NONE', #31288, #100639, #10953 ) ;
#60937 = ORIENTED_EDGE ( 'NONE', *, *, #48525, .F. ) ;
#60938 = AXIS2_PLACEMENT_3D ( 'NONE', #58521, #7452, #8731 ) ;
#60939 = EDGE_LOOP ( 'NONE', ( #82815, #7025 ) ) ;
#60940 = DIRECTION ( 'NONE',  ( 0.000000000000000000, -0.9999939076577903929, 0.003490651415223739937 ) ) ;
#60941 = DIRECTION ( 'NONE',  ( 0.000000000000000000, 0.000000000000000000, 1.000000000000000000 ) ) ;
#60942 = DIRECTION ( 'NONE',  ( -0.000000000000000000, 1.000000000000000000, -0.000000000000000000 ) ) ;
#60943 = DIRECTION ( 'NONE',  ( 0.000000000000000000, 0.000000000000000000, 1.000000000000000000 ) ) ;
#60944 = FACE_OUTER_BOUND ( 'NONE', #51435, .T. ) ;
#60945 = EDGE_LOOP ( 'NONE', ( #102343, #115092 ) ) ;
#60946 = CARTESIAN_POINT ( 'NONE',  ( 2.699999999999947331, 12.50000000000000000, -4.611443907251940644 ) ) ;
#60947 = CARTESIAN_POINT ( 'NONE',  ( 1.449999999999951772, 12.50000000000000000, -6.083687093685488989 ) ) ;
#60948 = DIRECTION ( 'NONE',  ( 0.000000000000000000, 0.000000000000000000, 1.000000000000000000 ) ) ;
#60949 = FACE_OUTER_BOUND ( 'NONE', #123446, .T. ) ;
#60950 = CARTESIAN_POINT ( 'NONE',  ( -5.850000000000021849, 12.50000000000000000, -5.802370205355749988 ) ) ;
#60951 = ORIENTED_EDGE ( 'NONE', *, *, #96058, .F. ) ;
#60952 = ORIENTED_EDGE ( 'NONE', *, *, #44711, .F. ) ;
#60953 = VERTEX_POINT ( 'NONE', #127202 ) ;
#60954 = EDGE_CURVE ( 'NONE', #82935, #22615, #37531, .T. ) ;
#60955 = PLANE ( 'NONE',  #111473 ) ;
#60956 = EDGE_CURVE ( 'NONE', #100324, #82878, #107550, .T. ) ;
#60957 = EDGE_CURVE ( 'NONE', #29934, #45445, #116255, .T. ) ;
#60958 = EDGE_LOOP ( 'NONE', ( #102711, #42895, #47049, #126724 ) ) ;
#60959 = CARTESIAN_POINT ( 'NONE',  ( 16.55874544816229132, -0.4845305829427751232, 6.091953208798936537 ) ) ;
#60960 = AXIS2_PLACEMENT_3D ( 'NONE', #48240, #18772, #26030 ) ;
#60961 = FACE_OUTER_BOUND ( 'NONE', #76429, .T. ) ;
#60962 = AXIS2_PLACEMENT_3D ( 'NONE', #35033, #55931, #84756 ) ;
#60963 = ADVANCED_FACE ( 'NONE', ( #78091 ), #57784, .T. ) ;
#60964 = ADVANCED_FACE ( 'NONE', ( #70202 ), #31568, .T. ) ;
#60965 = EDGE_LOOP ( 'NONE', ( #57529, #112712, #85799, #70417 ) ) ;
#60966 = DIRECTION ( 'NONE',  ( -0.000000000000000000, -1.000000000000000000, -0.000000000000000000 ) ) ;
#60967 = DIRECTION ( 'NONE',  ( -0.000000000000000000, 1.000000000000000000, -0.000000000000000000 ) ) ;
#60968 = DIRECTION ( 'NONE',  ( 0.000000000000000000, 0.000000000000000000, -1.000000000000000000 ) ) ;
#60969 = CARTESIAN_POINT ( 'NONE',  ( -12.09999999999999609, 2.500000000000000000, 0.7928203230275536750 ) ) ;
#60970 = AXIS2_PLACEMENT_3D ( 'NONE', #121032, #43145, #122972 ) ;
#60971 = EDGE_CURVE ( 'NONE', #64242, #98726, #110124, .T. ) ;
#60972 = EDGE_CURVE ( 'NONE', #32336, #49835, #84958, .T. ) ;
#60973 = DIRECTION ( 'NONE',  ( 0.000000000000000000, 0.000000000000000000, 1.000000000000000000 ) ) ;
#60974 = CONICAL_SURFACE ( 'NONE', #4508, 0.09999999999999982514, 0.003490658503988666988 ) ;
#60975 = ORIENTED_EDGE ( 'NONE', *, *, #64067, .F. ) ;
#60976 = CARTESIAN_POINT ( 'NONE',  ( 32.28091694169009429, 1.401435235935458268, -4.680151435985021813 ) ) ;
#60977 = PLANE ( 'NONE',  #49858 ) ;
#60978 = EDGE_CURVE ( 'NONE', #62648, #123389, #18053, .T. ) ;
#60979 = FACE_OUTER_BOUND ( 'NONE', #57377, .T. ) ;
#60980 = AXIS2_PLACEMENT_3D ( 'NONE', #35712, #25224, #65140 ) ;
#60982 = CARTESIAN_POINT ( 'NONE',  ( -4.800000000000022915, 2.500000000000000000, 3.883716857408420431 ) ) ;
#60981 = AXIS2_PLACEMENT_3D ( 'NONE', #4151, #25099, #103679 ) ;
#60983 = VERTEX_POINT ( 'NONE', #60403 ) ;
#60984 = AXIS2_PLACEMENT_3D ( 'NONE', #66435, #95903, #124069 ) ;
#60985 = VERTEX_POINT ( 'NONE', #51223 ) ;
#60986 = DIRECTION ( 'NONE',  ( 0.000000000000000000, 0.000000000000000000, 1.000000000000000000 ) ) ;
#60987 = DIRECTION ( 'NONE',  ( -4.274815082592931898E-19, -0.9999939076577903929, -0.003490651415223739937 ) ) ;
#60988 = AXIS2_PLACEMENT_3D ( 'NONE', #117469, #129291, #119424 ) ;
#60989 = LINE ( 'NONE', #22378, #28893 ) ;
#60990 = EDGE_LOOP ( 'NONE', ( #109978, #30944, #110629, #40931 ) ) ;
#60991 = PLANE ( 'NONE',  #107511 ) ;
#60992 = DIRECTION ( 'NONE',  ( 0.000000000000000000, -0.000000000000000000, 1.000000000000000000 ) ) ;
#60993 = AXIS2_PLACEMENT_3D ( 'NONE', #62953, #31569, #81940 ) ;
#60994 = AXIS2_PLACEMENT_3D ( 'NONE', #90710, #59343, #50788 ) ;
#60995 = ORIENTED_EDGE ( 'NONE', *, *, #23953, .T. ) ;
#60996 = DIRECTION ( 'NONE',  ( -0.000000000000000000, -1.000000000000000000, -0.000000000000000000 ) ) ;
#60997 = EDGE_LOOP ( 'NONE', ( #7362, #52371 ) ) ;
#60998 = DIRECTION ( 'NONE',  ( 0.000000000000000000, 1.000000000000000000, 0.000000000000000000 ) ) ;
#60999 = ORIENTED_EDGE ( 'NONE', *, *, #119490, .T. ) ;
#61000 = ORIENTED_EDGE ( 'NONE', *, *, #38145, .F. ) ;
#61001 = CARTESIAN_POINT ( 'NONE',  ( 5.849999999999931255, 12.50000000000000000, 2.857883832488649301 ) ) ;
#61002 = CARTESIAN_POINT ( 'NONE',  ( -0.8500000000000382805, 12.50000000000000000, -5.867463478539787225 ) ) ;
#61003 = ORIENTED_EDGE ( 'NONE', *, *, #60365, .T. ) ;
#61004 = EDGE_LOOP ( 'NONE', ( #11029, #82921, #27573, #123773 ) ) ;
#61005 = CARTESIAN_POINT ( 'NONE',  ( -8.100000000000010303, 12.50000000000000000, 3.983716857408420964 ) ) ;
#61006 = CARTESIAN_POINT ( 'NONE',  ( 1.449999999999951328, 2.500000000000000000, -1.818653347947326138 ) ) ;
#61007 = ORIENTED_EDGE ( 'NONE', *, *, #21054, .F. ) ;
#61008 = DIRECTION ( 'NONE',  ( 0.000000000000000000, 0.000000000000000000, 1.000000000000000000 ) ) ;
#61009 = CARTESIAN_POINT ( 'NONE',  ( 185.8177083336747160, 4.367472073101515306, 7.564683531250000925 ) ) ;
#61010 = EDGE_CURVE ( 'NONE', #124302, #43675, #112062, .T. ) ;
#61011 = DIRECTION ( 'NONE',  ( -0.000000000000000000, 1.000000000000000000, -0.000000000000000000 ) ) ;
#61012 = AXIS2_PLACEMENT_3D ( 'NONE', #117152, #107357, #57626 ) ;
#61013 = DIRECTION ( 'NONE',  ( -0.000000000000000000, -1.000000000000000000, -0.000000000000000000 ) ) ;
#61014 = FACE_OUTER_BOUND ( 'NONE', #38553, .T. ) ;
#61015 = AXIS2_PLACEMENT_3D ( 'NONE', #89443, #20071, #108429 ) ;
#61016 = AXIS2_PLACEMENT_3D ( 'NONE', #52553, #80086, #122590 ) ;
#61017 = CARTESIAN_POINT ( 'NONE',  ( -6.050000000000020250, 12.50000000000000000, -6.906693963081115939 ) ) ;
#61018 = DIRECTION ( 'NONE',  ( -0.000000000000000000, 1.000000000000000000, -0.000000000000000000 ) ) ;
#61019 = CONICAL_SURFACE ( 'NONE', #67344, 0.1000000000000002554, 0.003490658503988666988 ) ;
#61020 = ORIENTED_EDGE ( 'NONE', *, *, #110402, .F. ) ;
#61022 = EDGE_LOOP ( 'NONE', ( #82178, #56291 ) ) ;
#61021 = CIRCLE ( 'NONE', #121661, 0.1000000000000002554 ) ;
#61023 = CARTESIAN_POINT ( 'NONE',  ( -10.85000000000000142, 12.50000000000000000, -2.099970236277060476 ) ) ;
#61024 = EDGE_LOOP ( 'NONE', ( #123188, #94821 ) ) ;
#61025 = LINE ( 'NONE', #49948, #18303 ) ;
#61026 = CARTESIAN_POINT ( 'NONE',  ( 15.59999999999988951, 2.500000000000000000, -0.2464101615137783419 ) ) ;
#61027 = AXIS2_PLACEMENT_3D ( 'NONE', #91961, #50750, #42893 ) ;
#61028 = CARTESIAN_POINT ( 'NONE',  ( 5.599999999999931255, 12.50000000000000000, 4.676537180435972552 ) ) ;
#61030 = VERTEX_POINT ( 'NONE', #11270 ) ;
#61029 = ORIENTED_EDGE ( 'NONE', *, *, #22219, .F. ) ;
#61031 = FACE_BOUND ( 'NONE', #42886, .T. ) ;
#61032 = ORIENTED_EDGE ( 'NONE', *, *, #117850, .T. ) ;
#61033 = DIRECTION ( 'NONE',  ( -0.000000000000000000, -1.000000000000000000, -0.000000000000000000 ) ) ;
#61034 = CARTESIAN_POINT ( 'NONE',  ( 187.5000000000000000, 1.065442715258197248E-15, -8.699999999999999289 ) ) ;
#61035 = VECTOR ( 'NONE', #105122, 1000.000000000000000 ) ;
#61036 = DIRECTION ( 'NONE',  ( -0.000000000000000000, 1.000000000000000000, -0.000000000000000000 ) ) ;
#61037 = DIRECTION ( 'NONE',  ( 0.000000000000000000, 1.000000000000000000, 0.000000000000000000 ) ) ;
#61038 = DIRECTION ( 'NONE',  ( 0.000000000000000000, -0.000000000000000000, 1.000000000000000000 ) ) ;
#61039 = DIRECTION ( 'NONE',  ( 0.000000000000000000, 1.000000000000000000, 0.000000000000000000 ) ) ;
#61040 = DIRECTION ( 'NONE',  ( 0.000000000000000000, 0.000000000000000000, 1.000000000000000000 ) ) ;
#61041 = DIRECTION ( 'NONE',  ( -0.000000000000000000, -1.000000000000000000, -0.000000000000000000 ) ) ;
#61042 = DIRECTION ( 'NONE',  ( 0.000000000000000000, -0.000000000000000000, 1.000000000000000000 ) ) ;
#61043 = DIRECTION ( 'NONE',  ( 0.000000000000000000, 1.000000000000000000, 0.000000000000000000 ) ) ;
#61044 = CARTESIAN_POINT ( 'NONE',  ( -10.85000000000000142, 2.500000000000000000, 6.495190528383297135 ) ) ;
#61045 = VERTEX_POINT ( 'NONE', #13189 ) ;
#61046 = EDGE_LOOP ( 'NONE', ( #4719, #105219, #29637, #8248 ) ) ;
#61047 = ORIENTED_EDGE ( 'NONE', *, *, #90134, .T. ) ;
#61048 = ORIENTED_EDGE ( 'NONE', *, *, #51155, .F. ) ;
#61049 = DIRECTION ( 'NONE',  ( -0.000000000000000000, -1.000000000000000000, -0.000000000000000000 ) ) ;
#61050 = DIRECTION ( 'NONE',  ( 0.000000000000000000, 1.000000000000000000, 0.000000000000000000 ) ) ;
#61052 = VERTEX_POINT ( 'NONE', #61017 ) ;
#61051 = ORIENTED_EDGE ( 'NONE', *, *, #71100, .F. ) ;
#61053 = ORIENTED_EDGE ( 'NONE', *, *, #122145, .T. ) ;
#61054 = DIRECTION ( 'NONE',  ( 0.000000000000000000, 0.000000000000000000, 1.000000000000000000 ) ) ;
#61055 = VECTOR ( 'NONE', #20717, 1000.000000000000000 ) ;
#61056 = AXIS2_PLACEMENT_3D ( 'NONE', #77363, #14554, #55147 ) ;
#61057 = EDGE_CURVE ( 'NONE', #52824, #29223, #89832, .T. ) ;
#61058 = LINE ( 'NONE', #9394, #57196 ) ;
#61059 = DIRECTION ( 'NONE',  ( -4.274815082592931898E-19, -0.9999939076577903929, -0.003490651415223739937 ) ) ;
#61060 = FACE_OUTER_BOUND ( 'NONE', #85956, .T. ) ;
#61061 = DIRECTION ( 'NONE',  ( 0.000000000000000000, -0.9999939076577903929, 0.003490651415223739937 ) ) ;
#61062 = DIRECTION ( 'NONE',  ( 0.000000000000000000, 0.000000000000000000, -1.000000000000000000 ) ) ;
#61063 = LINE ( 'NONE', #102291, #49624 ) ;
#61064 = EDGE_CURVE ( 'NONE', #73869, #58451, #30607, .T. ) ;
#61065 = VERTEX_POINT ( 'NONE', #21751 ) ;
#61066 = AXIS2_PLACEMENT_3D ( 'NONE', #3675, #71124, #41051 ) ;
#61067 = EDGE_CURVE ( 'NONE', #37903, #1292, #7590, .T. ) ;
#61068 = VECTOR ( 'NONE', #50775, 1000.000000000000000 ) ;
#61069 = CARTESIAN_POINT ( 'NONE',  ( 5.199999999999937117, 12.50000000000000000, -4.611443907251940644 ) ) ;
#61070 = EDGE_LOOP ( 'NONE', ( #70572, #98464, #83721, #48150 ) ) ;
#61071 = CIRCLE ( 'NONE', #121701, 0.06509327318403745899 ) ;
#61072 = ORIENTED_EDGE ( 'NONE', *, *, #90042, .F. ) ;
#61073 = CIRCLE ( 'NONE', #59020, 0.06509327318403745899 ) ;
#61074 = ORIENTED_EDGE ( 'NONE', *, *, #1850, .F. ) ;
#61075 = EDGE_CURVE ( 'NONE', #30951, #110642, #61685, .T. ) ;
#61077 = ADVANCED_FACE ( 'NONE', ( #40102 ), #15991, .T. ) ;
#61076 = CARTESIAN_POINT ( 'NONE',  ( -7.300000000000016698, 12.50000000000000000, -0.4115034346978157509 ) ) ;
#61079 = ORIENTED_EDGE ( 'NONE', *, *, #15550, .T. ) ;
#61078 = EDGE_CURVE ( 'NONE', #101182, #48101, #42702, .T. ) ;
#61080 = ORIENTED_EDGE ( 'NONE', *, *, #78394, .T. ) ;
#61081 = ADVANCED_FACE ( 'NONE', ( #92407 ), #21091, .T. ) ;
#61083 = VERTEX_POINT ( 'NONE', #90464 ) ;
#61082 = EDGE_CURVE ( 'NONE', #15541, #126358, #82611, .T. ) ;
#61084 = AXIS2_PLACEMENT_3D ( 'NONE', #75950, #76609, #87704 ) ;
#61085 = CARTESIAN_POINT ( 'NONE',  ( -5.850000000000018296, 2.500000000000000000, 5.802370205355744659 ) ) ;
#61086 = SURFACE_STYLE_USAGE ( .BOTH. , #63018 ) ;
#61087 = DIRECTION ( 'NONE',  ( -0.000000000000000000, 1.000000000000000000, -0.000000000000000000 ) ) ;
#61088 = FACE_OUTER_BOUND ( 'NONE', #30101, .T. ) ;
#61089 = CIRCLE ( 'NONE', #40168, 0.06509327318403745899 ) ;
#61090 = CARTESIAN_POINT ( 'NONE',  ( -4.600000000000024514, 2.500000000000000000, 3.737306695894644371 ) ) ;
#61091 = CARTESIAN_POINT ( 'NONE',  ( -8.750000000000005329, 2.500000000000000000, 5.702370205355745014 ) ) ;
#61092 = ADVANCED_FACE ( 'NONE', ( #72142 ), #105805, .T. ) ;
#61093 = AXIS2_PLACEMENT_3D ( 'NONE', #119131, #20283, #49117 ) ;
#61094 = DIRECTION ( 'NONE',  ( 0.000000000000000000, 0.000000000000000000, 1.000000000000000000 ) ) ;
#61095 = VERTEX_POINT ( 'NONE', #12551 ) ;
#61096 = CARTESIAN_POINT ( 'NONE',  ( 9.399999999999915090, 12.50000000000000000, 4.676537180435972552 ) ) ;
#61097 = EDGE_LOOP ( 'NONE', ( #80556, #8404, #117119, #89625, #56538 ) ) ;
#61098 = CARTESIAN_POINT ( 'NONE',  ( 7.899999999999924860, 12.50000000000000000, 3.702399969078682407 ) ) ;
#61099 = DIRECTION ( 'NONE',  ( 0.000000000000000000, 0.000000000000000000, 1.000000000000000000 ) ) ;
#61100 = ORIENTED_EDGE ( 'NONE', *, *, #58085, .F. ) ;
#61101 = CARTESIAN_POINT ( 'NONE',  ( 5.599999999999933031, 12.50000000000000000, 0.3464101615137735735 ) ) ;
#61102 = LINE ( 'NONE', #50017, #118904 ) ;
#61103 = ORIENTED_EDGE ( 'NONE', *, *, #111890, .T. ) ;
#61104 = CARTESIAN_POINT ( 'NONE',  ( 9.999999999999952038, 12.50000000000000000, 0.06509327318403515528 ) ) ;
#61105 = ORIENTED_EDGE ( 'NONE', *, *, #55192, .F. ) ;
#61106 = ORIENTED_EDGE ( 'NONE', *, *, #67577, .T. ) ;
#61107 = DIRECTION ( 'NONE',  ( 0.000000000000000000, 0.000000000000000000, 1.000000000000000000 ) ) ;
#61108 = CARTESIAN_POINT ( 'NONE',  ( 3.949999999999942446, 2.500000000000000000, -6.741600689897078169 ) ) ;
#61109 = CARTESIAN_POINT ( 'NONE',  ( -11.24999999999996270, 2.500000000000000000, 2.265063509461097357 ) ) ;
#61110 = CARTESIAN_POINT ( 'NONE',  ( -2.300000000000033573, 2.500000000000000000, 4.776537180435972196 ) ) ;
#61111 = FACE_OUTER_BOUND ( 'NONE', #11638, .T. ) ;
#61112 = ORIENTED_EDGE ( 'NONE', *, *, #18717, .F. ) ;
#61113 = DIRECTION ( 'NONE',  ( -0.000000000000000000, 1.000000000000000000, -0.000000000000000000 ) ) ;
#61114 = VECTOR ( 'NONE', #127983, 1000.000000000000000 ) ;
#61115 = CIRCLE ( 'NONE', #50652, 0.06509327318403745899 ) ;
#61116 = AXIS2_PLACEMENT_3D ( 'NONE', #41311, #30847, #30204 ) ;
#61117 = EDGE_CURVE ( 'NONE', #109003, #79439, #118409, .T. ) ;
#61118 = EDGE_CURVE ( 'NONE', #1292, #37903, #26396, .T. ) ;
#61119 = ORIENTED_EDGE ( 'NONE', *, *, #75003, .F. ) ;
#61120 = DIRECTION ( 'NONE',  ( 0.000000000000000000, -0.000000000000000000, 1.000000000000000000 ) ) ;
#61121 = LINE ( 'NONE', #69000, #70998 ) ;
#61122 = AXIS2_PLACEMENT_3D ( 'NONE', #71370, #1996, #21653 ) ;
#61123 = AXIS2_PLACEMENT_3D ( 'NONE', #4419, #63379, #81093 ) ;
#61124 = EDGE_CURVE ( 'NONE', #110722, #2868, #89086, .T. ) ;
#61125 = AXIS2_PLACEMENT_3D ( 'NONE', #102125, #113881, #94228 ) ;
#61126 = AXIS2_PLACEMENT_3D ( 'NONE', #106918, #17234, #89863 ) ;
#61127 = AXIS2_PLACEMENT_3D ( 'NONE', #30021, #87623, #120325 ) ;
#61128 = CARTESIAN_POINT ( 'NONE',  ( 186.7135416670080872, 4.367472073101518859, -7.564683531249999149 ) ) ;
#61129 = CYLINDRICAL_SURFACE ( 'NONE', #19629, 7.699999999999999289 ) ;
#61130 = DIRECTION ( 'NONE',  ( 0.000000000000000000, 0.000000000000000000, 1.000000000000000000 ) ) ;
#61131 = ADVANCED_FACE ( 'NONE', ( #113336 ), #9657, .T. ) ;
#61132 = FACE_OUTER_BOUND ( 'NONE', #21094, .T. ) ;
#61133 = DIRECTION ( 'NONE',  ( -0.000000000000000000, -1.000000000000000000, -0.000000000000000000 ) ) ;
#61134 = ORIENTED_EDGE ( 'NONE', *, *, #26180, .F. ) ;
#61135 = AXIS2_PLACEMENT_3D ( 'NONE', #90878, #71232, #31976 ) ;
#61136 = ADVANCED_FACE ( 'NONE', ( #114622 ), #93075, .T. ) ;
#61137 = CARTESIAN_POINT ( 'NONE',  ( -8.750000000000010658, 12.50000000000000000, 2.857883832488649301 ) ) ;
#61138 = ADVANCED_FACE ( 'NONE', ( #24319 ), #17545, .T. ) ;
#61139 = DIRECTION ( 'NONE',  ( 0.000000000000000000, 0.000000000000000000, 1.000000000000000000 ) ) ;
#61140 = DIRECTION ( 'NONE',  ( 0.000000000000000000, 1.000000000000000000, 0.000000000000000000 ) ) ;
#61141 = ORIENTED_EDGE ( 'NONE', *, *, #63441, .T. ) ;
#61142 = EDGE_CURVE ( 'NONE', #50060, #84067, #51620, .T. ) ;
#61143 = DIRECTION ( 'NONE',  ( -0.000000000000000000, 1.000000000000000000, -0.000000000000000000 ) ) ;
#61144 = AXIS2_PLACEMENT_3D ( 'NONE', #90755, #10883, #9620 ) ;
#61145 = ORIENTED_EDGE ( 'NONE', *, *, #84843, .F. ) ;
#61146 = ORIENTED_EDGE ( 'NONE', *, *, #15949, .T. ) ;
#61147 = FACE_OUTER_BOUND ( 'NONE', #91047, .T. ) ;
#61148 = ORIENTED_EDGE ( 'NONE', *, *, #75952, .F. ) ;
#61149 = CARTESIAN_POINT ( 'NONE',  ( 15.05551045035344870, -2.483581587658457490, -4.666934263344250766 ) ) ;
#61150 = DIRECTION ( 'NONE',  ( 0.000000000000000000, 0.000000000000000000, 1.000000000000000000 ) ) ;
#61151 = DIRECTION ( 'NONE',  ( 0.000000000000000000, 0.000000000000000000, 1.000000000000000000 ) ) ;
#61152 = CIRCLE ( 'NONE', #98790, 0.06509327318403745899 ) ;
#61153 = ORIENTED_EDGE ( 'NONE', *, *, #52347, .F. ) ;
#61154 = AXIS2_PLACEMENT_3D ( 'NONE', #82617, #12556, #103541 ) ;
#61155 = CARTESIAN_POINT ( 'NONE',  ( 3.949999999999942446, 12.50000000000000000, -2.511473670974877948 ) ) ;
#61156 = CARTESIAN_POINT ( 'NONE',  ( 4.349999999999936584, 2.500000000000000000, 6.248780366869520542 ) ) ;
#61157 = CARTESIAN_POINT ( 'NONE',  ( 17.46754056294898660, -1.506946016785628562, -5.249106941592948772 ) ) ;
#61158 = EDGE_CURVE ( 'NONE', #105300, #776, #73409, .T. ) ;
#61159 = CONICAL_SURFACE ( 'NONE', #84129, 0.1000000000000002554, 0.003490658503988666988 ) ;
#61160 = ORIENTED_EDGE ( 'NONE', *, *, #5116, .T. ) ;
#61161 = CONICAL_SURFACE ( 'NONE', #36029, 0.1000000000000000472, 0.003490658503988666988 ) ;
#61162 = AXIS2_PLACEMENT_3D ( 'NONE', #53169, #34833, #83274 ) ;
#61163 = ORIENTED_EDGE ( 'NONE', *, *, #82555, .T. ) ;
#61164 = ORIENTED_EDGE ( 'NONE', *, *, #60312, .T. ) ;
#61165 = CARTESIAN_POINT ( 'NONE',  ( 14.59999999999989484, 2.500000000000000000, -0.7928203230275542301 ) ) ;
#61166 = DIRECTION ( 'NONE',  ( 0.000000000000000000, -0.000000000000000000, 1.000000000000000000 ) ) ;
#61167 = DIRECTION ( 'NONE',  ( -0.000000000000000000, 1.000000000000000000, -0.000000000000000000 ) ) ;
#61168 = FACE_BOUND ( 'NONE', #109230, .T. ) ;
#61169 = VERTEX_POINT ( 'NONE', #24961 ) ;
#61170 = LINE ( 'NONE', #42179, #71841 ) ;
#61171 = LINE ( 'NONE', #101093, #75322 ) ;
#61172 = AXIS2_PLACEMENT_3D ( 'NONE', #40580, #80495, #110578 ) ;
#61173 = ORIENTED_EDGE ( 'NONE', *, *, #83091, .T. ) ;
#61174 = DIRECTION ( 'NONE',  ( -0.000000000000000000, -1.000000000000000000, -0.000000000000000000 ) ) ;
#61175 = PLANE ( 'NONE',  #45014 ) ;
#61176 = EDGE_CURVE ( 'NONE', #52125, #58340, #13940, .T. ) ;
#61177 = CONICAL_SURFACE ( 'NONE', #90402, 0.1000000000000000056, 0.003490658503988666988 ) ;
#61178 = CIRCLE ( 'NONE', #8834, 0.1000000000000002554 ) ;
#61179 = VECTOR ( 'NONE', #123043, 1000.000000000000000 ) ;
#61180 = DIRECTION ( 'NONE',  ( 0.000000000000000000, 0.000000000000000000, -1.000000000000000000 ) ) ;
#61181 = PLANE ( 'NONE',  #103126 ) ;
#61182 = DIRECTION ( 'NONE',  ( -0.000000000000000000, 1.000000000000000000, -0.000000000000000000 ) ) ;
#61183 = DIRECTION ( 'NONE',  ( 0.000000000000000000, 0.000000000000000000, -1.000000000000000000 ) ) ;
#61184 = AXIS2_PLACEMENT_3D ( 'NONE', #89513, #50882, #48302 ) ;
#61185 = CARTESIAN_POINT ( 'NONE',  ( 1.699999999999951994, 2.500000000000000000, -4.330127018922201643 ) ) ;
#61186 = ORIENTED_EDGE ( 'NONE', *, *, #65176, .F. ) ;
#61187 = CIRCLE ( 'NONE', #86296, 0.1000000000000002554 ) ;
#61188 = ORIENTED_EDGE ( 'NONE', *, *, #115199, .F. ) ;
#61189 = ORIENTED_EDGE ( 'NONE', *, *, #107948, .F. ) ;
#61190 = ORIENTED_EDGE ( 'NONE', *, *, #5371, .T. ) ;
#61191 = PLANE ( 'NONE',  #53725 ) ;
#61192 = CARTESIAN_POINT ( 'NONE',  ( 0.8499999999999545697, 2.500000000000000000, 2.757883832488649656 ) ) ;
#61193 = ORIENTED_EDGE ( 'NONE', *, *, #93707, .F. ) ;
#61194 = EDGE_CURVE ( 'NONE', #49661, #41193, #24418, .T. ) ;
#61195 = FACE_BOUND ( 'NONE', #18356, .T. ) ;
#61196 = DIRECTION ( 'NONE',  ( 0.000000000000000000, -0.000000000000000000, 1.000000000000000000 ) ) ;
#61197 = CARTESIAN_POINT ( 'NONE',  ( -4.200000000000029488, 2.500000000000000000, -4.430127018922202176 ) ) ;
#61198 = DIRECTION ( 'NONE',  ( 0.000000000000000000, 0.000000000000000000, 1.000000000000000000 ) ) ;
#61199 = DIRECTION ( 'NONE',  ( -0.000000000000000000, 1.000000000000000000, -0.000000000000000000 ) ) ;
#61200 = DIRECTION ( 'NONE',  ( -0.000000000000000000, -1.000000000000000000, -0.000000000000000000 ) ) ;
#61201 = DIRECTION ( 'NONE',  ( 0.000000000000000000, 0.000000000000000000, 1.000000000000000000 ) ) ;
#61202 = DIRECTION ( 'NONE',  ( 0.000000000000000000, -0.000000000000000000, 1.000000000000000000 ) ) ;
#61203 = DIRECTION ( 'NONE',  ( -0.000000000000000000, 1.000000000000000000, -0.000000000000000000 ) ) ;
#61204 = AXIS2_PLACEMENT_3D ( 'NONE', #53067, #63535, #15036 ) ;
#61205 = CARTESIAN_POINT ( 'NONE',  ( 7.499999999999927169, 2.500000000000000000, 3.537306695894645081 ) ) ;
#61206 = ORIENTED_EDGE ( 'NONE', *, *, #20042, .F. ) ;
#61207 = ORIENTED_EDGE ( 'NONE', *, *, #3988, .T. ) ;
#61208 = ORIENTED_EDGE ( 'NONE', *, *, #47537, .T. ) ;
#61209 = ORIENTED_EDGE ( 'NONE', *, *, #83512, .T. ) ;
#61210 = ORIENTED_EDGE ( 'NONE', *, *, #118537, .F. ) ;
#61211 = AXIS2_PLACEMENT_3D ( 'NONE', #10145, #59914, #88703 ) ;
#61212 = ORIENTED_EDGE ( 'NONE', *, *, #31412, .F. ) ;
#61213 = CONICAL_SURFACE ( 'NONE', #40288, 0.1000000000000002554, 0.003490658503988666988 ) ;
#61214 = CIRCLE ( 'NONE', #59064, 0.06509327318403745899 ) ;
#61215 = DIRECTION ( 'NONE',  ( -0.000000000000000000, -1.000000000000000000, -0.000000000000000000 ) ) ;
#61216 = VERTEX_POINT ( 'NONE', #43970 ) ;
#61217 = VECTOR ( 'NONE', #80579, 1000.000000000000000 ) ;
#61218 = AXIS2_PLACEMENT_3D ( 'NONE', #87506, #128097, #79634 ) ;
#61220 = ADVANCED_FACE ( 'NONE', ( #107225 ), #34906, .T. ) ;
#61219 = VECTOR ( 'NONE', #74319, 1000.000000000000000 ) ;
#61221 = CARTESIAN_POINT ( 'NONE',  ( 17.19804440726978001, 0.4677972980984275164, 5.492654682185340143 ) ) ;
#61222 = CARTESIAN_POINT ( 'NONE',  ( 13.91976764310545356, -2.499999999999999556, 6.779443705068508130 ) ) ;
#61223 = CARTESIAN_POINT ( 'NONE',  ( -4.150000000000027889, 2.500000000000000000, -6.395190528383301931 ) ) ;
#61224 = CARTESIAN_POINT ( 'NONE',  ( -4.200000000000025935, 12.50000000000000000, -2.385244779468109755E-15 ) ) ;
#61225 = VECTOR ( 'NONE', #55586, 1000.000000000000000 ) ;
#61226 = VECTOR ( 'NONE', #93774, 1000.000000000000000 ) ;
#61227 = AXIS2_PLACEMENT_3D ( 'NONE', #113706, #64598, #105163 ) ;
#61228 = ORIENTED_EDGE ( 'NONE', *, *, #18074, .T. ) ;
#61229 = CARTESIAN_POINT ( 'NONE',  ( 3.549999999999944755, 2.500000000000000000, -6.741600689897077281 ) ) ;
#61230 = VERTEX_POINT ( 'NONE', #87578 ) ;
#61231 = EDGE_LOOP ( 'NONE', ( #21846, #66706 ) ) ;
#61232 = DIRECTION ( 'NONE',  ( 0.000000000000000000, 0.000000000000000000, -1.000000000000000000 ) ) ;
#61233 = EDGE_CURVE ( 'NONE', #111264, #83483, #95528, .T. ) ;
#61234 = DIRECTION ( 'NONE',  ( -4.274815082592931898E-19, -0.9999939076577903929, -0.003490651415223739937 ) ) ;
#61236 = ADVANCED_FACE ( 'NONE', ( #47676 ), #83872, .T. ) ;
#61235 = DIRECTION ( 'NONE',  ( 0.000000000000000000, 0.000000000000000000, 1.000000000000000000 ) ) ;
#61237 = ADVANCED_FACE ( 'NONE', ( #28030 ), #64871, .T. ) ;
#61238 = EDGE_CURVE ( 'NONE', #88434, #51372, #107870, .T. ) ;
#61239 = ORIENTED_EDGE ( 'NONE', *, *, #98015, .F. ) ;
#61240 = ORIENTED_EDGE ( 'NONE', *, *, #101024, .F. ) ;
#61241 = AXIS2_PLACEMENT_3D ( 'NONE', #69677, #59888, #275 ) ;
#61242 = DIRECTION ( 'NONE',  ( 0.000000000000000000, -0.000000000000000000, 1.000000000000000000 ) ) ;
#61244 = EDGE_CURVE ( 'NONE', #21424, #120749, #124766, .T. ) ;
#61243 = DIRECTION ( 'NONE',  ( 0.000000000000000000, 0.000000000000000000, 1.000000000000000000 ) ) ;
#61245 = DIRECTION ( 'NONE',  ( 0.000000000000000000, -0.000000000000000000, 1.000000000000000000 ) ) ;
#61246 = DIRECTION ( 'NONE',  ( -4.274815082592931898E-19, -0.9999939076577903929, -0.003490651415223739937 ) ) ;
#61247 = VERTEX_POINT ( 'NONE', #34805 ) ;
#61248 = CARTESIAN_POINT ( 'NONE',  ( -0.4000000000000392131, 12.50000000000000000, -4.330127018922201643 ) ) ;
#61249 = ADVANCED_FACE ( 'NONE', ( #125095 ), #45363, .T. ) ;
#61251 = EDGE_LOOP ( 'NONE', ( #94209, #54483 ) ) ;
#61250 = AXIS2_PLACEMENT_3D ( 'NONE', #42810, #63712, #82721 ) ;
#61252 = CARTESIAN_POINT ( 'NONE',  ( 8.340322510150738111, -2.500000000000000444, 8.517653998215580557 ) ) ;
#61254 = ADVANCED_FACE ( 'NONE', ( #85168 ), #32843, .T. ) ;
#61253 = CONICAL_SURFACE ( 'NONE', #120028, 0.09999999999999982514, 0.003490658503988666988 ) ;
#61255 = AXIS2_PLACEMENT_3D ( 'NONE', #117180, #78603, #58313 ) ;
#61256 = EDGE_CURVE ( 'NONE', #97131, #73152, #97567, .T. ) ;
#61257 = ORIENTED_EDGE ( 'NONE', *, *, #123006, .T. ) ;
#61258 = CARTESIAN_POINT ( 'NONE',  ( -6.249999999999981348, 12.50000000000000000, 2.230156782645134950 ) ) ;
#61259 = DIRECTION ( 'NONE',  ( -0.000000000000000000, -1.000000000000000000, -0.000000000000000000 ) ) ;
#61260 = DIRECTION ( 'NONE',  ( -4.274815082592931898E-19, -0.9999939076577903929, -0.003490651415223739937 ) ) ;
#61261 = PRODUCT_DEFINITION ( 'UNKNOWN', '', #21272, #85987 ) ;
#61264 = EDGE_CURVE ( 'NONE', #119243, #122680, #9751, .T. ) ;
#61263 = AXIS2_PLACEMENT_3D ( 'NONE', #88344, #69358, #78570 ) ;
#61262 = CARTESIAN_POINT ( 'NONE',  ( 0.5999999999999621192, 2.500000000000000000, 0.2464101615137758439 ) ) ;
#61265 = VERTEX_POINT ( 'NONE', #89522 ) ;
#61266 = AXIS2_PLACEMENT_3D ( 'NONE', #72166, #2763, #104189 ) ;
#61267 = CARTESIAN_POINT ( 'NONE',  ( -2.700000000000030820, 2.500000000000000000, -3.983716857408426293 ) ) ;
#61268 = FACE_OUTER_BOUND ( 'NONE', #76274, .T. ) ;
#61269 = ORIENTED_EDGE ( 'NONE', *, *, #97287, .T. ) ;
#61270 = EDGE_LOOP ( 'NONE', ( #39692, #28617, #14360, #97503 ) ) ;
#61271 = ORIENTED_EDGE ( 'NONE', *, *, #45296, .F. ) ;
#61272 = CARTESIAN_POINT ( 'NONE',  ( 17.50000000000000000, 0.9166666666666685170, 2.864912725862981624 ) ) ;
#61273 = LINE ( 'NONE', #81550, #19822 ) ;
#61274 = CARTESIAN_POINT ( 'NONE',  ( 17.79089025268834590, 2.511997385349132195, 2.795007471442508606 ) ) ;
#61275 = AXIS2_PLACEMENT_3D ( 'NONE', #85624, #16851, #86910 ) ;
#61276 = PLANE ( 'NONE',  #126412 ) ;
#61277 = CARTESIAN_POINT ( 'NONE',  ( 8.949999999999919353, 12.50000000000000000, 2.576566944158910744 ) ) ;
#61278 = DIRECTION ( 'NONE',  ( -0.000000000000000000, -1.000000000000000000, -0.000000000000000000 ) ) ;
#61279 = CIRCLE ( 'NONE', #121909, 0.09999999999999982514 ) ;
#61280 = DIRECTION ( 'NONE',  ( -0.000000000000000000, 1.000000000000000000, -0.000000000000000000 ) ) ;
#61281 = CIRCLE ( 'NONE', #107231, 0.1000000000000000472 ) ;
#61282 = CONICAL_SURFACE ( 'NONE', #21562, 0.09999999999999982514, 0.003490658503988666988 ) ;
#61283 = FACE_OUTER_BOUND ( 'NONE', #10790, .T. ) ;
#61284 = CONICAL_SURFACE ( 'NONE', #119758, 0.1000000000000002554, 0.003490658503988666988 ) ;
#61285 = AXIS2_PLACEMENT_3D ( 'NONE', #4341, #44290, #84210 ) ;
#61286 = EDGE_LOOP ( 'NONE', ( #43546, #30511, #17916, #11409 ) ) ;
#61287 = DIRECTION ( 'NONE',  ( 1.000000000000000000, 0.000000000000000000, 0.000000000000000000 ) ) ;
#61288 = CARTESIAN_POINT ( 'NONE',  ( 8.149999999999923972, 2.500000000000000000, 1.718653347947321386 ) ) ;
#61289 = CARTESIAN_POINT ( 'NONE',  ( 7.049999999999928768, 2.500000000000000000, 6.395190528383296602 ) ) ;
#61290 = DIRECTION ( 'NONE',  ( -0.000000000000000000, 1.000000000000000000, -0.000000000000000000 ) ) ;
#61291 = ORIENTED_EDGE ( 'NONE', *, *, #105595, .T. ) ;
#61292 = DIRECTION ( 'NONE',  ( 0.000000000000000000, 0.000000000000000000, -1.000000000000000000 ) ) ;
#61293 = EDGE_CURVE ( 'NONE', #55263, #114720, #32763, .T. ) ;
#61294 = ADVANCED_FACE ( 'NONE', ( #49620 ), #57882, .T. ) ;
#61295 = DIRECTION ( 'NONE',  ( 0.000000000000000000, 1.000000000000000000, 0.000000000000000000 ) ) ;
#61297 = VERTEX_POINT ( 'NONE', #90812 ) ;
#61296 = DIRECTION ( 'NONE',  ( -4.274815082592931898E-19, -0.9999939076577903929, -0.003490651415223739937 ) ) ;
#61298 = VECTOR ( 'NONE', #9731, 1000.000000000000000 ) ;
#61299 = CONICAL_SURFACE ( 'NONE', #38315, 0.1000000000000000472, 0.003490658503988666988 ) ;
#61300 = ORIENTED_EDGE ( 'NONE', *, *, #23768, .F. ) ;
#61301 = EDGE_CURVE ( 'NONE', #5223, #103548, #28680, .T. ) ;
#61302 = FACE_OUTER_BOUND ( 'NONE', #113323, .T. ) ;
#61303 = VECTOR ( 'NONE', #52761, 1000.000000000000000 ) ;
#61304 = EDGE_LOOP ( 'NONE', ( #127072, #97691, #15809, #46540 ) ) ;
#61305 = CONICAL_SURFACE ( 'NONE', #113527, 0.1000000000000002554, 0.003490658503988666988 ) ;
#61306 = ORIENTED_EDGE ( 'NONE', *, *, #3808, .T. ) ;
#61307 = LINE ( 'NONE', #79645, #19735 ) ;
#61308 = AXIS2_PLACEMENT_3D ( 'NONE', #50929, #111775, #81660 ) ;
#61309 = CIRCLE ( 'NONE', #40387, 0.1000000000000002554 ) ;
#61310 = DIRECTION ( 'NONE',  ( 0.000000000000000000, 0.000000000000000000, -1.000000000000000000 ) ) ;
#61311 = CARTESIAN_POINT ( 'NONE',  ( 2.699999999999945555, 2.500000000000000000, 3.983716857408420076 ) ) ;
#61312 = CARTESIAN_POINT ( 'NONE',  ( -6.850000000000017408, 2.500000000000000000, -6.048780366869526581 ) ) ;
#61314 = ORIENTED_EDGE ( 'NONE', *, *, #69607, .T. ) ;
#61313 = CIRCLE ( 'NONE', #52905, 0.1000000000000000472 ) ;
#61315 = AXIS2_PLACEMENT_3D ( 'NONE', #50826, #72406, #73039 ) ;
#61316 = VECTOR ( 'NONE', #102965, 1000.000000000000000 ) ;
#61317 = DIRECTION ( 'NONE',  ( -0.000000000000000000, -1.000000000000000000, -0.000000000000000000 ) ) ;
#61318 = ORIENTED_EDGE ( 'NONE', *, *, #5064, .F. ) ;
#61319 = AXIS2_PLACEMENT_3D ( 'NONE', #125786, #4718, #123241 ) ;
#61320 = DIRECTION ( 'NONE',  ( 1.000000000000000000, -0.000000000000000000, -0.000000000000000000 ) ) ;
#61321 = DIRECTION ( 'NONE',  ( -0.000000000000000000, 1.000000000000000000, -0.000000000000000000 ) ) ;
#61322 = AXIS2_PLACEMENT_3D ( 'NONE', #59690, #80599, #70136 ) ;
#61323 = VERTEX_POINT ( 'NONE', #129481 ) ;
#61324 = ORIENTED_EDGE ( 'NONE', *, *, #69680, .T. ) ;
#61325 = EDGE_LOOP ( 'NONE', ( #43027, #11816, #76942, #4093 ) ) ;
#61326 = ORIENTED_EDGE ( 'NONE', *, *, #69105, .F. ) ;
#61327 = DIRECTION ( 'NONE',  ( 0.000000000000000000, -0.9999939076577903929, 0.003490651415223739937 ) ) ;
#61328 = CARTESIAN_POINT ( 'NONE',  ( 7.314170287632372869, 1.499999999999873657, 9.688393442221709506 ) ) ;
#61329 = DIRECTION ( 'NONE',  ( 0.000000000000000000, 0.000000000000000000, 1.000000000000000000 ) ) ;
#61330 = FACE_BOUND ( 'NONE', #102523, .T. ) ;
#61331 = DIRECTION ( 'NONE',  ( 0.000000000000000000, 0.000000000000000000, 1.000000000000000000 ) ) ;
#61332 = CARTESIAN_POINT ( 'NONE',  ( 184.6145833340161175, 6.668395609140177704, -3.849999999999998312 ) ) ;
#61333 = CARTESIAN_POINT ( 'NONE',  ( 9.799999999999915445, 2.500000000000000000, -4.576537180435977348 ) ) ;
#61334 = CARTESIAN_POINT ( 'NONE',  ( -3.550000000000031797, 2.500000000000000000, -6.148780366869526226 ) ) ;
#61335 = FACE_OUTER_BOUND ( 'NONE', #16337, .T. ) ;
#61336 = LINE ( 'NONE', #23324, #11244 ) ;
#61337 = CARTESIAN_POINT ( 'NONE',  ( -14.79999999999998295, 2.500000000000000000, -0.2464101615137760659 ) ) ;
#61338 = VECTOR ( 'NONE', #92194, 1000.000000000000000 ) ;
#61339 = CIRCLE ( 'NONE', #124025, 4.000000000000000000 ) ;
#61340 = CIRCLE ( 'NONE', #53029, 0.1000000000000000472 ) ;
#61341 = PLANE ( 'NONE',  #116304 ) ;
#61342 = VERTEX_POINT ( 'NONE', #8371 ) ;
#61343 = EDGE_LOOP ( 'NONE', ( #24414, #113397, #34387, #78163 ) ) ;
#61344 = ORIENTED_EDGE ( 'NONE', *, *, #66420, .T. ) ;
#61345 = ORIENTED_EDGE ( 'NONE', *, *, #37426, .T. ) ;
#61347 = ORIENTED_EDGE ( 'NONE', *, *, #1504, .T. ) ;
#61346 = EDGE_CURVE ( 'NONE', #75618, #64042, #1421, .T. ) ;
#61348 = CARTESIAN_POINT ( 'NONE',  ( -1.050000000000037792, 2.500000000000000000, 1.818653347947321475 ) ) ;
#61349 = DIRECTION ( 'NONE',  ( -4.274815082592931898E-19, -0.9999939076577903929, -0.003490651415223739937 ) ) ;
#61350 = ORIENTED_EDGE ( 'NONE', *, *, #99809, .T. ) ;
#61351 = ADVANCED_FACE ( 'NONE', ( #68587 ), #85049, .T. ) ;
#61352 = FACE_BOUND ( 'NONE', #8081, .T. ) ;
#61353 = CONICAL_SURFACE ( 'NONE', #111513, 0.1000000000000002554, 0.003490658503988666988 ) ;
#61354 = VECTOR ( 'NONE', #4389, 1000.000000000000000 ) ;
#61355 = DIRECTION ( 'NONE',  ( 0.000000000000000000, -0.000000000000000000, 1.000000000000000000 ) ) ;
#61356 = CONICAL_SURFACE ( 'NONE', #50887, 0.1000000000000000056, 0.003490658503988666988 ) ;
#61357 = VECTOR ( 'NONE', #124404, 1000.000000000000000 ) ;
#61358 = ORIENTED_EDGE ( 'NONE', *, *, #85480, .F. ) ;
#61359 = DIRECTION ( 'NONE',  ( 0.000000000000000000, -1.000000000000000000, 0.000000000000000000 ) ) ;
#61360 = DIRECTION ( 'NONE',  ( 0.000000000000000000, -0.000000000000000000, 1.000000000000000000 ) ) ;
#61361 = ADVANCED_FACE ( 'NONE', ( #20790 ), #105987, .T. ) ;
#61362 = CARTESIAN_POINT ( 'NONE',  ( 97.50000000000000000, 0.000000000000000000, 0.000000000000000000 ) ) ;
#61363 = DIRECTION ( 'NONE',  ( 0.000000000000000000, 1.000000000000000000, 0.000000000000000000 ) ) ;
#61364 = AXIS2_PLACEMENT_3D ( 'NONE', #63945, #54121, #44293 ) ;
#61365 = ORIENTED_EDGE ( 'NONE', *, *, #128478, .T. ) ;
#61366 = DIRECTION ( 'NONE',  ( 0.000000000000000000, 1.000000000000000000, 0.000000000000000000 ) ) ;
#61367 = CONICAL_SURFACE ( 'NONE', #2777, 0.1000000000000002554, 0.003490658503988666988 ) ;
#61368 = EDGE_LOOP ( 'NONE', ( #19531, #107987, #15825, #100583 ) ) ;
#61369 = ORIENTED_EDGE ( 'NONE', *, *, #33184, .F. ) ;
#61370 = LINE ( 'NONE', #71836, #52876 ) ;
#61371 = FACE_OUTER_BOUND ( 'NONE', #105884, .T. ) ;
#61372 = VECTOR ( 'NONE', #83419, 1000.000000000000000 ) ;
#61373 = VERTEX_POINT ( 'NONE', #479 ) ;
#61374 = CARTESIAN_POINT ( 'NONE',  ( 6.049999999999934097, 12.50000000000000000, -2.511473670974877948 ) ) ;
#61375 = CIRCLE ( 'NONE', #126209, 0.09999999999999982514 ) ;
#61376 = DIRECTION ( 'NONE',  ( 0.7336674352945127264, 0.000000000000000000, -0.6795087154616723524 ) ) ;
#61378 = EDGE_CURVE ( 'NONE', #101827, #128672, #126824, .T. ) ;
#61377 = CARTESIAN_POINT ( 'NONE',  ( -14.99999999999998224, 2.500000000000000000, -0.5928203230275518321 ) ) ;
#61379 = DIRECTION ( 'NONE',  ( 0.000000000000000000, -0.9999939076577903929, 0.003490651415223739937 ) ) ;
#61380 = CARTESIAN_POINT ( 'NONE',  ( -12.89999999999999147, 2.500000000000000000, 4.922947341949748257 ) ) ;
#61381 = VERTEX_POINT ( 'NONE', #120915 ) ;
#61382 = DIRECTION ( 'NONE',  ( -0.000000000000000000, -1.000000000000000000, -0.000000000000000000 ) ) ;
#61383 = ORIENTED_EDGE ( 'NONE', *, *, #91357, .T. ) ;
#61384 = DIRECTION ( 'NONE',  ( 0.000000000000000000, 0.000000000000000000, 1.000000000000000000 ) ) ;
#61385 = EDGE_CURVE ( 'NONE', #63267, #32002, #91318, .T. ) ;
#61386 = ORIENTED_EDGE ( 'NONE', *, *, #27105, .F. ) ;
#61387 = DIRECTION ( 'NONE',  ( -4.274815082592931898E-19, -0.9999939076577903929, -0.003490651415223739937 ) ) ;
#61388 = ORIENTED_EDGE ( 'NONE', *, *, #108109, .F. ) ;
#61389 = DIRECTION ( 'NONE',  ( -4.274815082592931898E-19, -0.9999939076577903929, -0.003490651415223739937 ) ) ;
#61390 = CARTESIAN_POINT ( 'NONE',  ( -11.84999999999999787, 12.50000000000000000, -6.841600689897074261 ) ) ;
#61391 = AXIS2_PLACEMENT_3D ( 'NONE', #50302, #128227, #88263 ) ;
#61392 = ADVANCED_FACE ( 'NONE', ( #29974 ), #105894, .T. ) ;
#61393 = PLANE ( 'NONE',  #63420 ) ;
#61394 = CONICAL_SURFACE ( 'NONE', #21684, 0.1000000000000002554, 0.003490658503988666988 ) ;
#61396 = EDGE_CURVE ( 'NONE', #36746, #117447, #101794, .T. ) ;
#61395 = DIRECTION ( 'NONE',  ( 0.000000000000000000, 1.000000000000000000, 0.000000000000000000 ) ) ;
#61397 = ADVANCED_FACE ( 'NONE', ( #20147 ), #80363, .T. ) ;
#61398 = CARTESIAN_POINT ( 'NONE',  ( 16.73738517756865107, 0.6985710795863369071, -5.899868569652234385 ) ) ;
#61399 = ADVANCED_FACE ( 'NONE', ( #10933 ), #5612, .T. ) ;
#61400 = EDGE_LOOP ( 'NONE', ( #99452, #35046 ) ) ;
#61401 = ORIENTED_EDGE ( 'NONE', *, *, #65626, .F. ) ;
#61402 = EDGE_LOOP ( 'NONE', ( #84609, #22701, #38388, #39812 ) ) ;
#61403 = FACE_OUTER_BOUND ( 'NONE', #23637, .T. ) ;
#61404 = CONICAL_SURFACE ( 'NONE', #11203, 0.09999999999999982514, 0.003490658503988666988 ) ;
#61405 = AXIS2_PLACEMENT_3D ( 'NONE', #9905, #128419, #89111 ) ;
#61406 = CONICAL_SURFACE ( 'NONE', #103151, 0.1000000000000002554, 0.003490658503988666988 ) ;
#61407 = CARTESIAN_POINT ( 'NONE',  ( -3.469446951953614189E-14, 2.500000000000000000, -0.6928203230275519209 ) ) ;
#61408 = CIRCLE ( 'NONE', #101098, 0.1000000000000000056 ) ;
#61409 = EDGE_CURVE ( 'NONE', #84837, #129184, #79076, .T. ) ;
#61411 = CARTESIAN_POINT ( 'NONE',  ( 12.89999999999990266, 2.500000000000000000, 3.637306695894644726 ) ) ;
#61410 = CONICAL_SURFACE ( 'NONE', #4932, 0.09999999999999982514, 0.003490658503988666988 ) ;
#61413 = VERTEX_POINT ( 'NONE', #50253 ) ;
#61412 = ORIENTED_EDGE ( 'NONE', *, *, #9547, .F. ) ;
#61414 = VERTEX_POINT ( 'NONE', #90145 ) ;
#61415 = EDGE_CURVE ( 'NONE', #87657, #107252, #78819, .T. ) ;
#61416 = CARTESIAN_POINT ( 'NONE',  ( -8.350000000000013856, 12.50000000000000000, -6.430097255199259010 ) ) ;
#61417 = ORIENTED_EDGE ( 'NONE', *, *, #35989, .F. ) ;
#61418 = CARTESIAN_POINT ( 'NONE',  ( -5.400000000000019895, 2.500000000000000000, 4.230127018922196669 ) ) ;
#61419 = FACE_OUTER_BOUND ( 'NONE', #126601, .T. ) ;
#61420 = CONICAL_SURFACE ( 'NONE', #25802, 0.1000000000000002554, 0.003490658503988666988 ) ;
#61421 = EDGE_CURVE ( 'NONE', #81575, #7967, #3490, .T. ) ;
#61422 = CIRCLE ( 'NONE', #128315, 0.1000000000000002554 ) ;
#61423 = ADVANCED_FACE ( 'NONE', ( #122855 ), #93375, .T. ) ;
#61424 = DIRECTION ( 'NONE',  ( 0.000000000000000000, 0.000000000000000000, 1.000000000000000000 ) ) ;
#61425 = CARTESIAN_POINT ( 'NONE',  ( 8.149999999999920419, 2.500000000000000000, 6.841600689897072485 ) ) ;
#61426 = DIRECTION ( 'NONE',  ( -0.000000000000000000, -1.000000000000000000, -0.000000000000000000 ) ) ;
#61427 = DIRECTION ( 'NONE',  ( -0.000000000000000000, -1.000000000000000000, -0.000000000000000000 ) ) ;
#61428 = LINE ( 'NONE', #84255, #78117 ) ;
#61429 = AXIS2_PLACEMENT_3D ( 'NONE', #125008, #124373, #83790 ) ;
#61431 = EDGE_CURVE ( 'NONE', #102257, #18238, #20219, .T. ) ;
#61430 = CARTESIAN_POINT ( 'NONE',  ( 7.499999999999927169, 12.50000000000000000, -5.022947341949754119 ) ) ;
#61432 = ORIENTED_EDGE ( 'NONE', *, *, #58462, .T. ) ;
#61433 = DIRECTION ( 'NONE',  ( 0.000000000000000000, -0.000000000000000000, 1.000000000000000000 ) ) ;
#61434 = CARTESIAN_POINT ( 'NONE',  ( -12.09999999999999432, 12.50000000000000000, 5.022947341949748790 ) ) ;
#61435 = ORIENTED_EDGE ( 'NONE', *, *, #6979, .F. ) ;
#61436 = ORIENTED_EDGE ( 'NONE', *, *, #90614, .T. ) ;
#61437 = CARTESIAN_POINT ( 'NONE',  ( 184.0260416670080588, -6.551208109652273848, -3.782341765625003571 ) ) ;
#61438 = DIRECTION ( 'NONE',  ( 0.000000000000000000, 1.000000000000000000, 0.000000000000000000 ) ) ;
#61439 = CARTESIAN_POINT ( 'NONE',  ( -8.350000000000013856, 12.50000000000000000, -2.165063509461101710 ) ) ;
#61440 = CIRCLE ( 'NONE', #48910, 0.06509327318403745899 ) ;
#61441 = DIRECTION ( 'NONE',  ( 0.000000000000000000, 1.000000000000000000, 0.000000000000000000 ) ) ;
#61442 = CARTESIAN_POINT ( 'NONE',  ( -15.19999999999998153, 12.50000000000000000, -0.2813168883297385570 ) ) ;
#61443 = CARTESIAN_POINT ( 'NONE',  ( -3.150000000000030109, 12.50000000000000000, 1.818653347947321475 ) ) ;
#61444 = DIRECTION ( 'NONE',  ( 0.000000000000000000, 0.000000000000000000, 1.000000000000000000 ) ) ;
#61445 = DIRECTION ( 'NONE',  ( 0.000000000000000000, 1.000000000000000000, 0.000000000000000000 ) ) ;
#61446 = AXIS2_PLACEMENT_3D ( 'NONE', #49563, #121488, #39754 ) ;
#61448 = CIRCLE ( 'NONE', #88618, 0.1000000000000002554 ) ;
#61447 = CARTESIAN_POINT ( 'NONE',  ( -11.04999999999999893, 2.500000000000000000, 6.048780366869520364 ) ) ;
#61449 = ORIENTED_EDGE ( 'NONE', *, *, #54609, .F. ) ;
#61450 = AXIS2_PLACEMENT_3D ( 'NONE', #23647, #103504, #22380 ) ;
#61451 = EDGE_LOOP ( 'NONE', ( #113823, #42038 ) ) ;
#61452 = ORIENTED_EDGE ( 'NONE', *, *, #54143, .T. ) ;
#61453 = VERTEX_POINT ( 'NONE', #93395 ) ;
#61454 = AXIS2_PLACEMENT_3D ( 'NONE', #26720, #124920, #75173 ) ;
#61455 = DIRECTION ( 'NONE',  ( 0.000000000000000000, 0.000000000000000000, -1.000000000000000000 ) ) ;
#61456 = CARTESIAN_POINT ( 'NONE',  ( -11.24999999999999822, 2.500000000000000000, 1.472243186433545459 ) ) ;
#61457 = AXIS2_PLACEMENT_3D ( 'NONE', #38415, #69131, #68490 ) ;
#61458 = ORIENTED_EDGE ( 'NONE', *, *, #99203, .T. ) ;
#61459 = FACE_OUTER_BOUND ( 'NONE', #43116, .T. ) ;
#61460 = AXIS2_PLACEMENT_3D ( 'NONE', #71763, #1716, #41034 ) ;
#61461 = EDGE_CURVE ( 'NONE', #35080, #96401, #3583, .T. ) ;
#61462 = CARTESIAN_POINT ( 'NONE',  ( 186.1562500006828031, 8.891194145520236347, 5.444286225454521982E-16 ) ) ;
#61463 = EDGE_CURVE ( 'NONE', #105776, #58192, #18244, .T. ) ;
#61464 = DIRECTION ( 'NONE',  ( -0.000000000000000000, 1.000000000000000000, -0.000000000000000000 ) ) ;
#61466 = EDGE_LOOP ( 'NONE', ( #52629, #122993, #31728, #102363 ) ) ;
#61465 = DIRECTION ( 'NONE',  ( -4.274815082592931898E-19, -0.9999939076577903929, -0.003490651415223739937 ) ) ;
#61467 = DIRECTION ( 'NONE',  ( -0.000000000000000000, -1.000000000000000000, -0.000000000000000000 ) ) ;
#61468 = CIRCLE ( 'NONE', #63514, 0.06509327318403741736 ) ;
#61469 = CARTESIAN_POINT ( 'NONE',  ( -3.750000000000027534, 12.50000000000000000, -1.472243186433550122 ) ) ;
#61470 = ORIENTED_EDGE ( 'NONE', *, *, #128910, .F. ) ;
#61471 = AXIS2_PLACEMENT_3D ( 'NONE', #49909, #110098, #28974 ) ;
#61472 = VECTOR ( 'NONE', #20540, 1000.000000000000000 ) ;
#61473 = CIRCLE ( 'NONE', #904, 0.06509327318403745899 ) ;
#61474 = VERTEX_POINT ( 'NONE', #73734 ) ;
#61475 = EDGE_LOOP ( 'NONE', ( #110809, #82839, #34104, #34752 ) ) ;
#61476 = ORIENTED_EDGE ( 'NONE', *, *, #76769, .T. ) ;
#61477 = DIRECTION ( 'NONE',  ( 0.000000000000000000, 0.000000000000000000, -1.000000000000000000 ) ) ;
#61478 = DIRECTION ( 'NONE',  ( 0.000000000000000000, 1.000000000000000000, 0.000000000000000000 ) ) ;
#61479 = CARTESIAN_POINT ( 'NONE',  ( 2.500000000000001776, -2.021986658763283096, -9.892226903609810051 ) ) ;
#61480 = AXIS2_PLACEMENT_3D ( 'NONE', #46191, #56634, #23986 ) ;
#61481 = ORIENTED_EDGE ( 'NONE', *, *, #41363, .T. ) ;
#61482 = DIRECTION ( 'NONE',  ( 0.000000000000000000, 1.000000000000000000, 0.000000000000000000 ) ) ;
#61483 = ORIENTED_EDGE ( 'NONE', *, *, #128035, .T. ) ;
#61484 = PLANE ( 'NONE',  #70526 ) ;
#61485 = FACE_OUTER_BOUND ( 'NONE', #64610, .T. ) ;
#61486 = LINE ( 'NONE', #92204, #111083 ) ;
#61487 = CARTESIAN_POINT ( 'NONE',  ( -13.09999999999999254, 2.500000000000000000, -4.676537180435975216 ) ) ;
#61488 = ORIENTED_EDGE ( 'NONE', *, *, #6494, .T. ) ;
#61489 = ORIENTED_EDGE ( 'NONE', *, *, #68445, .F. ) ;
#61490 = AXIS2_PLACEMENT_3D ( 'NONE', #92827, #3789, #101996 ) ;
#61491 = ORIENTED_EDGE ( 'NONE', *, *, #20594, .T. ) ;
#61492 = DIRECTION ( 'NONE',  ( -0.000000000000000000, -1.000000000000000000, -0.000000000000000000 ) ) ;
#61493 = CONICAL_SURFACE ( 'NONE', #63635, 0.1000000000000002554, 0.003490658503988666988 ) ;
#61494 = DIRECTION ( 'NONE',  ( -0.000000000000000000, 1.000000000000000000, -0.000000000000000000 ) ) ;
#61495 = FACE_BOUND ( 'NONE', #10551, .T. ) ;
#61496 = FACE_OUTER_BOUND ( 'NONE', #103282, .T. ) ;
#61497 = CARTESIAN_POINT ( 'NONE',  ( 13.94999999999989804, 2.500000000000000000, 1.918653347947321564 ) ) ;
#61498 = CARTESIAN_POINT ( 'NONE',  ( -2.499999999999996003, 2.500000000000000000, -4.230127018922201998 ) ) ;
#61499 = EDGE_CURVE ( 'NONE', #120419, #120803, #122717, .T. ) ;
#61500 = AXIS2_PLACEMENT_3D ( 'NONE', #76122, #47957, #56464 ) ;
#61501 = AXIS2_PLACEMENT_3D ( 'NONE', #98591, #8289, #48226 ) ;
#61502 = CONICAL_SURFACE ( 'NONE', #84471, 0.1000000000000002554, 0.003490658503988666988 ) ;
#61503 = VECTOR ( 'NONE', #12118, 1000.000000000000000 ) ;
#61504 = LINE ( 'NONE', #101415, #2411 ) ;
#61505 = CYLINDRICAL_SURFACE ( 'NONE', #4891, 2.249999999999996891 ) ;
#61506 = CARTESIAN_POINT ( 'NONE',  ( 11.24999999999994316, 2.500000000000000000, 2.265063509461097357 ) ) ;
#61507 = ORIENTED_EDGE ( 'NONE', *, *, #29573, .F. ) ;
#61509 = CARTESIAN_POINT ( 'NONE',  ( 11.24999999999990941, 12.50000000000000000, 7.253104124594885960 ) ) ;
#61508 = AXIS2_PLACEMENT_3D ( 'NONE', #69995, #2508, #41835 ) ;
#61510 = VECTOR ( 'NONE', #96961, 1000.000000000000000 ) ;
#61511 = FACE_OUTER_BOUND ( 'NONE', #43459, .T. ) ;
#61512 = ORIENTED_EDGE ( 'NONE', *, *, #104934, .F. ) ;
#61513 = EDGE_LOOP ( 'NONE', ( #113326, #4012 ) ) ;
#61514 = CIRCLE ( 'NONE', #38537, 0.09999999999999999167 ) ;
#61515 = EDGE_CURVE ( 'NONE', #8603, #79214, #21423, .T. ) ;
#61516 = DIRECTION ( 'NONE',  ( 0.000000000000000000, 0.000000000000000000, -1.000000000000000000 ) ) ;
#61518 = EDGE_CURVE ( 'NONE', #26678, #38170, #99740, .T. ) ;
#61517 = CARTESIAN_POINT ( 'NONE',  ( 6.849999999999930367, 2.500000000000000000, -6.148780366869526226 ) ) ;
#61519 = FACE_BOUND ( 'NONE', #34433, .T. ) ;
#61520 = CARTESIAN_POINT ( 'NONE',  ( 15.83209681635555022, -2.500000000000000000, -5.404881881984138658 ) ) ;
#61521 = AXIS2_PLACEMENT_3D ( 'NONE', #127871, #38888, #17911 ) ;
#61522 = ORIENTED_EDGE ( 'NONE', *, *, #77270, .F. ) ;
#61523 = DIRECTION ( 'NONE',  ( 0.000000000000000000, 0.000000000000000000, -1.000000000000000000 ) ) ;
#61524 = EDGE_CURVE ( 'NONE', #107, #5118, #64211, .T. ) ;
#61525 = DIRECTION ( 'NONE',  ( 0.000000000000000000, 0.000000000000000000, 1.000000000000000000 ) ) ;
#61527 = ORIENTED_EDGE ( 'NONE', *, *, #81185, .F. ) ;
#61526 = VECTOR ( 'NONE', #96236, 1000.000000000000000 ) ;
#61528 = CARTESIAN_POINT ( 'NONE',  ( -9.150000000000005684, 2.500000000000000000, 5.702370205355745014 ) ) ;
#61529 = DIRECTION ( 'NONE',  ( -0.000000000000000000, -1.000000000000000000, -0.000000000000000000 ) ) ;
#61530 = CARTESIAN_POINT ( 'NONE',  ( -2.500000000000032419, 2.500000000000000000, -3.737306695894649700 ) ) ;
#61531 = CARTESIAN_POINT ( 'NONE',  ( -12.09999999999999609, 12.50000000000000000, 0.7579135962115910452 ) ) ;
#61532 = CIRCLE ( 'NONE', #115802, 0.09999999999999982514 ) ;
#61533 = EDGE_LOOP ( 'NONE', ( #61193, #55933, #83905, #84857 ) ) ;
#61534 = CARTESIAN_POINT ( 'NONE',  ( -11.05000000000000249, 12.50000000000000000, -6.148780366869522673 ) ) ;
#61535 = CARTESIAN_POINT ( 'NONE',  ( 8.749999999999953815, 2.500000000000000000, -2.165063509461101710 ) ) ;
#61536 = DIRECTION ( 'NONE',  ( -0.000000000000000000, -1.000000000000000000, -0.000000000000000000 ) ) ;
#61537 = ORIENTED_EDGE ( 'NONE', *, *, #67226, .T. ) ;
#61538 = VERTEX_POINT ( 'NONE', #63285 ) ;
#61539 = FACE_OUTER_BOUND ( 'NONE', #73632, .T. ) ;
#61540 = EDGE_LOOP ( 'NONE', ( #37451, #8846 ) ) ;
#61541 = DIRECTION ( 'NONE',  ( -4.274815082592931898E-19, -0.9999939076577903929, -0.003490651415223739937 ) ) ;
#61542 = DIRECTION ( 'NONE',  ( 0.000000000000000000, 1.000000000000000000, 0.000000000000000000 ) ) ;
#61543 = AXIS2_PLACEMENT_3D ( 'NONE', #47458, #67728, #38287 ) ;
#61544 = EDGE_CURVE ( 'NONE', #26678, #50768, #112394, .T. ) ;
#61545 = CARTESIAN_POINT ( 'NONE',  ( -10.40000000000000213, 2.500000000000000000, 0.5928203230275495006 ) ) ;
#61546 = ORIENTED_EDGE ( 'NONE', *, *, #53248, .T. ) ;
#61547 = CARTESIAN_POINT ( 'NONE',  ( -0.4000000000000331624, 2.500000000000000000, 0.000000000000000000 ) ) ;
#61548 = DIRECTION ( 'NONE',  ( 0.000000000000000000, 1.000000000000000000, 0.000000000000000000 ) ) ;
#61549 = CARTESIAN_POINT ( 'NONE',  ( 2.699999999999946443, 2.500000000000000000, 0.3464101615137735735 ) ) ;
#61550 = CARTESIAN_POINT ( 'NONE',  ( -0.8500000000000386136, 12.50000000000000000, 2.922977105672686982 ) ) ;
#61551 = DIRECTION ( 'NONE',  ( -4.274815082592931898E-19, -0.9999939076577903929, -0.003490651415223739937 ) ) ;
#61552 = ADVANCED_FACE ( 'NONE', ( #103210 ), #108128, .T. ) ;
#61553 = DIRECTION ( 'NONE',  ( -0.000000000000000000, -1.000000000000000000, -0.000000000000000000 ) ) ;
#61554 = ADVANCED_FACE ( 'NONE', ( #81628 ), #92756, .T. ) ;
#61555 = ORIENTED_EDGE ( 'NONE', *, *, #112938, .T. ) ;
#61556 = ORIENTED_EDGE ( 'NONE', *, *, #23968, .T. ) ;
#61557 = FACE_OUTER_BOUND ( 'NONE', #5791, .T. ) ;
#61559 = ORIENTED_EDGE ( 'NONE', *, *, #69026, .F. ) ;
#61558 = AXIS2_PLACEMENT_3D ( 'NONE', #80650, #1423, #123146 ) ;
#61560 = CIRCLE ( 'NONE', #17705, 0.1000000000000002554 ) ;
#61561 = LINE ( 'NONE', #49813, #80697 ) ;
#61562 = EDGE_CURVE ( 'NONE', #48575, #33637, #82939, .T. ) ;
#61564 = ORIENTED_EDGE ( 'NONE', *, *, #102339, .F. ) ;
#61563 = ORIENTED_EDGE ( 'NONE', *, *, #87210, .F. ) ;
#61565 = EDGE_CURVE ( 'NONE', #2276, #12831, #87190, .T. ) ;
#61566 = EDGE_LOOP ( 'NONE', ( #38636, #85931, #112592, #29932 ) ) ;
#61567 = CIRCLE ( 'NONE', #11371, 0.1000000000000000056 ) ;
#61568 = ADVANCED_FACE ( 'NONE', ( #33820 ), #82293, .T. ) ;
#61569 = CARTESIAN_POINT ( 'NONE',  ( 5.799999999999934985, 2.500000000000000000, -4.330127018922201643 ) ) ;
#61570 = EDGE_CURVE ( 'NONE', #112245, #115252, #76743, .T. ) ;
#61571 = AXIS2_PLACEMENT_3D ( 'NONE', #9495, #39627, #107696 ) ;
#61572 = FACE_OUTER_BOUND ( 'NONE', #62522, .T. ) ;
#61573 = DIRECTION ( 'NONE',  ( 0.000000000000000000, 1.000000000000000000, 0.000000000000000000 ) ) ;
#61574 = ADVANCED_FACE ( 'NONE', ( #62011 ), #20306, .T. ) ;
#61575 = DIRECTION ( 'NONE',  ( -0.000000000000000000, -1.000000000000000000, -0.000000000000000000 ) ) ;
#61576 = FACE_OUTER_BOUND ( 'NONE', #33096, .T. ) ;
#61577 = CARTESIAN_POINT ( 'NONE',  ( 1.249999999999988454, 12.50000000000000000, 2.230156782645134950 ) ) ;
#61578 = CARTESIAN_POINT ( 'NONE',  ( 1.249999999999953815, 2.500000000000000000, -2.757883832488654097 ) ) ;
#61579 = DIRECTION ( 'NONE',  ( 0.000000000000000000, -0.9999939076577903929, 0.003490651415223739937 ) ) ;
#61581 = EDGE_CURVE ( 'NONE', #23243, #87251, #62656, .T. ) ;
#61580 = DIRECTION ( 'NONE',  ( 0.000000000000000000, -0.000000000000000000, 1.000000000000000000 ) ) ;
#61582 = ORIENTED_EDGE ( 'NONE', *, *, #27261, .T. ) ;
#61583 = CIRCLE ( 'NONE', #124262, 0.06509327318403745899 ) ;
#61584 = CIRCLE ( 'NONE', #25976, 0.06509327318403745899 ) ;
#61585 = DIRECTION ( 'NONE',  ( -0.000000000000000000, 1.000000000000000000, -0.000000000000000000 ) ) ;
#61586 = AXIS2_PLACEMENT_3D ( 'NONE', #55452, #26002, #27270 ) ;
#61587 = CIRCLE ( 'NONE', #107632, 0.1000000000000002554 ) ;
#61588 = VERTEX_POINT ( 'NONE', #87425 ) ;
#61589 = ORIENTED_EDGE ( 'NONE', *, *, #113232, .F. ) ;
#61590 = CARTESIAN_POINT ( 'NONE',  ( -10.45000000000000107, 12.50000000000000000, 2.165063509461097713 ) ) ;
#61591 = CARTESIAN_POINT ( 'NONE',  ( -2.100000000000034728, 2.500000000000000000, 4.230127018922196669 ) ) ;
#61592 = CARTESIAN_POINT ( 'NONE',  ( -6.650000000000014566, 12.50000000000000000, 5.737276932171707422 ) ) ;
#61593 = CARTESIAN_POINT ( 'NONE',  ( 186.6250000000000000, -8.891194145520236347, -1.633285867636356299E-15 ) ) ;
#61594 = CONICAL_SURFACE ( 'NONE', #124277, 0.1000000000000002554, 0.003490658503988666988 ) ;
#61596 = DIRECTION ( 'NONE',  ( 0.000000000000000000, 1.000000000000000000, 0.000000000000000000 ) ) ;
#61595 = AXIS2_PLACEMENT_3D ( 'NONE', #104390, #64456, #94558 ) ;
#61597 = DIRECTION ( 'NONE',  ( -0.000000000000000000, 1.000000000000000000, -0.000000000000000000 ) ) ;
#61598 = DIRECTION ( 'NONE',  ( 0.000000000000000000, 1.000000000000000000, 0.000000000000000000 ) ) ;
#61599 = ORIENTED_EDGE ( 'NONE', *, *, #103667, .F. ) ;
#61601 = ORIENTED_EDGE ( 'NONE', *, *, #84283, .T. ) ;
#61600 = AXIS2_PLACEMENT_3D ( 'NONE', #88272, #107289, #49042 ) ;
#61602 = AXIS2_PLACEMENT_3D ( 'NONE', #11100, #23507, #80520 ) ;
#61603 = EDGE_LOOP ( 'NONE', ( #107577, #66866, #48909, #99940 ) ) ;
#61604 = ORIENTED_EDGE ( 'NONE', *, *, #37712, .F. ) ;
#61605 = AXIS2_PLACEMENT_3D ( 'NONE', #77673, #116949, #47595 ) ;
#61606 = EDGE_LOOP ( 'NONE', ( #93779, #129125, #44927, #93451 ) ) ;
#61607 = CARTESIAN_POINT ( 'NONE',  ( 4.799999999999939426, 12.50000000000000000, -4.611443907251939756 ) ) ;
#61608 = DIRECTION ( 'NONE',  ( -0.000000000000000000, -1.000000000000000000, -0.000000000000000000 ) ) ;
#61609 = CARTESIAN_POINT ( 'NONE',  ( -12.09999999999999609, 2.500000000000000000, 4.430127018922196847 ) ) ;
#61610 = EDGE_CURVE ( 'NONE', #4240, #103155, #67114, .T. ) ;
#61611 = DIRECTION ( 'NONE',  ( -0.000000000000000000, -1.000000000000000000, -0.000000000000000000 ) ) ;
#61612 = CARTESIAN_POINT ( 'NONE',  ( 9.599999999999917932, 2.500000000000000000, -2.276824562219559311E-15 ) ) ;
#61613 = ORIENTED_EDGE ( 'NONE', *, *, #110465, .T. ) ;
#61614 = CARTESIAN_POINT ( 'NONE',  ( 0.3999999999999619971, 12.50000000000000000, -1.084202172485504434E-16 ) ) ;
#61615 = DIRECTION ( 'NONE',  ( 0.000000000000000000, 0.000000000000000000, -1.000000000000000000 ) ) ;
#61616 = CARTESIAN_POINT ( 'NONE',  ( -10.85000000000000142, 12.50000000000000000, -6.495190528383298911 ) ) ;
#61617 = CARTESIAN_POINT ( 'NONE',  ( -9.600000000000008527, 2.500000000000000000, -3.537306695894645969 ) ) ;
#61619 = ADVANCED_FACE ( 'NONE', ( #116876 ), #28728, .T. ) ;
#61618 = DIRECTION ( 'NONE',  ( 0.000000000000000000, 1.000000000000000000, 0.000000000000000000 ) ) ;
#61620 = ORIENTED_EDGE ( 'NONE', *, *, #112026, .F. ) ;
#61621 = VERTEX_POINT ( 'NONE', #74395 ) ;
#61622 = VERTEX_POINT ( 'NONE', #105789 ) ;
#61623 = CARTESIAN_POINT ( 'NONE',  ( -6.249999999999981348, 2.500000000000000000, 2.065063509461097624 ) ) ;
#61624 = VERTEX_POINT ( 'NONE', #114318 ) ;
#61625 = AXIS2_PLACEMENT_3D ( 'NONE', #5636, #126060, #64565 ) ;
#61626 = CARTESIAN_POINT ( 'NONE',  ( 10.79999999999991367, 12.50000000000000000, 0.06509327318403504425 ) ) ;
#61627 = FACE_OUTER_BOUND ( 'NONE', #24055, .T. ) ;
#61628 = CONICAL_SURFACE ( 'NONE', #5160, 0.1000000000000000472, 0.003490658503988666988 ) ;
#61629 = ORIENTED_EDGE ( 'NONE', *, *, #59221, .T. ) ;
#61630 = FACE_OUTER_BOUND ( 'NONE', #44893, .T. ) ;
#61631 = DIRECTION ( 'NONE',  ( 0.000000000000000000, -0.9999939076577903929, 0.003490651415223739937 ) ) ;
#61632 = DIRECTION ( 'NONE',  ( 0.000000000000000000, 1.000000000000000000, 0.000000000000000000 ) ) ;
#61633 = CARTESIAN_POINT ( 'NONE',  ( -6.650000000000015454, 12.50000000000000000, 7.188010851410848723 ) ) ;
#61634 = AXIS2_PLACEMENT_3D ( 'NONE', #89157, #101560, #128460 ) ;
#61635 = DIRECTION ( 'NONE',  ( 0.000000000000000000, 0.000000000000000000, -1.000000000000000000 ) ) ;
#61636 = CONICAL_SURFACE ( 'NONE', #70233, 0.09999999999999982514, 0.003490658503988666988 ) ;
#61637 = ORIENTED_EDGE ( 'NONE', *, *, #27504, .T. ) ;
#61638 = ORIENTED_EDGE ( 'NONE', *, *, #55778, .F. ) ;
#61639 = DIRECTION ( 'NONE',  ( -4.274815082592931898E-19, -0.9999939076577903929, -0.003490651415223739937 ) ) ;
#61640 = CARTESIAN_POINT ( 'NONE',  ( -9.999999999999969802, 12.50000000000000000, 0.06509327318403515528 ) ) ;
#61641 = DIRECTION ( 'NONE',  ( 0.000000000000000000, 1.000000000000000000, 0.000000000000000000 ) ) ;
#61642 = DIRECTION ( 'NONE',  ( -0.000000000000000000, 1.000000000000000000, -0.000000000000000000 ) ) ;
#61643 = EDGE_CURVE ( 'NONE', #35451, #3120, #65195, .T. ) ;
#61644 = ORIENTED_EDGE ( 'NONE', *, *, #96079, .F. ) ;
#61645 = CONICAL_SURFACE ( 'NONE', #15642, 0.1000000000000002554, 0.003490658503988666988 ) ;
#61646 = CONICAL_SURFACE ( 'NONE', #101359, 0.1000000000000002554, 0.003490658503988666988 ) ;
#61648 = EDGE_LOOP ( 'NONE', ( #51929, #80594, #74744, #113253 ) ) ;
#61647 = CIRCLE ( 'NONE', #74167, 0.1000000000000002554 ) ;
#61649 = FACE_OUTER_BOUND ( 'NONE', #37428, .T. ) ;
#61650 = FACE_OUTER_BOUND ( 'NONE', #129446, .T. ) ;
#61651 = DIRECTION ( 'NONE',  ( 0.000000000000000000, -0.9999939076577903929, 0.003490651415223739937 ) ) ;
#61652 = AXIS2_PLACEMENT_3D ( 'NONE', #59257, #37674, #99169 ) ;
#61653 = DIRECTION ( 'NONE',  ( -4.274815082592931898E-19, -0.9999939076577903929, -0.003490651415223739937 ) ) ;
#61654 = ORIENTED_EDGE ( 'NONE', *, *, #34196, .F. ) ;
#61655 = EDGE_CURVE ( 'NONE', #45027, #180, #66271, .T. ) ;
#61656 = DIRECTION ( 'NONE',  ( -0.000000000000000000, -1.000000000000000000, -0.000000000000000000 ) ) ;
#61657 = DIRECTION ( 'NONE',  ( 0.000000000000000000, 1.000000000000000000, 0.000000000000000000 ) ) ;
#61658 = EDGE_LOOP ( 'NONE', ( #72019, #62014, #125400, #111057 ) ) ;
#61659 = EDGE_CURVE ( 'NONE', #90431, #76525, #101876, .T. ) ;
#61660 = FACE_OUTER_BOUND ( 'NONE', #127779, .T. ) ;
#61661 = ADVANCED_FACE ( 'NONE', ( #17384 ), #105133, .T. ) ;
#61662 = EDGE_LOOP ( 'NONE', ( #24241, #41409 ) ) ;
#61663 = CARTESIAN_POINT ( 'NONE',  ( 4.349999999999936584, 2.500000000000000000, 6.048780366869520364 ) ) ;
#61664 = ORIENTED_EDGE ( 'NONE', *, *, #118697, .T. ) ;
#61665 = CIRCLE ( 'NONE', #40748, 0.06509327318403745899 ) ;
#61666 = ORIENTED_EDGE ( 'NONE', *, *, #87428, .T. ) ;
#61667 = LINE ( 'NONE', #11903, #109181 ) ;
#61668 = CARTESIAN_POINT ( 'NONE',  ( -14.59999999999998366, 2.500000000000000000, -0.6928203230275520319 ) ) ;
#61669 = EDGE_CURVE ( 'NONE', #28566, #57456, #16733, .T. ) ;
#61670 = CIRCLE ( 'NONE', #38603, 0.09999999999999982514 ) ;
#61671 = AXIS2_PLACEMENT_3D ( 'NONE', #107737, #116256, #108377 ) ;
#61672 = ORIENTED_EDGE ( 'NONE', *, *, #11201, .F. ) ;
#61673 = ORIENTED_EDGE ( 'NONE', *, *, #116067, .T. ) ;
#61674 = EDGE_CURVE ( 'NONE', #40266, #122166, #97253, .T. ) ;
#61675 = CARTESIAN_POINT ( 'NONE',  ( 9.549999999999915445, 2.500000000000000000, 6.495190528383297135 ) ) ;
#61676 = DIRECTION ( 'NONE',  ( 0.000000000000000000, 0.000000000000000000, 1.000000000000000000 ) ) ;
#61677 = CARTESIAN_POINT ( 'NONE',  ( -2.300000000000032685, 2.500000000000000000, -0.4464101615137783252 ) ) ;
#61678 = CARTESIAN_POINT ( 'NONE',  ( 185.8593750003413732, 0.000000000000000000, 7.564683531250000925 ) ) ;
#61679 = CONICAL_SURFACE ( 'NONE', #53269, 0.09999999999999982514, 0.003490658503988666988 ) ;
#61680 = CIRCLE ( 'NONE', #124370, 0.06509327318403745899 ) ;
#61681 = CARTESIAN_POINT ( 'NONE',  ( 14.54999999999989591, 12.50000000000000000, 2.165063509461097713 ) ) ;
#61682 = LINE ( 'NONE', #51856, #126737 ) ;
#61683 = FACE_OUTER_BOUND ( 'NONE', #23978, .T. ) ;
#61684 = CONICAL_SURFACE ( 'NONE', #3191, 0.1000000000000002554, 0.003490658503988666988 ) ;
#61685 = LINE ( 'NONE', #71477, #64037 ) ;
#61686 = DIRECTION ( 'NONE',  ( 0.000000000000000000, 1.000000000000000000, 0.000000000000000000 ) ) ;
#61687 = CIRCLE ( 'NONE', #53283, 0.06509327318403745899 ) ;
#61688 = AXIS2_PLACEMENT_3D ( 'NONE', #97408, #48312, #18196 ) ;
#61689 = EDGE_LOOP ( 'NONE', ( #81297, #74842, #44199, #103682 ) ) ;
#61690 = ORIENTED_EDGE ( 'NONE', *, *, #72061, .T. ) ;
#61691 = PLANE ( 'NONE',  #69547 ) ;
#61692 = EDGE_LOOP ( 'NONE', ( #117216, #94420 ) ) ;
#61693 = CARTESIAN_POINT ( 'NONE',  ( -4.250072516143177381E-14, 2.500000000000000000, -3.637306695894650055 ) ) ;
#61694 = CARTESIAN_POINT ( 'NONE',  ( 6.649999999999930189, 12.50000000000000000, -2.857883832488653741 ) ) ;
#61695 = VECTOR ( 'NONE', #88463, 1000.000000000000000 ) ;
#61696 = DIRECTION ( 'NONE',  ( 0.000000000000000000, 0.000000000000000000, -1.000000000000000000 ) ) ;
#61698 = ORIENTED_EDGE ( 'NONE', *, *, #16732, .F. ) ;
#61697 = VERTEX_POINT ( 'NONE', #47522 ) ;
#61699 = FACE_BOUND ( 'NONE', #79898, .T. ) ;
#61700 = ORIENTED_EDGE ( 'NONE', *, *, #30550, .F. ) ;
#61701 = DIRECTION ( 'NONE',  ( -0.000000000000000000, 1.000000000000000000, -0.000000000000000000 ) ) ;
#61702 = DIRECTION ( 'NONE',  ( 0.000000000000000000, 0.000000000000000000, 1.000000000000000000 ) ) ;
#61703 = DIRECTION ( 'NONE',  ( 0.000000000000000000, 1.000000000000000000, 0.000000000000000000 ) ) ;
#61704 = CARTESIAN_POINT ( 'NONE',  ( 2.299999999999947864, 2.500000000000000000, 4.083716857408421497 ) ) ;
#61705 = LINE ( 'NONE', #101624, #70236 ) ;
#61706 = DIRECTION ( 'NONE',  ( -0.000000000000000000, 1.000000000000000000, -0.000000000000000000 ) ) ;
#61707 = DIRECTION ( 'NONE',  ( 0.000000000000000000, 1.000000000000000000, 0.000000000000000000 ) ) ;
#61708 = DIRECTION ( 'NONE',  ( 0.000000000000000000, 1.000000000000000000, 0.000000000000000000 ) ) ;
#61709 = FACE_OUTER_BOUND ( 'NONE', #54475, .T. ) ;
#61710 = CARTESIAN_POINT ( 'NONE',  ( 10.64999999999991331, 12.50000000000000000, 6.841600689897072485 ) ) ;
#61711 = AXIS2_PLACEMENT_3D ( 'NONE', #61694, #93084, #54422 ) ;
#61712 = DIRECTION ( 'NONE',  ( 0.000000000000000000, 1.000000000000000000, 0.000000000000000000 ) ) ;
#61713 = ADVANCED_FACE ( 'NONE', ( #127370 ), #55899, .T. ) ;
#61714 = ORIENTED_EDGE ( 'NONE', *, *, #5126, .T. ) ;
#61715 = ORIENTED_EDGE ( 'NONE', *, *, #93158, .T. ) ;
#61716 = ORIENTED_EDGE ( 'NONE', *, *, #112615, .F. ) ;
#61717 = ORIENTED_EDGE ( 'NONE', *, *, #93828, .F. ) ;
#61718 = CARTESIAN_POINT ( 'NONE',  ( 11.44999999999990692, 12.50000000000000000, -6.841600689897078702 ) ) ;
#61719 = EDGE_CURVE ( 'NONE', #1993, #54526, #5638, .T. ) ;
#61720 = CARTESIAN_POINT ( 'NONE',  ( -9.600000000000008527, 2.500000000000000000, 4.330127018922196314 ) ) ;
#61721 = EDGE_CURVE ( 'NONE', #13533, #40017, #118589, .T. ) ;
#61723 = ORIENTED_EDGE ( 'NONE', *, *, #50162, .T. ) ;
#61722 = ORIENTED_EDGE ( 'NONE', *, *, #95399, .F. ) ;
#61724 = ORIENTED_EDGE ( 'NONE', *, *, #61659, .T. ) ;
#61725 = EDGE_CURVE ( 'NONE', #118121, #89261, #49666, .T. ) ;
#61726 = DIRECTION ( 'NONE',  ( 0.000000000000000000, 1.000000000000000000, 0.000000000000000000 ) ) ;
#61727 = AXIS2_PLACEMENT_3D ( 'NONE', #30475, #129324, #79557 ) ;
#61728 = ADVANCED_FACE ( 'NONE', ( #14794 ), #62178, .T. ) ;
#61729 = VECTOR ( 'NONE', #29305, 1000.000000000000000 ) ;
#61730 = CARTESIAN_POINT ( 'NONE',  ( 5.449999999999936229, 2.500000000000000000, -2.165063509461101710 ) ) ;
#61731 = PRESENTATION_STYLE_ASSIGNMENT (( #91816 ) ) ;
#61732 = CARTESIAN_POINT ( 'NONE',  ( -0.6000000000000323963, 12.50000000000000000, 0.2813168883297385570 ) ) ;
#61733 = EDGE_CURVE ( 'NONE', #54782, #74101, #24517, .T. ) ;
#61734 = FACE_OUTER_BOUND ( 'NONE', #93496, .T. ) ;
#61735 = DIRECTION ( 'NONE',  ( 0.000000000000000000, 1.000000000000000000, 0.000000000000000000 ) ) ;
#61736 = DIRECTION ( 'NONE',  ( 0.000000000000000000, 0.000000000000000000, -1.000000000000000000 ) ) ;
#61737 = VERTEX_POINT ( 'NONE', #15458 ) ;
#61739 = EDGE_CURVE ( 'NONE', #62716, #42325, #72636, .T. ) ;
#61738 = DIRECTION ( 'NONE',  ( 0.000000000000000000, 1.000000000000000000, 0.000000000000000000 ) ) ;
#61740 = ORIENTED_EDGE ( 'NONE', *, *, #57300, .T. ) ;
#61741 = CIRCLE ( 'NONE', #22025, 0.06509327318403745899 ) ;
#61742 = ADVANCED_FACE ( 'NONE', ( #55403 ), #47503, .T. ) ;
#61743 = ORIENTED_EDGE ( 'NONE', *, *, #67113, .T. ) ;
#61744 = ORIENTED_EDGE ( 'NONE', *, *, #84002, .T. ) ;
#61745 = CARTESIAN_POINT ( 'NONE',  ( -0.6000000000000383915, 2.500000000000000000, -4.083716857408426826 ) ) ;
#61746 = ORIENTED_EDGE ( 'NONE', *, *, #57411, .T. ) ;
#61747 = EDGE_LOOP ( 'NONE', ( #36371, #72227, #93420, #56777 ) ) ;
#61748 = ORIENTED_EDGE ( 'NONE', *, *, #75548, .F. ) ;
#61750 = CONICAL_SURFACE ( 'NONE', #5276, 0.1000000000000002554, 0.003490658503988666988 ) ;
#61749 = CARTESIAN_POINT ( 'NONE',  ( -12.09999999999999609, 12.50000000000000000, -4.265033745738161741 ) ) ;
#61751 = CARTESIAN_POINT ( 'NONE',  ( -9.150000000000005684, 12.50000000000000000, 7.122917578226811486 ) ) ;
#61752 = AXIS2_PLACEMENT_3D ( 'NONE', #5478, #45433, #85346 ) ;
#61753 = DIRECTION ( 'NONE',  ( -0.000000000000000000, -1.000000000000000000, -0.000000000000000000 ) ) ;
#61754 = DIRECTION ( 'NONE',  ( 0.000000000000000000, 0.000000000000000000, -1.000000000000000000 ) ) ;
#61755 = DIRECTION ( 'NONE',  ( 0.000000000000000000, 0.000000000000000000, -1.000000000000000000 ) ) ;
#61756 = CARTESIAN_POINT ( 'NONE',  ( -14.59999999999998366, 12.50000000000000000, -0.6928203230275520319 ) ) ;
#61757 = ORIENTED_EDGE ( 'NONE', *, *, #84108, .F. ) ;
#61758 = CARTESIAN_POINT ( 'NONE',  ( 8.149999999999920419, 2.500000000000000000, -2.511473670974877948 ) ) ;
#61759 = VERTEX_POINT ( 'NONE', #35762 ) ;
#61760 = DIRECTION ( 'NONE',  ( -0.000000000000000000, 1.000000000000000000, -0.000000000000000000 ) ) ;
#61761 = EDGE_LOOP ( 'NONE', ( #23742, #95682 ) ) ;
#61762 = DIRECTION ( 'NONE',  ( -4.274815082592931898E-19, -0.9999939076577903929, -0.003490651415223739937 ) ) ;
#61763 = CIRCLE ( 'NONE', #67995, 0.06509327318403745899 ) ;
#61764 = ORIENTED_EDGE ( 'NONE', *, *, #125776, .T. ) ;
#61765 = CARTESIAN_POINT ( 'NONE',  ( 14.14999999999989377, 2.500000000000000000, -2.757883832488654097 ) ) ;
#61766 = CONICAL_SURFACE ( 'NONE', #72232, 0.1000000000000000472, 0.003490658503988666988 ) ;
#61768 = CARTESIAN_POINT ( 'NONE',  ( 4.549999999999939426, 2.500000000000000000, -2.265063509461101798 ) ) ;
#61767 = AXIS2_PLACEMENT_3D ( 'NONE', #29717, #80113, #49382 ) ;
#61769 = ORIENTED_EDGE ( 'NONE', *, *, #22088, .T. ) ;
#61770 = AXIS2_PLACEMENT_3D ( 'NONE', #81976, #53809, #22444 ) ;
#61771 = ORIENTED_EDGE ( 'NONE', *, *, #6107, .F. ) ;
#61772 = CARTESIAN_POINT ( 'NONE',  ( 9.549999999999918998, 2.500000000000000000, 2.065063509461097624 ) ) ;
#61773 = CARTESIAN_POINT ( 'NONE',  ( -11.64999999999999680, 2.500000000000000000, 5.802370205355744659 ) ) ;
#61774 = DIRECTION ( 'NONE',  ( -4.274815082592931898E-19, -0.9999939076577903929, -0.003490651415223739937 ) ) ;
#61775 = CARTESIAN_POINT ( 'NONE',  ( -0.6000000000000323963, 12.50000000000000000, -0.2813168883297385570 ) ) ;
#61776 = AXIS2_PLACEMENT_3D ( 'NONE', #26967, #128412, #38746 ) ;
#61778 = ADVANCED_FACE ( 'NONE', ( #115590 ), #25947, .T. ) ;
#61777 = DIRECTION ( 'NONE',  ( -0.000000000000000000, -1.000000000000000000, -0.000000000000000000 ) ) ;
#61779 = CONICAL_SURFACE ( 'NONE', #111937, 0.1000000000000002554, 0.003490658503988666988 ) ;
#61780 = EDGE_LOOP ( 'NONE', ( #29546, #67352 ) ) ;
#61781 = CIRCLE ( 'NONE', #17835, 0.06509327318403745899 ) ;
#61782 = CARTESIAN_POINT ( 'NONE',  ( -5.850000000000018296, 2.500000000000000000, 5.702370205355745014 ) ) ;
#61783 = ORIENTED_EDGE ( 'NONE', *, *, #77752, .T. ) ;
#61784 = CARTESIAN_POINT ( 'NONE',  ( 179.5000000000000000, 0.000000000000000000, 0.000000000000000000 ) ) ;
#61786 = VECTOR ( 'NONE', #64254, 1000.000000000000000 ) ;
#61785 = DIRECTION ( 'NONE',  ( 0.000000000000000000, -0.9999939076577903929, 0.003490651415223739937 ) ) ;
#61787 = AXIS2_PLACEMENT_3D ( 'NONE', #89875, #80720, #195 ) ;
#61788 = VECTOR ( 'NONE', #125651, 1000.000000000000000 ) ;
#61789 = CARTESIAN_POINT ( 'NONE',  ( 187.4218750003414016, 0.000000000000000000, 7.564683531250000925 ) ) ;
#61790 = CARTESIAN_POINT ( 'NONE',  ( 0.4499999999999552136, 2.500000000000000000, 6.595190528383296780 ) ) ;
#61791 = LINE ( 'NONE', #83358, #73746 ) ;
#61792 = FACE_OUTER_BOUND ( 'NONE', #19505, .T. ) ;
#61793 = DIRECTION ( 'NONE',  ( 0.000000000000000000, 0.000000000000000000, 1.000000000000000000 ) ) ;
#61794 = ORIENTED_EDGE ( 'NONE', *, *, #476, .T. ) ;
#61795 = FACE_OUTER_BOUND ( 'NONE', #100207, .T. ) ;
#61796 = DIRECTION ( 'NONE',  ( 0.000000000000000000, 1.000000000000000000, 0.000000000000000000 ) ) ;
#61797 = CARTESIAN_POINT ( 'NONE',  ( -13.54999999999999005, 2.500000000000000000, -1.818653347947323917 ) ) ;
#61798 = ORIENTED_EDGE ( 'NONE', *, *, #93164, .T. ) ;
#61799 = VECTOR ( 'NONE', #86457, 1000.000000000000000 ) ;
#61800 = ORIENTED_EDGE ( 'NONE', *, *, #124663, .F. ) ;
#61801 = CARTESIAN_POINT ( 'NONE',  ( -3.150000000000030553, 2.500000000000000000, 6.148780366869520009 ) ) ;
#61802 = ORIENTED_EDGE ( 'NONE', *, *, #121067, .T. ) ;
#61803 = EDGE_LOOP ( 'NONE', ( #24716, #76737 ) ) ;
#61804 = FACE_OUTER_BOUND ( 'NONE', #78049, .T. ) ;
#61805 = ORIENTED_EDGE ( 'NONE', *, *, #33169, .T. ) ;
#61807 = EDGE_CURVE ( 'NONE', #122474, #112402, #103935, .T. ) ;
#61806 = CARTESIAN_POINT ( 'NONE',  ( 16.84158739989841180, -0.4722467112506605336, -5.802037699235492063 ) ) ;
#61808 = DIRECTION ( 'NONE',  ( -0.000000000000000000, -1.000000000000000000, -0.000000000000000000 ) ) ;
#61809 = CARTESIAN_POINT ( 'NONE',  ( 17.17539648375905870, 2.541523116374017732, 5.507477068182278224 ) ) ;
#61810 = AXIS2_PLACEMENT_3D ( 'NONE', #9370, #107573, #57834 ) ;
#61811 = CONICAL_SURFACE ( 'NONE', #5353, 0.1000000000000002554, 0.003490658503988666988 ) ;
#61812 = ORIENTED_EDGE ( 'NONE', *, *, #14651, .F. ) ;
#61813 = ADVANCED_FACE ( 'NONE', ( #119460 ), #60134, .T. ) ;
#61814 = CARTESIAN_POINT ( 'NONE',  ( 107.9999999999992895, 5.855766388783293586, 5.000000000000080824 ) ) ;
#61815 = CARTESIAN_POINT ( 'NONE',  ( 6.899999999999926636, 12.50000000000000000, -0.3464101615137782364 ) ) ;
#61816 = ADVANCED_FACE ( 'NONE', ( #100478 ), #66449, .T. ) ;
#61817 = EDGE_CURVE ( 'NONE', #16509, #120005, #30885, .T. ) ;
#61818 = ORIENTED_EDGE ( 'NONE', *, *, #5818, .T. ) ;
#61819 = CIRCLE ( 'NONE', #36785, 0.09999999999999982514 ) ;
#61820 = ORIENTED_EDGE ( 'NONE', *, *, #98170, .F. ) ;
#61821 = VECTOR ( 'NONE', #98684, 1000.000000000000000 ) ;
#61822 = ORIENTED_EDGE ( 'NONE', *, *, #29572, .T. ) ;
#61823 = CARTESIAN_POINT ( 'NONE',  ( 1.449999999999949551, 12.50000000000000000, 6.841600689897072485 ) ) ;
#61824 = CARTESIAN_POINT ( 'NONE',  ( 184.0312500006828031, 9.429780353434619030E-16, -7.700000000000000178 ) ) ;
#61825 = EDGE_CURVE ( 'NONE', #49326, #116833, #104023, .T. ) ;
#61826 = ADVANCED_FACE ( 'NONE', ( #60582 ), #47598, .T. ) ;
#61827 = DIRECTION ( 'NONE',  ( 0.000000000000000000, 0.000000000000000000, -1.000000000000000000 ) ) ;
#61828 = ADVANCED_FACE ( 'NONE', ( #98522 ), #7862, .T. ) ;
#61829 = FACE_BOUND ( 'NONE', #15169, .T. ) ;
#61830 = ORIENTED_EDGE ( 'NONE', *, *, #87493, .F. ) ;
#61831 = EDGE_CURVE ( 'NONE', #92562, #48804, #55980, .T. ) ;
#61832 = CARTESIAN_POINT ( 'NONE',  ( 11.84999999999990727, 12.50000000000000000, -2.511473670974877948 ) ) ;
#61833 = DIRECTION ( 'NONE',  ( 0.000000000000000000, 0.000000000000000000, -1.000000000000000000 ) ) ;
#61834 = ORIENTED_EDGE ( 'NONE', *, *, #9216, .T. ) ;
#61835 = CARTESIAN_POINT ( 'NONE',  ( 8.749999999999921840, 12.50000000000000000, 2.857883832488649301 ) ) ;
#61836 = CARTESIAN_POINT ( 'NONE',  ( 0.8499999999999553468, 12.50000000000000000, -2.165063509461101710 ) ) ;
#61837 = LINE ( 'NONE', #63761, #109217 ) ;
#61838 = DIRECTION ( 'NONE',  ( -0.000000000000000000, 1.000000000000000000, -0.000000000000000000 ) ) ;
#61839 = DIRECTION ( 'NONE',  ( -0.000000000000000000, 1.000000000000000000, -0.000000000000000000 ) ) ;
#61840 = EDGE_CURVE ( 'NONE', #105625, #116790, #99830, .T. ) ;
#61841 = LINE ( 'NONE', #40925, #32578 ) ;
#61842 = DIRECTION ( 'NONE',  ( 0.000000000000000000, 1.000000000000000000, 0.000000000000000000 ) ) ;
#61843 = EDGE_LOOP ( 'NONE', ( #79897, #97985, #42614, #91007 ) ) ;
#61844 = ORIENTED_EDGE ( 'NONE', *, *, #13656, .F. ) ;
#61845 = EDGE_LOOP ( 'NONE', ( #129141, #25413, #64876, #100826 ) ) ;
#61846 = ORIENTED_EDGE ( 'NONE', *, *, #67618, .F. ) ;
#61847 = CARTESIAN_POINT ( 'NONE',  ( 14.99999999999992895, 12.50000000000000000, -2.276824562219559311E-15 ) ) ;
#61848 = DIRECTION ( 'NONE',  ( 0.000000000000000000, 0.000000000000000000, -1.000000000000000000 ) ) ;
#61849 = ORIENTED_EDGE ( 'NONE', *, *, #93266, .T. ) ;
#61850 = FACE_BOUND ( 'NONE', #33592, .T. ) ;
#61851 = CARTESIAN_POINT ( 'NONE',  ( 11.04999999999990834, 2.500000000000000000, -6.841600689897077814 ) ) ;
#61852 = CARTESIAN_POINT ( 'NONE',  ( -6.700000000000019718, 2.500000000000000000, -2.385244779468109755E-15 ) ) ;
#61853 = CARTESIAN_POINT ( 'NONE',  ( -6.850000000000013856, 2.500000000000000000, 6.048780366869521252 ) ) ;
#61854 = LINE ( 'NONE', #113512, #93034 ) ;
#61855 = AXIS2_PLACEMENT_3D ( 'NONE', #118091, #109574, #79480 ) ;
#61856 = DIRECTION ( 'NONE',  ( 0.000000000000000000, 1.000000000000000000, 0.000000000000000000 ) ) ;
#61857 = CARTESIAN_POINT ( 'NONE',  ( 12.69999999999990159, 2.500000000000000000, -3.983716857408426293 ) ) ;
#61858 = CARTESIAN_POINT ( 'NONE',  ( 3.349999999999945466, 2.500000000000000000, -2.165063509461101710 ) ) ;
#61859 = CARTESIAN_POINT ( 'NONE',  ( 4.799999999999937650, 2.500000000000000000, -3.983716857408426293 ) ) ;
#61860 = ADVANCED_FACE ( 'NONE', ( #27872 ), #118184, .T. ) ;
#61861 = DIRECTION ( 'NONE',  ( -0.000000000000000000, -1.000000000000000000, -0.000000000000000000 ) ) ;
#61862 = ORIENTED_EDGE ( 'NONE', *, *, #72895, .F. ) ;
#61863 = ORIENTED_EDGE ( 'NONE', *, *, #28440, .F. ) ;
#61864 = VERTEX_POINT ( 'NONE', #108362 ) ;
#61865 = EDGE_LOOP ( 'NONE', ( #4703, #96253, #76397, #48152 ) ) ;
#61866 = EDGE_LOOP ( 'NONE', ( #113763, #75083, #44286, #92155 ) ) ;
#61867 = VERTEX_POINT ( 'NONE', #323 ) ;
#61868 = VERTEX_POINT ( 'NONE', #129325 ) ;
#61869 = CONICAL_SURFACE ( 'NONE', #28413, 0.09999999999999982514, 0.003490658503988666988 ) ;
#61870 = CARTESIAN_POINT ( 'NONE',  ( -11.84999999999999787, 2.500000000000000000, -1.818653347947321919 ) ) ;
#61871 = EDGE_CURVE ( 'NONE', #121723, #90081, #93555, .T. ) ;
#61872 = VERTEX_POINT ( 'NONE', #69732 ) ;
#61873 = EDGE_LOOP ( 'NONE', ( #61188, #56382, #101214, #73369 ) ) ;
#61874 = EDGE_CURVE ( 'NONE', #27091, #70439, #120744, .T. ) ;
#61875 = AXIS2_PLACEMENT_3D ( 'NONE', #27143, #67037, #17286 ) ;
#61876 = VECTOR ( 'NONE', #106750, 1000.000000000000000 ) ;
#61877 = ADVANCED_FACE ( 'NONE', ( #88726 ), #37135, .T. ) ;
#61878 = AXIS2_PLACEMENT_3D ( 'NONE', #45949, #85844, #125760 ) ;
#61879 = CARTESIAN_POINT ( 'NONE',  ( -6.249999999999984901, 2.500000000000000000, -2.065063509461102065 ) ) ;
#61880 = CARTESIAN_POINT ( 'NONE',  ( 15.22989033368280154, -2.499999999999999556, 7.180069491320001163 ) ) ;
#61881 = CARTESIAN_POINT ( 'NONE',  ( 8.549999999999924327, 12.50000000000000000, 1.818653347947321475 ) ) ;
#61883 = AXIS2_PLACEMENT_3D ( 'NONE', #5086, #3810, #83667 ) ;
#61882 = CARTESIAN_POINT ( 'NONE',  ( 0.3999999999999568345, 2.500000000000000000, -5.022947341949754119 ) ) ;
#61884 = EDGE_CURVE ( 'NONE', #7480, #112355, #51803, .T. ) ;
#61885 = ORIENTED_EDGE ( 'NONE', *, *, #84591, .F. ) ;
#61886 = CARTESIAN_POINT ( 'NONE',  ( 8.949999999999915801, 2.500000000000000000, -1.718653347947326049 ) ) ;
#61887 = EDGE_CURVE ( 'NONE', #72458, #37153, #79001, .T. ) ;
#61888 = EDGE_CURVE ( 'NONE', #35194, #60040, #50113, .T. ) ;
#61889 = ORIENTED_EDGE ( 'NONE', *, *, #106635, .T. ) ;
#61890 = EDGE_CURVE ( 'NONE', #127833, #65132, #110280, .T. ) ;
#61891 = ORIENTED_EDGE ( 'NONE', *, *, #57991, .F. ) ;
#61892 = FACE_OUTER_BOUND ( 'NONE', #3805, .T. ) ;
#61893 = DIRECTION ( 'NONE',  ( 0.000000000000000000, 0.000000000000000000, 1.000000000000000000 ) ) ;
#61894 = AXIS2_PLACEMENT_3D ( 'NONE', #21598, #73919, #11770 ) ;
#61895 = VERTEX_POINT ( 'NONE', #32420 ) ;
#61896 = EDGE_CURVE ( 'NONE', #90044, #80196, #64308, .T. ) ;
#61897 = ORIENTED_EDGE ( 'NONE', *, *, #54109, .F. ) ;
#61898 = CARTESIAN_POINT ( 'NONE',  ( 187.5000000000000000, 0.000000000000000000, 7.700000000000000178 ) ) ;
#61899 = DIRECTION ( 'NONE',  ( 0.000000000000000000, 0.000000000000000000, -1.000000000000000000 ) ) ;
#61900 = DIRECTION ( 'NONE',  ( 0.000000000000000000, 0.000000000000000000, 1.000000000000000000 ) ) ;
#61901 = DIRECTION ( 'NONE',  ( 0.000000000000000000, 1.000000000000000000, 0.000000000000000000 ) ) ;
#61902 = CARTESIAN_POINT ( 'NONE',  ( -3.100000000000028511, 12.50000000000000000, -0.4115034346978156399 ) ) ;
#61903 = AXIS2_PLACEMENT_3D ( 'NONE', #28855, #86465, #126402 ) ;
#61904 = AXIS2_PLACEMENT_3D ( 'NONE', #27675, #67604, #44771 ) ;
#61905 = ORIENTED_EDGE ( 'NONE', *, *, #95679, .F. ) ;
#61907 = AXIS2_PLACEMENT_3D ( 'NONE', #115396, #125879, #15272 ) ;
#61906 = CARTESIAN_POINT ( 'NONE',  ( 3.349999999999944578, 2.500000000000000000, -5.902370205355750521 ) ) ;
#61908 = ORIENTED_EDGE ( 'NONE', *, *, #44710, .F. ) ;
#61909 = AXIS2_PLACEMENT_3D ( 'NONE', #108658, #1284, #79219 ) ;
#61910 = DIRECTION ( 'NONE',  ( 0.000000000000000000, 0.000000000000000000, 1.000000000000000000 ) ) ;
#61911 = FACE_OUTER_BOUND ( 'NONE', #75267, .T. ) ;
#61912 = CARTESIAN_POINT ( 'NONE',  ( 4.799999999999939426, 12.50000000000000000, -4.676537180435977881 ) ) ;
#61913 = CARTESIAN_POINT ( 'NONE',  ( 2.699999999999947331, 2.500000000000000000, -0.2464101615137783419 ) ) ;
#61914 = DIRECTION ( 'NONE',  ( 0.000000000000000000, 0.000000000000000000, 1.000000000000000000 ) ) ;
#61915 = ORIENTED_EDGE ( 'NONE', *, *, #24759, .F. ) ;
#61916 = AXIS2_PLACEMENT_3D ( 'NONE', #89497, #49590, #100590 ) ;
#61917 = LINE ( 'NONE', #112934, #94888 ) ;
#61919 = TOROIDAL_SURFACE ( 'NONE', #5448, 8.199999999999999289, 0.5000000000000000000 ) ;
#61918 = VECTOR ( 'NONE', #41280, 1000.000000000000000 ) ;
#61920 = PLANE ( 'NONE',  #52794 ) ;
#61921 = ORIENTED_EDGE ( 'NONE', *, *, #96216, .F. ) ;
#61922 = EDGE_LOOP ( 'NONE', ( #63887, #106039 ) ) ;
#61923 = EDGE_LOOP ( 'NONE', ( #53291, #47426 ) ) ;
#61924 = CARTESIAN_POINT ( 'NONE',  ( 14.99999999999989164, 2.500000000000000000, 0.6928203230275494784 ) ) ;
#61925 = DIRECTION ( 'NONE',  ( -0.000000000000000000, 1.000000000000000000, -0.000000000000000000 ) ) ;
#61926 = DIRECTION ( 'NONE',  ( 0.000000000000000000, 0.000000000000000000, 1.000000000000000000 ) ) ;
#61927 = DIRECTION ( 'NONE',  ( 0.000000000000000000, -0.9999939076577903929, 0.003490651415223739937 ) ) ;
#61928 = DIRECTION ( 'NONE',  ( 0.000000000000000000, 0.000000000000000000, -1.000000000000000000 ) ) ;
#61930 = ADVANCED_FACE ( 'NONE', ( #52666 ), #42217, .T. ) ;
#61929 = FACE_OUTER_BOUND ( 'NONE', #21582, .T. ) ;
#61931 = CARTESIAN_POINT ( 'NONE',  ( -12.69999999999999218, 2.500000000000000000, 4.776537180435972196 ) ) ;
#61932 = DIRECTION ( 'NONE',  ( -0.000000000000000000, 1.000000000000000000, -0.000000000000000000 ) ) ;
#61933 = EDGE_LOOP ( 'NONE', ( #107813, #52389, #114838, #114584 ) ) ;
#61934 = FACE_OUTER_BOUND ( 'NONE', #46442, .T. ) ;
#61935 = EDGE_CURVE ( 'NONE', #123233, #50100, #72723, .T. ) ;
#61936 = CARTESIAN_POINT ( 'NONE',  ( -9.200000000000006395, 2.500000000000000000, -2.385244779468109755E-15 ) ) ;
#61937 = DIRECTION ( 'NONE',  ( 0.000000000000000000, 0.000000000000000000, -1.000000000000000000 ) ) ;
#61938 = DIRECTION ( 'NONE',  ( 0.000000000000000000, 1.000000000000000000, 0.000000000000000000 ) ) ;
#61939 = ORIENTED_EDGE ( 'NONE', *, *, #17211, .T. ) ;
#61940 = CARTESIAN_POINT ( 'NONE',  ( -8.749999999999975131, 2.500000000000000000, -2.165063509461101710 ) ) ;
#61941 = CIRCLE ( 'NONE', #13791, 0.1000000000000002554 ) ;
#61942 = CIRCLE ( 'NONE', #68179, 0.06509327318403745899 ) ;
#61943 = DIRECTION ( 'NONE',  ( 0.000000000000000000, 0.000000000000000000, -1.000000000000000000 ) ) ;
#61945 = ORIENTED_EDGE ( 'NONE', *, *, #27989, .F. ) ;
#61944 = DIRECTION ( 'NONE',  ( 0.000000000000000000, 0.000000000000000000, -1.000000000000000000 ) ) ;
#61946 = VERTEX_POINT ( 'NONE', #53331 ) ;
#61948 = AXIS2_PLACEMENT_3D ( 'NONE', #119601, #1755, #1121 ) ;
#61947 = AXIS2_PLACEMENT_3D ( 'NONE', #69652, #42135, #91233 ) ;
#61949 = CARTESIAN_POINT ( 'NONE',  ( 187.0000000000000000, 0.000000000000000000, 7.700000000000000178 ) ) ;
#61950 = ORIENTED_EDGE ( 'NONE', *, *, #46424, .F. ) ;
#61951 = ORIENTED_EDGE ( 'NONE', *, *, #67031, .F. ) ;
#61952 = DIRECTION ( 'NONE',  ( 0.000000000000000000, 1.000000000000000000, 0.000000000000000000 ) ) ;
#61953 = DIRECTION ( 'NONE',  ( 0.000000000000000000, 0.000000000000000000, -1.000000000000000000 ) ) ;
#61954 = FACE_OUTER_BOUND ( 'NONE', #67363, .T. ) ;
#61956 = CIRCLE ( 'NONE', #5499, 0.06509327318403745899 ) ;
#61955 = CIRCLE ( 'NONE', #93261, 0.1000000000000000472 ) ;
#61957 = CARTESIAN_POINT ( 'NONE',  ( 5.649999999999934630, 2.500000000000000000, -1.718653347947325827 ) ) ;
#61958 = ORIENTED_EDGE ( 'NONE', *, *, #12608, .F. ) ;
#61960 = EDGE_CURVE ( 'NONE', #91248, #80232, #113520, .T. ) ;
#61959 = CIRCLE ( 'NONE', #15963, 0.09999999999999982514 ) ;
#61961 = DIRECTION ( 'NONE',  ( 0.000000000000000000, 1.000000000000000000, 0.000000000000000000 ) ) ;
#61962 = VERTEX_POINT ( 'NONE', #91303 ) ;
#61963 = CARTESIAN_POINT ( 'NONE',  ( 8.299999999999922551, 2.500000000000000000, 4.330127018922196314 ) ) ;
#61964 = EDGE_CURVE ( 'NONE', #113935, #27857, #22568, .T. ) ;
#61965 = ORIENTED_EDGE ( 'NONE', *, *, #70021, .T. ) ;
#61966 = ORIENTED_EDGE ( 'NONE', *, *, #13698, .T. ) ;
#61967 = ORIENTED_EDGE ( 'NONE', *, *, #78244, .T. ) ;
#61968 = ORIENTED_EDGE ( 'NONE', *, *, #35840, .T. ) ;
#61969 = CARTESIAN_POINT ( 'NONE',  ( 0.3999999999999619971, 2.500000000000000000, 0.09999999999999989453 ) ) ;
#61970 = CARTESIAN_POINT ( 'NONE',  ( 14.69113575703644869, 2.500000000000000000, 6.337000354879313235 ) ) ;
#61971 = EDGE_CURVE ( 'NONE', #90560, #4778, #81050, .T. ) ;
#61972 = ADVANCED_FACE ( 'NONE', ( #110929 ), #12095, .T. ) ;
#61973 = CARTESIAN_POINT ( 'NONE',  ( -1.900000000000034106, 12.50000000000000000, 0.2813168883297361700 ) ) ;
#61974 = ADVANCED_FACE ( 'NONE', ( #23868 ), #12074, .T. ) ;
#61975 = FACE_BOUND ( 'NONE', #81377, .T. ) ;
#61977 = EDGE_CURVE ( 'NONE', #94015, #18162, #31120, .T. ) ;
#61976 = VERTEX_POINT ( 'NONE', #1626 ) ;
#61978 = DIRECTION ( 'NONE',  ( 0.000000000000000000, 0.000000000000000000, -1.000000000000000000 ) ) ;
#61979 = AXIS2_PLACEMENT_3D ( 'NONE', #89537, #77766, #99372 ) ;
#61980 = CARTESIAN_POINT ( 'NONE',  ( 186.9843750003414300, -8.734944146203032389, -1.604583208406768146E-15 ) ) ;
#61981 = DIRECTION ( 'NONE',  ( -0.000000000000000000, 1.000000000000000000, -0.000000000000000000 ) ) ;
#61982 = DIRECTION ( 'NONE',  ( -0.000000000000000000, -1.000000000000000000, -0.000000000000000000 ) ) ;
#61983 = AXIS2_PLACEMENT_3D ( 'NONE', #25229, #105080, #15409 ) ;
#61984 = AXIS2_PLACEMENT_3D ( 'NONE', #6805, #5537, #76874 ) ;
#61985 = DIRECTION ( 'NONE',  ( 0.000000000000000000, 1.000000000000000000, 0.000000000000000000 ) ) ;
#61986 = PLANE ( 'NONE',  #25940 ) ;
#61987 = EDGE_CURVE ( 'NONE', #17533, #35519, #123346, .T. ) ;
#61988 = CARTESIAN_POINT ( 'NONE',  ( -9.150000000000011013, 2.500000000000000000, -5.702370205355745014 ) ) ;
#61989 = AXIS2_PLACEMENT_3D ( 'NONE', #85166, #125093, #35438 ) ;
#61990 = AXIS2_PLACEMENT_3D ( 'NONE', #80674, #110755, #1449 ) ;
#61991 = ADVANCED_FACE ( 'NONE', ( #43517 ), #122903, .T. ) ;
#61992 = ADVANCED_FACE ( 'NONE', ( #72328 ), #45541, .T. ) ;
#61993 = CARTESIAN_POINT ( 'NONE',  ( 12.09999999999990550, 2.500000000000000000, -3.737306695894649700 ) ) ;
#61994 = CONICAL_SURFACE ( 'NONE', #7594, 0.1000000000000002554, 0.003490658503988666988 ) ;
#61995 = EDGE_LOOP ( 'NONE', ( #2901, #69380, #9464, #18119 ) ) ;
#61996 = ORIENTED_EDGE ( 'NONE', *, *, #121073, .T. ) ;
#61997 = VERTEX_POINT ( 'NONE', #122067 ) ;
#61998 = ORIENTED_EDGE ( 'NONE', *, *, #42610, .T. ) ;
#61999 = ORIENTED_EDGE ( 'NONE', *, *, #38811, .F. ) ;
#62000 = CARTESIAN_POINT ( 'NONE',  ( 11.69999999999990870, 2.500000000000000000, 4.330127018922196314 ) ) ;
#62001 = CARTESIAN_POINT ( 'NONE',  ( 0.3999999999999563904, 12.50000000000000000, 3.637306695894644726 ) ) ;
#62002 = VERTEX_POINT ( 'NONE', #33679 ) ;
#62003 = FACE_BOUND ( 'NONE', #3438, .T. ) ;
#62005 = DIRECTION ( 'NONE',  ( 0.000000000000000000, 1.000000000000000000, 0.000000000000000000 ) ) ;
#62004 = CIRCLE ( 'NONE', #116356, 0.1000000000000002554 ) ;
#62007 = VECTOR ( 'NONE', #94357, 1000.000000000000000 ) ;
#62006 = AXIS2_PLACEMENT_3D ( 'NONE', #10356, #90850, #68625 ) ;
#62008 = VERTEX_POINT ( 'NONE', #72962 ) ;
#62009 = CARTESIAN_POINT ( 'NONE',  ( 2.899999999999943956, 2.500000000000000000, 4.430127018922196847 ) ) ;
#62010 = CARTESIAN_POINT ( 'NONE',  ( -11.64999999999999680, 12.50000000000000000, 6.495190528383297135 ) ) ;
#62011 = FACE_OUTER_BOUND ( 'NONE', #117984, .T. ) ;
#62012 = ORIENTED_EDGE ( 'NONE', *, *, #86678, .T. ) ;
#62013 = DIRECTION ( 'NONE',  ( -4.274815082592931898E-19, -0.9999939076577903929, -0.003490651415223739937 ) ) ;
#62014 = ORIENTED_EDGE ( 'NONE', *, *, #118887, .F. ) ;
#62015 = ORIENTED_EDGE ( 'NONE', *, *, #41790, .F. ) ;
#62016 = VERTEX_POINT ( 'NONE', #83434 ) ;
#62017 = DIRECTION ( 'NONE',  ( 0.000000000000000000, -0.000000000000000000, 1.000000000000000000 ) ) ;
#62018 = DIRECTION ( 'NONE',  ( 0.000000000000000000, 0.000000000000000000, 1.000000000000000000 ) ) ;
#62019 = EDGE_LOOP ( 'NONE', ( #69891, #71035, #116243, #67884 ) ) ;
#62020 = LINE ( 'NONE', #12250, #80962 ) ;
#62021 = DIRECTION ( 'NONE',  ( -0.000000000000000000, 1.000000000000000000, -0.000000000000000000 ) ) ;
#62022 = CARTESIAN_POINT ( 'NONE',  ( 7.099999999999925926, 12.50000000000000000, 0.6928203230275494784 ) ) ;
#62023 = DIRECTION ( 'NONE',  ( 0.000000000000000000, 1.000000000000000000, 0.000000000000000000 ) ) ;
#62024 = CARTESIAN_POINT ( 'NONE',  ( 185.8645833340161175, -6.668395609140180369, 3.849999999999994760 ) ) ;
#62025 = ORIENTED_EDGE ( 'NONE', *, *, #22255, .F. ) ;
#62026 = DIRECTION ( 'NONE',  ( -0.000000000000000000, -1.000000000000000000, -0.000000000000000000 ) ) ;
#62027 = EDGE_CURVE ( 'NONE', #106414, #34384, #58065, .T. ) ;
#62028 = ORIENTED_EDGE ( 'NONE', *, *, #116669, .F. ) ;
#62029 = CARTESIAN_POINT ( 'NONE',  ( 10.39999999999991154, 2.500000000000000000, -3.537306695894649966 ) ) ;
#62030 = EDGE_CURVE ( 'NONE', #46732, #24133, #40946, .T. ) ;
#62031 = AXIS2_PLACEMENT_3D ( 'NONE', #123044, #102736, #104044 ) ;
#62032 = ORIENTED_EDGE ( 'NONE', *, *, #108036, .F. ) ;
#62033 = AXIS2_PLACEMENT_3D ( 'NONE', #42470, #100712, #112489 ) ;
#62035 = EDGE_CURVE ( 'NONE', #30567, #28910, #71029, .T. ) ;
#62034 = CARTESIAN_POINT ( 'NONE',  ( -5.850000000000018296, 12.50000000000000000, 5.802370205355744659 ) ) ;
#62036 = VERTEX_POINT ( 'NONE', #81493 ) ;
#62037 = CYLINDRICAL_SURFACE ( 'NONE', #76412, 3.000000000000000000 ) ;
#62038 = CARTESIAN_POINT ( 'NONE',  ( 187.5000000000000000, 0.000000000000000000, 0.000000000000000000 ) ) ;
#62039 =( BOUNDED_SURFACE ( )  B_SPLINE_SURFACE ( 3, 2, ( 
 ( #81442, #23151, #108467 ),
 ( #8972, #12673, #63080 ),
 ( #62453, #52609, #112831 ),
 ( #102370, #71606, #120713 ),
 ( #111537, #18796, #2878 ),
 ( #128790, #2210, #93197 ),
 ( #91253, #58737, #39123 ),
 ( #78389, #98636, #51353 ),
 ( #32369, #1572, #31693 ),
 ( #102994, #13321, #80802 ),
 ( #53277, #92532, #3518 ),
 ( #118294, #121348, #61806 ),
 ( #48927, #82071, #28638 ),
 ( #61149, #72273, #72905 ) ),
 .UNSPECIFIED., .F., .F., .T. ) 
 B_SPLINE_SURFACE_WITH_KNOTS ( ( 4, 2, 2, 2, 2, 2, 4 ),
 ( 3, 3 ),
 ( 0.000000000000000000, 0.001744612550437227034, 0.002616918825655840768, 0.003489225100874454068, 0.005233837651311681535, 0.006106143926530294835, 0.006978450201748908135 ),
 ( 0.000000000000000000, 1.000000000000000000 ),
 .UNSPECIFIED. ) 
 GEOMETRIC_REPRESENTATION_ITEM ( )  RATIONAL_B_SPLINE_SURFACE ( (
 ( 1.000000000000000000, 0.7318752858502194369, 1.000000000000000000),
 ( 1.000000000000000000, 0.7270130115583837149, 1.000000000000000000),
 ( 1.000000000000000000, 0.7223762446132400150, 1.000000000000000000),
 ( 1.000000000000000000, 0.7156127915554295615, 1.000000000000000000),
 ( 1.000000000000000000, 0.7133893117690700558, 1.000000000000000000),
 ( 1.000000000000000000, 0.7090389252574490486, 1.000000000000000000),
 ( 1.000000000000000000, 0.7069297463491782674, 1.000000000000000000),
 ( 1.000000000000000000, 0.7010696893198986590, 1.000000000000000000),
 ( 1.000000000000000000, 0.6977361265597721296, 1.000000000000000000),
 ( 1.000000000000000000, 0.6948030504688549325, 1.000000000000000000),
 ( 1.000000000000000000, 0.6942033558615769984, 1.000000000000000000),
 ( 1.000000000000000000, 0.6937817651808135810, 1.000000000000000000),
 ( 1.000000000000000000, 0.6939284133497518603, 1.000000000000000000),
 ( 1.000000000000000000, 0.6944177883068419765, 1.000000000000000000) ) ) 
 REPRESENTATION_ITEM ( '' )  SURFACE ( )  );
#62040 = FACE_OUTER_BOUND ( 'NONE', #14380, .T. ) ;
#62041 = FACE_OUTER_BOUND ( 'NONE', #108349, .T. ) ;
#62042 = FACE_OUTER_BOUND ( 'NONE', #10284, .T. ) ;
#62043 = EDGE_LOOP ( 'NONE', ( #111356, #65420 ) ) ;
#62044 = EDGE_CURVE ( 'NONE', #15792, #100531, #91500, .T. ) ;
#62047 = ORIENTED_EDGE ( 'NONE', *, *, #25565, .F. ) ;
#62046 = CIRCLE ( 'NONE', #5570, 0.06509327318403745899 ) ;
#62045 = AXIS2_PLACEMENT_3D ( 'NONE', #44556, #24914, #82561 ) ;
#62048 = DIRECTION ( 'NONE',  ( 0.000000000000000000, -0.000000000000000000, 1.000000000000000000 ) ) ;
#62049 = LINE ( 'NONE', #101965, #70317 ) ;
#62050 = FACE_OUTER_BOUND ( 'NONE', #82098, .T. ) ;
#62052 = EDGE_LOOP ( 'NONE', ( #55688, #83391, #44234, #116011 ) ) ;
#62051 = EDGE_LOOP ( 'NONE', ( #48428, #21, #102318, #58236 ) ) ;
#62053 = EDGE_LOOP ( 'NONE', ( #101859, #99314, #89812, #102316 ) ) ;
#62054 = AXIS2_PLACEMENT_3D ( 'NONE', #53799, #114021, #24352 ) ;
#62055 = CARTESIAN_POINT ( 'NONE',  ( 0.000000000000000000, 0.000000000000000000, -5.000000000000004441 ) ) ;
#62057 = AXIS2_PLACEMENT_3D ( 'NONE', #47817, #108651, #27493 ) ;
#62056 = VECTOR ( 'NONE', #111316, 1000.000000000000000 ) ;
#62058 = ORIENTED_EDGE ( 'NONE', *, *, #98017, .T. ) ;
#62059 = CARTESIAN_POINT ( 'NONE',  ( 1.449999999999952660, 2.500000000000000000, -6.841600689897078702 ) ) ;
#62060 = DIRECTION ( 'NONE',  ( 0.000000000000000000, 0.000000000000000000, 1.000000000000000000 ) ) ;
#62061 = VECTOR ( 'NONE', #113502, 1000.000000000000000 ) ;
#62062 = DIRECTION ( 'NONE',  ( 0.000000000000000000, 0.000000000000000000, 1.000000000000000000 ) ) ;
#62063 = ORIENTED_EDGE ( 'NONE', *, *, #18954, .F. ) ;
#62064 = DIRECTION ( 'NONE',  ( -4.274815082592931898E-19, -0.9999939076577903929, -0.003490651415223739937 ) ) ;
#62065 = LINE ( 'NONE', #11655, #88443 ) ;
#62066 = DIRECTION ( 'NONE',  ( -0.000000000000000000, 1.000000000000000000, -0.000000000000000000 ) ) ;
#62067 = FACE_OUTER_BOUND ( 'NONE', #40949, .T. ) ;
#62068 = EDGE_CURVE ( 'NONE', #125864, #12245, #28817, .T. ) ;
#62069 = DIRECTION ( 'NONE',  ( 0.000000000000000000, 0.000000000000000000, -1.000000000000000000 ) ) ;
#62070 = ORIENTED_EDGE ( 'NONE', *, *, #80662, .F. ) ;
#62071 = DIRECTION ( 'NONE',  ( 0.000000000000000000, 0.000000000000000000, 1.000000000000000000 ) ) ;
#62072 = VERTEX_POINT ( 'NONE', #95176 ) ;
#62073 = ORIENTED_EDGE ( 'NONE', *, *, #25073, .F. ) ;
#62074 = CARTESIAN_POINT ( 'NONE',  ( 187.1718750003414016, 9.264065473108010111E-16, -7.564683531250000925 ) ) ;
#62075 = CARTESIAN_POINT ( 'NONE',  ( -6.250000000000015987, 2.500000000000000000, 1.472243186433545459 ) ) ;
#62076 = CIRCLE ( 'NONE', #18132, 0.09999999999999982514 ) ;
#62077 = DIRECTION ( 'NONE',  ( -0.000000000000000000, 1.000000000000000000, -0.000000000000000000 ) ) ;
#62078 = AXIS2_PLACEMENT_3D ( 'NONE', #92434, #42057, #83275 ) ;
#62080 = AXIS2_PLACEMENT_3D ( 'NONE', #17729, #47866, #87759 ) ;
#62079 = DIRECTION ( 'NONE',  ( 0.000000000000000000, 0.000000000000000000, 1.000000000000000000 ) ) ;
#62081 = CARTESIAN_POINT ( 'NONE',  ( 87.50000000000001421, -3.975344334345451980, 6.360552532166690476 ) ) ;
#62082 = CARTESIAN_POINT ( 'NONE',  ( 11.64999999999990443, 12.50000000000000000, 2.922977105672686982 ) ) ;
#62083 = CONICAL_SURFACE ( 'NONE', #85039, 0.09999999999999999167, 0.003490658503988666988 ) ;
#62084 = EDGE_CURVE ( 'NONE', #1556, #28294, #112443, .T. ) ;
#62085 = DIRECTION ( 'NONE',  ( -0.000000000000000000, -1.000000000000000000, -0.000000000000000000 ) ) ;
#62086 = DIRECTION ( 'NONE',  ( 0.000000000000000000, 0.000000000000000000, 1.000000000000000000 ) ) ;
#62087 = AXIS2_PLACEMENT_3D ( 'NONE', #76332, #115586, #56028 ) ;
#62088 = AXIS2_PLACEMENT_3D ( 'NONE', #71168, #88878, #128841 ) ;
#62089 = FACE_OUTER_BOUND ( 'NONE', #35538, .T. ) ;
#62090 = ORIENTED_EDGE ( 'NONE', *, *, #100077, .F. ) ;
#62091 = VERTEX_POINT ( 'NONE', #26441 ) ;
#62092 = AXIS2_PLACEMENT_3D ( 'NONE', #79967, #19768, #72096 ) ;
#62093 = ORIENTED_EDGE ( 'NONE', *, *, #39273, .T. ) ;
#62094 = ORIENTED_EDGE ( 'NONE', *, *, #62798, .T. ) ;
#62095 = AXIS2_PLACEMENT_3D ( 'NONE', #45137, #15641, #16912 ) ;
#62096 = ADVANCED_FACE ( 'NONE', ( #24501 ), #116626, .T. ) ;
#62097 = CARTESIAN_POINT ( 'NONE',  ( -1.050000000000038680, 2.500000000000000000, 2.511473670974873507 ) ) ;
#62098 = DIRECTION ( 'NONE',  ( 0.000000000000000000, 0.000000000000000000, 1.000000000000000000 ) ) ;
#62099 = AXIS2_PLACEMENT_3D ( 'NONE', #102226, #123152, #72760 ) ;
#62100 = ORIENTED_EDGE ( 'NONE', *, *, #38862, .T. ) ;
#62101 = DIRECTION ( 'NONE',  ( 0.000000000000000000, 0.000000000000000000, 1.000000000000000000 ) ) ;
#62103 = CIRCLE ( 'NONE', #5631, 0.09999999999999982514 ) ;
#62102 = CIRCLE ( 'NONE', #36962, 0.1000000000000000472 ) ;
#62104 = CARTESIAN_POINT ( 'NONE',  ( -7.499999999999976907, 2.500000000000000000, 4.330127018922196314 ) ) ;
#62105 = VERTEX_POINT ( 'NONE', #5484 ) ;
#62106 = EDGE_CURVE ( 'NONE', #66127, #33429, #18135, .T. ) ;
#62107 = CARTESIAN_POINT ( 'NONE',  ( -10.00000000000000355, 12.50000000000000000, 3.637306695894644726 ) ) ;
#62108 = DIRECTION ( 'NONE',  ( 0.000000000000000000, 0.000000000000000000, -1.000000000000000000 ) ) ;
#62109 = VERTEX_POINT ( 'NONE', #84051 ) ;
#62110 = EDGE_LOOP ( 'NONE', ( #119279, #97987 ) ) ;
#62111 = VERTEX_POINT ( 'NONE', #93891 ) ;
#62112 = ORIENTED_EDGE ( 'NONE', *, *, #16190, .F. ) ;
#62113 = DIRECTION ( 'NONE',  ( 0.000000000000000000, 0.000000000000000000, -1.000000000000000000 ) ) ;
#62114 = VECTOR ( 'NONE', #39183, 1000.000000000000000 ) ;
#62115 = CARTESIAN_POINT ( 'NONE',  ( 4.999999999999933387, 12.50000000000000000, 5.022947341949748790 ) ) ;
#62116 = DIRECTION ( 'NONE',  ( -4.274815082592931898E-19, -0.9999939076577903929, -0.003490651415223739937 ) ) ;
#62117 = CARTESIAN_POINT ( 'NONE',  ( -0.4000000000000396572, 12.50000000000000000, 3.637306695894644726 ) ) ;
#62118 = ORIENTED_EDGE ( 'NONE', *, *, #98325, .F. ) ;
#62119 = EDGE_CURVE ( 'NONE', #35293, #63751, #110370, .T. ) ;
#62120 = CARTESIAN_POINT ( 'NONE',  ( 195.5000000000000000, 0.000000000000000000, -5.000000000000000000 ) ) ;
#62121 = ORIENTED_EDGE ( 'NONE', *, *, #10106, .F. ) ;
#62122 = CARTESIAN_POINT ( 'NONE',  ( -6.900000000000015454, 2.500000000000000000, 4.083716857408420609 ) ) ;
#62123 = CARTESIAN_POINT ( 'NONE',  ( 2.500000000000002220, -2.499999999999999556, -9.999999999999998224 ) ) ;
#62124 = CARTESIAN_POINT ( 'NONE',  ( -8.350000000000013856, 12.50000000000000000, -6.495190528383297135 ) ) ;
#62125 = DIRECTION ( 'NONE',  ( -0.000000000000000000, -1.000000000000000000, -0.000000000000000000 ) ) ;
#62126 = EDGE_CURVE ( 'NONE', #35145, #26812, #25783, .T. ) ;
#62127 = EDGE_LOOP ( 'NONE', ( #117190, #68103 ) ) ;
#62128 = AXIS2_PLACEMENT_3D ( 'NONE', #48342, #126261, #7761 ) ;
#62129 = AXIS2_PLACEMENT_3D ( 'NONE', #97189, #43761, #44378 ) ;
#62130 = VERTEX_POINT ( 'NONE', #64419 ) ;
#62131 = VERTEX_POINT ( 'NONE', #14657 ) ;
#62132 = DIRECTION ( 'NONE',  ( 0.000000000000000000, 1.000000000000000000, 0.000000000000000000 ) ) ;
#62133 = LINE ( 'NONE', #41851, #37284 ) ;
#62134 = EDGE_CURVE ( 'NONE', #68530, #56898, #11874, .T. ) ;
#62135 = ADVANCED_FACE ( 'NONE', ( #96443 ), #120840, .T. ) ;
#62136 = DIRECTION ( 'NONE',  ( -0.000000000000000000, 1.000000000000000000, -0.000000000000000000 ) ) ;
#62137 = EDGE_CURVE ( 'NONE', #80208, #118649, #34898, .T. ) ;
#62138 = FACE_BOUND ( 'NONE', #10761, .T. ) ;
#62139 = EDGE_CURVE ( 'NONE', #65087, #85338, #106282, .T. ) ;
#62140 = FACE_OUTER_BOUND ( 'NONE', #49103, .T. ) ;
#62141 = DIRECTION ( 'NONE',  ( 0.000000000000000000, 1.000000000000000000, 0.000000000000000000 ) ) ;
#62143 = CONICAL_SURFACE ( 'NONE', #72601, 0.1000000000000002554, 0.003490658503988666988 ) ;
#62142 = AXIS2_PLACEMENT_3D ( 'NONE', #96863, #77864, #55656 ) ;
#62144 = CARTESIAN_POINT ( 'NONE',  ( -4.350000000000023626, 2.500000000000000000, 1.818653347947321475 ) ) ;
#62145 = EDGE_CURVE ( 'NONE', #3135, #39693, #30693, .T. ) ;
#62146 = DIRECTION ( 'NONE',  ( 0.000000000000000000, 0.000000000000000000, -1.000000000000000000 ) ) ;
#62147 = EDGE_CURVE ( 'NONE', #42231, #25321, #91307, .T. ) ;
#62148 = CARTESIAN_POINT ( 'NONE',  ( 8.349999999999919709, 2.500000000000000000, -1.472243186433550122 ) ) ;
#62149 = ADVANCED_FACE ( 'NONE', ( #36909 ), #103835, .T. ) ;
#62150 = DIRECTION ( 'NONE',  ( 0.000000000000000000, 1.000000000000000000, 0.000000000000000000 ) ) ;
#62151 = ORIENTED_EDGE ( 'NONE', *, *, #66381, .T. ) ;
#62152 = AXIS2_PLACEMENT_3D ( 'NONE', #43804, #64705, #64068 ) ;
#62153 = CARTESIAN_POINT ( 'NONE',  ( -10.40000000000000213, 2.500000000000000000, 5.022947341949748790 ) ) ;
#62154 = EDGE_CURVE ( 'NONE', #126358, #16718, #99917, .T. ) ;
#62155 = AXIS2_PLACEMENT_3D ( 'NONE', #119955, #59772, #62332 ) ;
#62156 = EDGE_CURVE ( 'NONE', #116689, #85338, #116334, .T. ) ;
#62157 = CARTESIAN_POINT ( 'NONE',  ( -3.642919299551294898E-14, 2.500000000000000000, 0.6928203230275518099 ) ) ;
#62158 = ORIENTED_EDGE ( 'NONE', *, *, #46584, .F. ) ;
#62159 = ORIENTED_EDGE ( 'NONE', *, *, #97466, .T. ) ;
#62160 = DIRECTION ( 'NONE',  ( 0.000000000000000000, 0.000000000000000000, 1.000000000000000000 ) ) ;
#62161 = DIRECTION ( 'NONE',  ( 0.000000000000000000, -0.9999939076577903929, 0.003490651415223739937 ) ) ;
#62162 = FACE_BOUND ( 'NONE', #125779, .T. ) ;
#62163 = ADVANCED_FACE ( 'NONE', ( #46719 ), #26748, .T. ) ;
#62164 = DIRECTION ( 'NONE',  ( 0.000000000000000000, 0.000000000000000000, -1.000000000000000000 ) ) ;
#62165 = VERTEX_POINT ( 'NONE', #76828 ) ;
#62166 = CARTESIAN_POINT ( 'NONE',  ( 0.000000000000000000, 2.500000000000000000, 0.1000000000000000056 ) ) ;
#62167 = DIRECTION ( 'NONE',  ( 0.000000000000000000, 0.000000000000000000, 1.000000000000000000 ) ) ;
#62168 = VECTOR ( 'NONE', #28865, 1000.000000000000000 ) ;
#62169 = VERTEX_POINT ( 'NONE', #4839 ) ;
#62170 = LINE ( 'NONE', #90971, #105507 ) ;
#62171 = AXIS2_PLACEMENT_3D ( 'NONE', #77713, #69179, #60047 ) ;
#62172 = CARTESIAN_POINT ( 'NONE',  ( -4.350000000000023626, 12.50000000000000000, 6.083687093685483660 ) ) ;
#62173 = AXIS2_PLACEMENT_3D ( 'NONE', #13309, #12025, #53259 ) ;
#62174 = VERTEX_POINT ( 'NONE', #44797 ) ;
#62175 = DIRECTION ( 'NONE',  ( 0.000000000000000000, -0.000000000000000000, 1.000000000000000000 ) ) ;
#62176 = CARTESIAN_POINT ( 'NONE',  ( 4.549999999999939426, 2.500000000000000000, -2.265063509461101798 ) ) ;
#62177 = CIRCLE ( 'NONE', #99828, 0.06509327318403745899 ) ;
#62178 = CONICAL_SURFACE ( 'NONE', #26570, 0.1000000000000000056, 0.003490658503988666988 ) ;
#62179 = EDGE_LOOP ( 'NONE', ( #67813, #77011 ) ) ;
#62180 = AXIS2_PLACEMENT_3D ( 'NONE', #11352, #51300, #110202 ) ;
#62181 = CIRCLE ( 'NONE', #122807, 0.1000000000000002554 ) ;
#62182 = LINE ( 'NONE', #11768, #71761 ) ;
#62183 = CARTESIAN_POINT ( 'NONE',  ( -3.950000000000025491, 2.500000000000000000, 6.048780366869521252 ) ) ;
#62184 = CARTESIAN_POINT ( 'NONE',  ( 6.249999999999967137, 2.500000000000000000, 6.595190528383296780 ) ) ;
#62185 = VERTEX_POINT ( 'NONE', #34988 ) ;
#62186 = EDGE_LOOP ( 'NONE', ( #34785, #9102, #6627, #101554 ) ) ;
#62187 = CONICAL_SURFACE ( 'NONE', #122812, 0.1000000000000002554, 0.003490658503988666988 ) ;
#62188 = DIRECTION ( 'NONE',  ( 0.000000000000000000, 1.000000000000000000, 0.000000000000000000 ) ) ;
#62189 = VERTEX_POINT ( 'NONE', #114802 ) ;
#62190 = CARTESIAN_POINT ( 'NONE',  ( -3.550000000000027356, 2.500000000000000000, 1.818653347947321475 ) ) ;
#62191 = DIRECTION ( 'NONE',  ( 0.000000000000000000, 0.000000000000000000, -1.000000000000000000 ) ) ;
#62192 = ADVANCED_FACE ( 'NONE', ( #128532 ), #85035, .T. ) ;
#62194 = VECTOR ( 'NONE', #22108, 1000.000000000000000 ) ;
#62193 = CONICAL_SURFACE ( 'NONE', #5722, 0.1000000000000002554, 0.003490658503988666988 ) ;
#62195 = DIRECTION ( 'NONE',  ( -0.000000000000000000, 1.000000000000000000, -0.000000000000000000 ) ) ;
#62196 = ORIENTED_EDGE ( 'NONE', *, *, #51964, .F. ) ;
#62198 = EDGE_CURVE ( 'NONE', #77843, #48167, #76924, .T. ) ;
#62197 = FACE_OUTER_BOUND ( 'NONE', #60240, .T. ) ;
#62199 = CARTESIAN_POINT ( 'NONE',  ( 2.899999999999946620, 2.500000000000000000, -3.537306695894649966 ) ) ;
#62200 = DIRECTION ( 'NONE',  ( -0.000000000000000000, 1.000000000000000000, -0.000000000000000000 ) ) ;
#62201 = CARTESIAN_POINT ( 'NONE',  ( -6.050000000000018474, 2.500000000000000000, 6.841600689897072485 ) ) ;
#62202 = DIRECTION ( 'NONE',  ( 0.000000000000000000, -0.000000000000000000, 1.000000000000000000 ) ) ;
#62203 = DIRECTION ( 'NONE',  ( 0.000000000000000000, 0.000000000000000000, 1.000000000000000000 ) ) ;
#62204 = EDGE_CURVE ( 'NONE', #21147, #107141, #9373, .T. ) ;
#62205 = ORIENTED_EDGE ( 'NONE', *, *, #35527, .F. ) ;
#62206 = ORIENTED_EDGE ( 'NONE', *, *, #73606, .T. ) ;
#62207 = DIRECTION ( 'NONE',  ( 0.000000000000000000, 0.000000000000000000, 1.000000000000000000 ) ) ;
#62208 = EDGE_LOOP ( 'NONE', ( #79427, #15626 ) ) ;
#62209 = CARTESIAN_POINT ( 'NONE',  ( -4.600000000000028066, 2.500000000000000000, -5.122947341949753763 ) ) ;
#62211 = ORIENTED_EDGE ( 'NONE', *, *, #114279, .F. ) ;
#62210 = EDGE_LOOP ( 'NONE', ( #79561, #9964, #54588, #113106 ) ) ;
#62212 = EDGE_LOOP ( 'NONE', ( #10745, #66791, #18458, #11480 ) ) ;
#62213 = AXIS2_PLACEMENT_3D ( 'NONE', #116684, #57783, #76127 ) ;
#62214 = LINE ( 'NONE', #102124, #45671 ) ;
#62215 = DIRECTION ( 'NONE',  ( 0.000000000000000000, 0.000000000000000000, -1.000000000000000000 ) ) ;
#62216 = CARTESIAN_POINT ( 'NONE',  ( -3.350000000000028511, 2.500000000000000000, 1.472243186433545459 ) ) ;
#62217 = DIRECTION ( 'NONE',  ( 0.000000000000000000, 1.000000000000000000, 0.000000000000000000 ) ) ;
#62218 = DIRECTION ( 'NONE',  ( 0.000000000000000000, 0.000000000000000000, -1.000000000000000000 ) ) ;
#62219 = CARTESIAN_POINT ( 'NONE',  ( 1.649999999999950617, 12.50000000000000000, 2.165063509461097713 ) ) ;
#62220 = DIRECTION ( 'NONE',  ( -0.000000000000000000, 1.000000000000000000, -0.000000000000000000 ) ) ;
#62221 = DIRECTION ( 'NONE',  ( 0.000000000000000000, 0.000000000000000000, 1.000000000000000000 ) ) ;
#62222 = LINE ( 'NONE', #32124, #127154 ) ;
#62224 = ORIENTED_EDGE ( 'NONE', *, *, #96213, .F. ) ;
#62223 = CIRCLE ( 'NONE', #93510, 0.06509327318403745899 ) ;
#62225 = LINE ( 'NONE', #110660, #107134 ) ;
#62226 = ORIENTED_EDGE ( 'NONE', *, *, #128982, .F. ) ;
#62227 = EDGE_LOOP ( 'NONE', ( #100015, #20446, #46802, #100315 ) ) ;
#62228 = CARTESIAN_POINT ( 'NONE',  ( -8.750000000000005329, 2.500000000000000000, 5.802370205355744659 ) ) ;
#62229 = CARTESIAN_POINT ( 'NONE',  ( 10.59999999999990905, 2.500000000000000000, -4.576537180435978236 ) ) ;
#62230 = LINE ( 'NONE', #111973, #23556 ) ;
#62231 = AXIS2_PLACEMENT_3D ( 'NONE', #60043, #119570, #99949 ) ;
#62232 = ADVANCED_FACE ( 'NONE', ( #38867 ), #37226, .T. ) ;
#62233 = DIRECTION ( 'NONE',  ( 0.000000000000000000, 1.000000000000000000, 0.000000000000000000 ) ) ;
#62234 = CIRCLE ( 'NONE', #35054, 0.06509327318403741736 ) ;
#62235 = AXIS2_PLACEMENT_3D ( 'NONE', #97753, #98384, #127232 ) ;
#62236 = FACE_OUTER_BOUND ( 'NONE', #87564, .T. ) ;
#62237 = DIRECTION ( 'NONE',  ( 0.000000000000000000, -0.000000000000000000, 1.000000000000000000 ) ) ;
#62238 = PLANE ( 'NONE',  #65605 ) ;
#62239 = ORIENTED_EDGE ( 'NONE', *, *, #110717, .T. ) ;
#62240 = EDGE_LOOP ( 'NONE', ( #103468, #80156 ) ) ;
#62241 = VECTOR ( 'NONE', #90979, 1000.000000000000000 ) ;
#62242 = VERTEX_POINT ( 'NONE', #129175 ) ;
#62243 = ORIENTED_EDGE ( 'NONE', *, *, #93773, .F. ) ;
#62244 = EDGE_CURVE ( 'NONE', #35299, #14887, #57836, .T. ) ;
#62245 = CIRCLE ( 'NONE', #72701, 0.1000000000000000472 ) ;
#62247 = ORIENTED_EDGE ( 'NONE', *, *, #70691, .T. ) ;
#62246 = EDGE_CURVE ( 'NONE', #74354, #115572, #93368, .T. ) ;
#62248 = DIRECTION ( 'NONE',  ( 0.000000000000000000, 0.000000000000000000, 1.000000000000000000 ) ) ;
#62249 = FACE_OUTER_BOUND ( 'NONE', #679, .T. ) ;
#62250 = CIRCLE ( 'NONE', #81122, 0.06509327318403745899 ) ;
#62251 = DIRECTION ( 'NONE',  ( 0.000000000000000000, 0.000000000000000000, 1.000000000000000000 ) ) ;
#62252 = DIRECTION ( 'NONE',  ( -0.000000000000000000, -1.000000000000000000, -0.000000000000000000 ) ) ;
#62253 = CIRCLE ( 'NONE', #87269, 0.09999999999999982514 ) ;
#62254 = DIRECTION ( 'NONE',  ( 0.000000000000000000, 0.000000000000000000, 1.000000000000000000 ) ) ;
#62255 = VERTEX_POINT ( 'NONE', #49965 ) ;
#62256 = DIRECTION ( 'NONE',  ( 0.000000000000000000, 1.000000000000000000, 0.000000000000000000 ) ) ;
#62257 = CARTESIAN_POINT ( 'NONE',  ( 0.6499999999999566125, 12.50000000000000000, -6.841600689897077814 ) ) ;
#62258 = EDGE_CURVE ( 'NONE', #113976, #108759, #30321, .T. ) ;
#62259 = DIRECTION ( 'NONE',  ( 0.000000000000000000, 1.000000000000000000, 0.000000000000000000 ) ) ;
#62260 = PLANE ( 'NONE',  #20082 ) ;
#62261 = CIRCLE ( 'NONE', #41339, 0.09999999999999982514 ) ;
#62262 = AXIS2_PLACEMENT_3D ( 'NONE', #119573, #127483, #28642 ) ;
#62263 = CARTESIAN_POINT ( 'NONE',  ( -7.950000000000012612, 2.500000000000000000, -2.165063509461101710 ) ) ;
#62264 = ORIENTED_EDGE ( 'NONE', *, *, #2582, .F. ) ;
#62265 = CIRCLE ( 'NONE', #87364, 0.09999999999999982514 ) ;
#62266 = ORIENTED_EDGE ( 'NONE', *, *, #18080, .F. ) ;
#62267 = ORIENTED_EDGE ( 'NONE', *, *, #50132, .F. ) ;
#62268 = DIRECTION ( 'NONE',  ( 0.000000000000000000, 0.000000000000000000, -1.000000000000000000 ) ) ;
#62269 = VERTEX_POINT ( 'NONE', #29658 ) ;
#62270 = CARTESIAN_POINT ( 'NONE',  ( 9.399999999999915090, 2.500000000000000000, 4.676537180435972552 ) ) ;
#62271 = DIRECTION ( 'NONE',  ( 0.000000000000000000, 0.000000000000000000, 1.000000000000000000 ) ) ;
#62272 = AXIS2_PLACEMENT_3D ( 'NONE', #50355, #90258, #90927 ) ;
#62273 = ORIENTED_EDGE ( 'NONE', *, *, #114910, .F. ) ;
#62274 = LINE ( 'NONE', #72730, #43272 ) ;
#62276 = AXIS2_PLACEMENT_3D ( 'NONE', #9563, #48854, #99238 ) ;
#62275 = CARTESIAN_POINT ( 'NONE',  ( -13.54999999999999005, 2.500000000000000000, 2.411473670974877415 ) ) ;
#62277 = CARTESIAN_POINT ( 'NONE',  ( -0.8500000000000382805, 2.500000000000000000, -1.472243186433550122 ) ) ;
#62278 = DIRECTION ( 'NONE',  ( 0.000000000000000000, 1.000000000000000000, 0.000000000000000000 ) ) ;
#62279 = EDGE_CURVE ( 'NONE', #76856, #44317, #27708, .T. ) ;
#62281 = VECTOR ( 'NONE', #109676, 1000.000000000000000 ) ;
#62280 = CIRCLE ( 'NONE', #1618, 1.388921157871087386 ) ;
#62282 = LINE ( 'NONE', #110082, #16344 ) ;
#62283 = EDGE_LOOP ( 'NONE', ( #96744, #27088 ) ) ;
#62284 = ORIENTED_EDGE ( 'NONE', *, *, #60380, .F. ) ;
#62285 = EDGE_CURVE ( 'NONE', #103089, #124700, #66163, .T. ) ;
#62286 = CARTESIAN_POINT ( 'NONE',  ( 187.0416666666666572, -4.445597072760107515, 7.700000000000023270 ) ) ;
#62287 = LINE ( 'NONE', #101559, #7971 ) ;
#62288 = EDGE_CURVE ( 'NONE', #118069, #125289, #70659, .T. ) ;
#62289 = CARTESIAN_POINT ( 'NONE',  ( 6.899999999999926636, 2.500000000000000000, 0.2464101615137736789 ) ) ;
#62290 = CARTESIAN_POINT ( 'NONE',  ( 3.299999999999944755, 2.500000000000000000, -2.385244779468109755E-15 ) ) ;
#62291 = ORIENTED_EDGE ( 'NONE', *, *, #94664, .T. ) ;
#62292 = EDGE_CURVE ( 'NONE', #54553, #128976, #57870, .T. ) ;
#62293 = EDGE_CURVE ( 'NONE', #109985, #9468, #110087, .T. ) ;
#62294 = EDGE_LOOP ( 'NONE', ( #38280, #108540, #26447, #21226 ) ) ;
#62295 = DIRECTION ( 'NONE',  ( -0.000000000000000000, -1.000000000000000000, -0.000000000000000000 ) ) ;
#62296 = DIRECTION ( 'NONE',  ( -0.000000000000000000, -1.000000000000000000, -0.000000000000000000 ) ) ;
#62297 = EDGE_CURVE ( 'NONE', #2356, #3164, #87372, .T. ) ;
#62298 = CARTESIAN_POINT ( 'NONE',  ( 5.399999999999934630, 12.50000000000000000, 0.6928203230275494784 ) ) ;
#62299 = CARTESIAN_POINT ( 'NONE',  ( -1.450000000000035483, 2.500000000000000000, 6.148780366869520897 ) ) ;
#62300 = EDGE_LOOP ( 'NONE', ( #109905, #61537, #21763, #38476 ) ) ;
#62301 = CARTESIAN_POINT ( 'NONE',  ( 1.249999999999954259, 12.50000000000000000, -7.188010851410854052 ) ) ;
#62302 = ADVANCED_FACE ( 'NONE', ( #87273 ), #9743, .T. ) ;
#62303 = DIRECTION ( 'NONE',  ( 0.000000000000000000, 0.000000000000000000, 1.000000000000000000 ) ) ;
#62304 = VERTEX_POINT ( 'NONE', #19164 ) ;
#62305 = VECTOR ( 'NONE', #124798, 1000.000000000000000 ) ;
#62306 = FACE_OUTER_BOUND ( 'NONE', #123508, .T. ) ;
#62307 = ORIENTED_EDGE ( 'NONE', *, *, #17046, .T. ) ;
#62308 = EDGE_CURVE ( 'NONE', #90957, #70171, #80044, .T. ) ;
#62309 = PLANE ( 'NONE',  #116450 ) ;
#62310 = AXIS2_PLACEMENT_3D ( 'NONE', #51276, #52543, #11964 ) ;
#62311 = VECTOR ( 'NONE', #100264, 1000.000000000000000 ) ;
#62312 = ORIENTED_EDGE ( 'NONE', *, *, #67373, .T. ) ;
#62313 = CARTESIAN_POINT ( 'NONE',  ( -4.150000000000027889, 2.500000000000000000, -6.595190528383302109 ) ) ;
#62314 = DIRECTION ( 'NONE',  ( -0.000000000000000000, -1.000000000000000000, -0.000000000000000000 ) ) ;
#62315 = EDGE_LOOP ( 'NONE', ( #105320, #56670, #33215, #80030 ) ) ;
#62316 = ORIENTED_EDGE ( 'NONE', *, *, #38797, .T. ) ;
#62317 = CARTESIAN_POINT ( 'NONE',  ( 187.3802083336747444, 4.367472073101515306, 7.564683531250000925 ) ) ;
#62318 = CARTESIAN_POINT ( 'NONE',  ( 127.5000000000000000, 2.000000000000000000, -4.999999999999998224 ) ) ;
#62319 = CARTESIAN_POINT ( 'NONE',  ( -6.250000000000015987, 2.500000000000000000, 1.572243186433545548 ) ) ;
#62320 = CARTESIAN_POINT ( 'NONE',  ( 184.2343750003414016, 8.734944146203032389, 5.348610694689227483E-16 ) ) ;
#62321 = AXIS2_PLACEMENT_3D ( 'NONE', #53701, #93631, #81237 ) ;
#62322 = DIRECTION ( 'NONE',  ( 0.000000000000000000, 1.000000000000000000, 0.000000000000000000 ) ) ;
#62323 = CARTESIAN_POINT ( 'NONE',  ( -0.4000000000000401013, 2.500000000000000000, -3.637306695894650055 ) ) ;
#62324 = DIRECTION ( 'NONE',  ( -0.000000000000000000, -1.000000000000000000, -0.000000000000000000 ) ) ;
#62325 = DIRECTION ( 'NONE',  ( -0.000000000000000000, -1.000000000000000000, -0.000000000000000000 ) ) ;
#62326 = DIRECTION ( 'NONE',  ( -4.274815082592931898E-19, -0.9999939076577903929, -0.003490651415223739937 ) ) ;
#62327 = CIRCLE ( 'NONE', #22630, 0.06509327318403745899 ) ;
#62328 = EDGE_LOOP ( 'NONE', ( #9361, #22450, #104996, #83043 ) ) ;
#62329 = EDGE_LOOP ( 'NONE', ( #117064, #108163, #62751, #91223 ) ) ;
#62330 = CARTESIAN_POINT ( 'NONE',  ( 8.149999999999920419, 2.500000000000000000, -1.818653347947325916 ) ) ;
#62331 = ORIENTED_EDGE ( 'NONE', *, *, #6500, .T. ) ;
#62332 = DIRECTION ( 'NONE',  ( 0.000000000000000000, -0.000000000000000000, 1.000000000000000000 ) ) ;
#62333 = FACE_OUTER_BOUND ( 'NONE', #64605, .T. ) ;
#62334 = CONICAL_SURFACE ( 'NONE', #106149, 0.1000000000000002554, 0.003490658503988666988 ) ;
#62335 = PLANE ( 'NONE',  #3065 ) ;
#62337 = ORIENTED_EDGE ( 'NONE', *, *, #77041, .T. ) ;
#62336 = VERTEX_POINT ( 'NONE', #37554 ) ;
#62338 = FACE_BOUND ( 'NONE', #30976, .T. ) ;
#62339 = ORIENTED_EDGE ( 'NONE', *, *, #56009, .T. ) ;
#62340 = CARTESIAN_POINT ( 'NONE',  ( -2.499999999999996003, 12.50000000000000000, 0.06509327318403515528 ) ) ;
#62341 = DIRECTION ( 'NONE',  ( -0.000000000000000000, -1.000000000000000000, -0.000000000000000000 ) ) ;
#62342 = DIRECTION ( 'NONE',  ( 0.000000000000000000, 0.000000000000000000, 1.000000000000000000 ) ) ;
#62343 = VECTOR ( 'NONE', #102626, 1000.000000000000000 ) ;
#62344 = DIRECTION ( 'NONE',  ( 0.000000000000000000, 1.000000000000000000, 0.000000000000000000 ) ) ;
#62345 = ADVANCED_FACE ( 'NONE', ( #127852 ), #99044, .T. ) ;
#62346 = LINE ( 'NONE', #100331, #82679 ) ;
#62347 = CARTESIAN_POINT ( 'NONE',  ( -13.29999999999999005, 2.500000000000000000, -4.330127018922198978 ) ) ;
#62348 = DIRECTION ( 'NONE',  ( 0.000000000000000000, 0.000000000000000000, -1.000000000000000000 ) ) ;
#62349 = DIRECTION ( 'NONE',  ( -0.000000000000000000, 1.000000000000000000, -0.000000000000000000 ) ) ;
#62350 = CARTESIAN_POINT ( 'NONE',  ( 10.84999999999990905, 2.500000000000000000, -5.802370205355749988 ) ) ;
#62351 = CARTESIAN_POINT ( 'NONE',  ( -4.076600168545496672E-14, 2.500000000000000000, -4.922947341949753586 ) ) ;
#62352 = AXIS2_PLACEMENT_3D ( 'NONE', #113381, #121925, #102915 ) ;
#62353 = AXIS2_PLACEMENT_3D ( 'NONE', #81825, #92292, #53666 ) ;
#62354 = CARTESIAN_POINT ( 'NONE',  ( -1.250000000000001554, 12.50000000000000000, 6.495190528383297135 ) ) ;
#62355 = EDGE_CURVE ( 'NONE', #2098, #51142, #82911, .T. ) ;
#62356 = ORIENTED_EDGE ( 'NONE', *, *, #103788, .T. ) ;
#62358 = ORIENTED_EDGE ( 'NONE', *, *, #76516, .T. ) ;
#62357 = AXIS2_PLACEMENT_3D ( 'NONE', #101551, #110710, #100887 ) ;
#62359 = VERTEX_POINT ( 'NONE', #18541 ) ;
#62360 = DIRECTION ( 'NONE',  ( 0.000000000000000000, 0.000000000000000000, 1.000000000000000000 ) ) ;
#62361 = VERTEX_POINT ( 'NONE', #58493 ) ;
#62362 = DIRECTION ( 'NONE',  ( -4.274815082592931898E-19, -0.9999939076577903929, -0.003490651415223739937 ) ) ;
#62363 = PLANE ( 'NONE',  #31990 ) ;
#62365 = EDGE_LOOP ( 'NONE', ( #63350, #28789 ) ) ;
#62364 = ORIENTED_EDGE ( 'NONE', *, *, #10416, .F. ) ;
#62367 = ORIENTED_EDGE ( 'NONE', *, *, #30077, .T. ) ;
#62366 = AXIS2_PLACEMENT_3D ( 'NONE', #2764, #32896, #63633 ) ;
#62368 = CARTESIAN_POINT ( 'NONE',  ( -13.09999999999999254, 12.50000000000000000, -0.3464101615137741286 ) ) ;
#62369 = PLANE ( 'NONE',  #27948 ) ;
#62370 = DIRECTION ( 'NONE',  ( 0.000000000000000000, 1.000000000000000000, 0.000000000000000000 ) ) ;
#62371 = CARTESIAN_POINT ( 'NONE',  ( -9.150000000000005684, 2.500000000000000000, 5.802370205355744659 ) ) ;
#62372 = FACE_OUTER_BOUND ( 'NONE', #105050, .T. ) ;
#62373 = CARTESIAN_POINT ( 'NONE',  ( -2.300000000000033573, 12.50000000000000000, -4.048810130592463530 ) ) ;
#62374 = VECTOR ( 'NONE', #43326, 1000.000000000000000 ) ;
#62375 = VERTEX_POINT ( 'NONE', #48657 ) ;
#62376 = CARTESIAN_POINT ( 'NONE',  ( -7.300000000000014921, 12.50000000000000000, 4.741630453620009789 ) ) ;
#62377 = ORIENTED_EDGE ( 'NONE', *, *, #85925, .T. ) ;
#62379 = AXIS2_PLACEMENT_3D ( 'NONE', #91732, #123131, #92364 ) ;
#62378 = CIRCLE ( 'NONE', #16358, 0.1000000000000002554 ) ;
#62380 = VERTEX_POINT ( 'NONE', #40791 ) ;
#62381 = VERTEX_POINT ( 'NONE', #80702 ) ;
#62382 = CARTESIAN_POINT ( 'NONE',  ( -6.650000000000019007, 2.500000000000000000, -5.802370205355749988 ) ) ;
#62383 = VERTEX_POINT ( 'NONE', #93099 ) ;
#62384 = VERTEX_POINT ( 'NONE', #41431 ) ;
#62385 = ORIENTED_EDGE ( 'NONE', *, *, #29183, .T. ) ;
#62386 = EDGE_CURVE ( 'NONE', #4792, #121198, #24412, .T. ) ;
#62387 = FILL_AREA_STYLE_COLOUR ( '', #49771 ) ;
#62388 = CARTESIAN_POINT ( 'NONE',  ( -5.000000000000023093, 12.50000000000000000, 0.6928203230275494784 ) ) ;
#62389 = CARTESIAN_POINT ( 'NONE',  ( 7.049999999999928768, 2.500000000000000000, 6.595190528383296780 ) ) ;
#62390 = CARTESIAN_POINT ( 'NONE',  ( 10.59999999999990905, 12.50000000000000000, 3.983716857408420076 ) ) ;
#62392 = AXIS2_PLACEMENT_3D ( 'NONE', #82455, #122371, #53622 ) ;
#62391 = DIRECTION ( 'NONE',  ( 0.000000000000000000, 1.000000000000000000, 0.000000000000000000 ) ) ;
#62393 = FACE_OUTER_BOUND ( 'NONE', #2685, .T. ) ;
#62394 = ADVANCED_FACE ( 'NONE', ( #43360 ), #45443, .T. ) ;
#62395 = EDGE_LOOP ( 'NONE', ( #101044, #70027, #76927, #44006 ) ) ;
#62397 = DIRECTION ( 'NONE',  ( 0.000000000000000000, 1.000000000000000000, 0.000000000000000000 ) ) ;
#62396 = AXIS2_PLACEMENT_3D ( 'NONE', #122469, #22975, #63541 ) ;
#62399 = ORIENTED_EDGE ( 'NONE', *, *, #115326, .F. ) ;
#62398 = AXIS2_PLACEMENT_3D ( 'NONE', #42934, #82846, #33106 ) ;
#62400 = FACE_OUTER_BOUND ( 'NONE', #69155, .T. ) ;
#62401 = CONICAL_SURFACE ( 'NONE', #37266, 0.1000000000000000472, 0.003490658503988666988 ) ;
#62402 = ORIENTED_EDGE ( 'NONE', *, *, #106786, .T. ) ;
#62404 = ADVANCED_FACE ( 'NONE', ( #120615 ), #85128, .T. ) ;
#62403 = DIRECTION ( 'NONE',  ( 0.000000000000000000, -0.000000000000000000, 1.000000000000000000 ) ) ;
#62405 = EDGE_CURVE ( 'NONE', #61045, #79468, #93460, .T. ) ;
#62406 = VERTEX_POINT ( 'NONE', #71505 ) ;
#62407 = CIRCLE ( 'NONE', #10163, 0.1000000000000000472 ) ;
#62408 = LINE ( 'NONE', #61765, #65256 ) ;
#62409 = AXIS2_PLACEMENT_3D ( 'NONE', #71364, #90361, #72677 ) ;
#62410 = AXIS2_PLACEMENT_3D ( 'NONE', #73787, #101334, #101975 ) ;
#62411 = ADVANCED_FACE ( 'NONE', ( #121258 ), #87181, .T. ) ;
#62412 = DIRECTION ( 'NONE',  ( 0.000000000000000000, 1.000000000000000000, 0.000000000000000000 ) ) ;
#62413 = ORIENTED_EDGE ( 'NONE', *, *, #50023, .F. ) ;
#62414 = ORIENTED_EDGE ( 'NONE', *, *, #67717, .F. ) ;
#62415 = FACE_OUTER_BOUND ( 'NONE', #61475, .T. ) ;
#62416 = CARTESIAN_POINT ( 'NONE',  ( 3.949999999999940670, 2.500000000000000000, 1.718653347947321386 ) ) ;
#62417 = ADVANCED_FACE ( 'NONE', ( #73432 ), #66260, .T. ) ;
#62418 = CARTESIAN_POINT ( 'NONE',  ( 4.599999999999935696, 2.500000000000000000, 5.022947341949748790 ) ) ;
#62419 = CARTESIAN_POINT ( 'NONE',  ( -0.4000000000000392131, 2.500000000000000000, -4.922947341949753586 ) ) ;
#62420 = VECTOR ( 'NONE', #18166, 1000.000000000000000 ) ;
#62421 = FACE_OUTER_BOUND ( 'NONE', #114859, .T. ) ;
#62422 = CIRCLE ( 'NONE', #70804, 0.1000000000000002554 ) ;
#62423 = ORIENTED_EDGE ( 'NONE', *, *, #4481, .F. ) ;
#62424 = CARTESIAN_POINT ( 'NONE',  ( 9.149999999999915090, 2.500000000000000000, -2.165063509461101710 ) ) ;
#62425 = ORIENTED_EDGE ( 'NONE', *, *, #8310, .T. ) ;
#62426 = CARTESIAN_POINT ( 'NONE',  ( -9.350000000000008527, 12.50000000000000000, -6.906693963081109722 ) ) ;
#62428 = CIRCLE ( 'NONE', #93706, 0.1000000000000002554 ) ;
#62427 = DIRECTION ( 'NONE',  ( 0.000000000000000000, 0.000000000000000000, 1.000000000000000000 ) ) ;
#62429 = ADVANCED_FACE ( 'NONE', ( #11939 ), #108119, .T. ) ;
#62430 = AXIS2_PLACEMENT_3D ( 'NONE', #76826, #28374, #8070 ) ;
#62431 = VECTOR ( 'NONE', #56432, 1000.000000000000000 ) ;
#62432 = DIRECTION ( 'NONE',  ( -0.000000000000000000, 1.000000000000000000, -0.000000000000000000 ) ) ;
#62433 = DIRECTION ( 'NONE',  ( 0.000000000000000000, 0.000000000000000000, 1.000000000000000000 ) ) ;
#62434 = DIRECTION ( 'NONE',  ( 0.000000000000000000, 1.000000000000000000, 0.000000000000000000 ) ) ;
#62435 = DIRECTION ( 'NONE',  ( -0.000000000000000000, 1.000000000000000000, -0.000000000000000000 ) ) ;
#62436 = DIRECTION ( 'NONE',  ( 0.000000000000000000, 0.000000000000000000, -1.000000000000000000 ) ) ;
#62437 = ORIENTED_EDGE ( 'NONE', *, *, #106164, .T. ) ;
#62438 = CARTESIAN_POINT ( 'NONE',  ( 3.299999999999944755, 2.500000000000000000, -4.330127018922201643 ) ) ;
#62439 = EDGE_CURVE ( 'NONE', #22140, #27344, #112244, .T. ) ;
#62440 = DIRECTION ( 'NONE',  ( 0.000000000000000000, -0.9999939076577903929, 0.003490651415223739937 ) ) ;
#62441 = DIRECTION ( 'NONE',  ( 0.000000000000000000, -0.000000000000000000, 1.000000000000000000 ) ) ;
#62442 = ORIENTED_EDGE ( 'NONE', *, *, #52939, .T. ) ;
#62443 = ORIENTED_EDGE ( 'NONE', *, *, #8294, .F. ) ;
#62444 = AXIS2_PLACEMENT_3D ( 'NONE', #110338, #20678, #50777 ) ;
#62445 = EDGE_CURVE ( 'NONE', #49778, #26094, #14017, .T. ) ;
#62446 = DIRECTION ( 'NONE',  ( 0.000000000000000000, 1.000000000000000000, 0.000000000000000000 ) ) ;
#62447 = CIRCLE ( 'NONE', #104292, 0.06509327318403745899 ) ;
#62448 = VERTEX_POINT ( 'NONE', #42059 ) ;
#62449 = ORIENTED_EDGE ( 'NONE', *, *, #54661, .F. ) ;
#62450 = DIRECTION ( 'NONE',  ( 0.000000000000000000, 1.000000000000000000, 0.000000000000000000 ) ) ;
#62451 = EDGE_CURVE ( 'NONE', #63624, #93574, #110782, .T. ) ;
#62452 = ORIENTED_EDGE ( 'NONE', *, *, #78735, .F. ) ;
#62454 = AXIS2_PLACEMENT_3D ( 'NONE', #37390, #115258, #87111 ) ;
#62453 = CARTESIAN_POINT ( 'NONE',  ( 20.06694580393454785, -2.635910463901357303, -2.269534205241988456 ) ) ;
#62455 = DIRECTION ( 'NONE',  ( -0.000000000000000000, -1.000000000000000000, -0.000000000000000000 ) ) ;
#62456 = ADVANCED_FACE ( 'NONE', ( #61709 ), #53175, .T. ) ;
#62457 = CARTESIAN_POINT ( 'NONE',  ( 16.68526679984121586, 0.4774970013478979647, 5.954360761637129684 ) ) ;
#62458 = EDGE_CURVE ( 'NONE', #125340, #3331, #32833, .T. ) ;
#62459 = EDGE_LOOP ( 'NONE', ( #85258, #7808, #29762, #45050 ) ) ;
#62460 = DIRECTION ( 'NONE',  ( 0.000000000000000000, 1.000000000000000000, 0.000000000000000000 ) ) ;
#62462 = EDGE_CURVE ( 'NONE', #37733, #85672, #100335, .T. ) ;
#62461 = CIRCLE ( 'NONE', #110556, 0.06509327318403745899 ) ;
#62463 = DIRECTION ( 'NONE',  ( 0.000000000000000000, 0.000000000000000000, 1.000000000000000000 ) ) ;
#62464 = CIRCLE ( 'NONE', #104304, 0.1000000000000000472 ) ;
#62465 = ORIENTED_EDGE ( 'NONE', *, *, #88354, .F. ) ;
#62466 = ADVANCED_FACE ( 'NONE', ( #122557 ), #72809, .T. ) ;
#62469 = EDGE_CURVE ( 'NONE', #55655, #47265, #89252, .T. ) ;
#62468 = VECTOR ( 'NONE', #72579, 1000.000000000000000 ) ;
#62467 = CIRCLE ( 'NONE', #112633, 0.06509327318403745899 ) ;
#62470 = ORIENTED_EDGE ( 'NONE', *, *, #92554, .F. ) ;
#62471 = ORIENTED_EDGE ( 'NONE', *, *, #77809, .T. ) ;
#62472 = CARTESIAN_POINT ( 'NONE',  ( -2.900000000000030109, 2.500000000000000000, -3.537306695894649966 ) ) ;
#62473 = DIRECTION ( 'NONE',  ( 0.000000000000000000, 0.000000000000000000, 1.000000000000000000 ) ) ;
#62474 = DIRECTION ( 'NONE',  ( 0.000000000000000000, 0.000000000000000000, 1.000000000000000000 ) ) ;
#62475 = FACE_BOUND ( 'NONE', #108930, .T. ) ;
#62476 = ORIENTED_EDGE ( 'NONE', *, *, #43414, .F. ) ;
#62477 = PLANE ( 'NONE',  #4914 ) ;
#62478 = DIRECTION ( 'NONE',  ( -0.000000000000000000, 1.000000000000000000, -0.000000000000000000 ) ) ;
#62479 = ORIENTED_EDGE ( 'NONE', *, *, #18656, .F. ) ;
#62480 = DIRECTION ( 'NONE',  ( 0.000000000000000000, 1.000000000000000000, 0.000000000000000000 ) ) ;
#62481 = FACE_OUTER_BOUND ( 'NONE', #16896, .T. ) ;
#62482 = CARTESIAN_POINT ( 'NONE',  ( 179.5000000000000000, 1.375000000000000000, 7.576237522675751457 ) ) ;
#62483 = CARTESIAN_POINT ( 'NONE',  ( 2.500000000000002220, -1.500000000000000000, 10.00000000000000178 ) ) ;
#62484 = VECTOR ( 'NONE', #63122, 1000.000000000000000 ) ;
#62485 = DIRECTION ( 'NONE',  ( 0.000000000000000000, 0.000000000000000000, 1.000000000000000000 ) ) ;
#62486 = PLANE ( 'NONE',  #116160 ) ;
#62487 = CARTESIAN_POINT ( 'NONE',  ( 3.749999999999942268, 2.500000000000000000, 1.472243186433545459 ) ) ;
#62488 = CIRCLE ( 'NONE', #43718, 0.5000000000000000000 ) ;
#62489 = AXIS2_PLACEMENT_3D ( 'NONE', #3308, #18598, #43253 ) ;
#62490 = ORIENTED_EDGE ( 'NONE', *, *, #10660, .F. ) ;
#62491 = EDGE_LOOP ( 'NONE', ( #36284, #109493, #103550, #77758 ) ) ;
#62492 = AXIS2_PLACEMENT_3D ( 'NONE', #103261, #113063, #81676 ) ;
#62493 = EDGE_LOOP ( 'NONE', ( #125464, #58674, #70131, #83537 ) ) ;
#62494 = VERTEX_POINT ( 'NONE', #1471 ) ;
#62495 = PLANE ( 'NONE',  #22354 ) ;
#62496 = DIRECTION ( 'NONE',  ( 0.000000000000000000, 0.000000000000000000, -1.000000000000000000 ) ) ;
#62497 = DIRECTION ( 'NONE',  ( 0.000000000000000000, -0.9999939076577903929, 0.003490651415223739937 ) ) ;
#62498 = ORIENTED_EDGE ( 'NONE', *, *, #28908, .T. ) ;
#62499 = FACE_BOUND ( 'NONE', #78051, .T. ) ;
#62500 = DIRECTION ( 'NONE',  ( 0.000000000000000000, 1.000000000000000000, 0.000000000000000000 ) ) ;
#62501 = DIRECTION ( 'NONE',  ( 0.000000000000000000, 0.000000000000000000, 1.000000000000000000 ) ) ;
#62502 = AXIS2_PLACEMENT_3D ( 'NONE', #36971, #76893, #28443 ) ;
#62503 = AXIS2_PLACEMENT_3D ( 'NONE', #55607, #115137, #75887 ) ;
#62504 = PLANE ( 'NONE',  #72145 ) ;
#62505 = AXIS2_PLACEMENT_3D ( 'NONE', #84902, #126114, #44327 ) ;
#62506 = LINE ( 'NONE', #32414, #51185 ) ;
#62507 = CARTESIAN_POINT ( 'NONE',  ( 5.849999999999933920, 12.50000000000000000, -2.857883832488653741 ) ) ;
#62508 = CARTESIAN_POINT ( 'NONE',  ( -9.550000000000006040, 2.500000000000000000, 2.165063509461097713 ) ) ;
#62509 = CARTESIAN_POINT ( 'NONE',  ( -5.850000000000018296, 2.500000000000000000, 5.902370205355745192 ) ) ;
#62510 = DIRECTION ( 'NONE',  ( 0.000000000000000000, 1.000000000000000000, 0.000000000000000000 ) ) ;
#62511 = DIRECTION ( 'NONE',  ( 0.000000000000000000, 1.000000000000000000, 0.000000000000000000 ) ) ;
#62512 = AXIS2_PLACEMENT_3D ( 'NONE', #35100, #75011, #54079 ) ;
#62513 = ORIENTED_EDGE ( 'NONE', *, *, #83683, .T. ) ;
#62514 = EDGE_CURVE ( 'NONE', #108066, #121486, #111418, .T. ) ;
#62515 = ORIENTED_EDGE ( 'NONE', *, *, #19166, .F. ) ;
#62516 = VERTEX_POINT ( 'NONE', #54439 ) ;
#62517 = VERTEX_POINT ( 'NONE', #76020 ) ;
#62518 = VERTEX_POINT ( 'NONE', #115946 ) ;
#62519 = ORIENTED_EDGE ( 'NONE', *, *, #99724, .T. ) ;
#62520 = PLANE ( 'NONE',  #77738 ) ;
#62521 = EDGE_LOOP ( 'NONE', ( #47132, #114901, #102234, #86280 ) ) ;
#62522 = EDGE_LOOP ( 'NONE', ( #1631, #128890 ) ) ;
#62523 = CIRCLE ( 'NONE', #6051, 0.1000000000000000056 ) ;
#62524 = CARTESIAN_POINT ( 'NONE',  ( 127.5000000000000000, 1.500000000000000000, 6.000000000000000000 ) ) ;
#62525 = CARTESIAN_POINT ( 'NONE',  ( 14.66596006039096522, -2.499999999999999556, 7.515560524215777249 ) ) ;
#62526 = DIRECTION ( 'NONE',  ( -0.000000000000000000, 1.000000000000000000, -0.000000000000000000 ) ) ;
#62527 = CARTESIAN_POINT ( 'NONE',  ( -12.89999999999999147, 2.500000000000000000, -4.230127018922199333 ) ) ;
#62528 = CIRCLE ( 'NONE', #79241, 0.06509327318403745899 ) ;
#62529 = VERTEX_POINT ( 'NONE', #105491 ) ;
#62530 = DIRECTION ( 'NONE',  ( 0.000000000000000000, 0.000000000000000000, -1.000000000000000000 ) ) ;
#62531 = ORIENTED_EDGE ( 'NONE', *, *, #82969, .T. ) ;
#62532 = ORIENTED_EDGE ( 'NONE', *, *, #87247, .F. ) ;
#62533 = VECTOR ( 'NONE', #21329, 1000.000000000000000 ) ;
#62534 = DIRECTION ( 'NONE',  ( 0.000000000000000000, -0.000000000000000000, 1.000000000000000000 ) ) ;
#62535 = CARTESIAN_POINT ( 'NONE',  ( -6.249999999999984901, 2.500000000000000000, -6.495190528383302464 ) ) ;
#62536 = ORIENTED_EDGE ( 'NONE', *, *, #123113, .F. ) ;
#62537 = VECTOR ( 'NONE', #95858, 1000.000000000000000 ) ;
#62538 = ORIENTED_EDGE ( 'NONE', *, *, #66993, .F. ) ;
#62539 = DIRECTION ( 'NONE',  ( -0.000000000000000000, -1.000000000000000000, -0.000000000000000000 ) ) ;
#62540 = VECTOR ( 'NONE', #99475, 1000.000000000000000 ) ;
#62541 = DIRECTION ( 'NONE',  ( -4.274815082592931898E-19, -0.9999939076577903929, -0.003490651415223739937 ) ) ;
#62542 = CARTESIAN_POINT ( 'NONE',  ( 8.349999999999923261, 2.500000000000000000, -6.595190528383302109 ) ) ;
#62543 = LINE ( 'NONE', #40979, #79624 ) ;
#62544 = DIRECTION ( 'NONE',  ( -0.000000000000000000, 1.000000000000000000, -0.000000000000000000 ) ) ;
#62545 = AXIS2_PLACEMENT_3D ( 'NONE', #83453, #123361, #15319 ) ;
#62546 = VERTEX_POINT ( 'NONE', #16428 ) ;
#62547 = CARTESIAN_POINT ( 'NONE',  ( 15.40585131959743848, -2.500000000000000000, 5.817868759122586830 ) ) ;
#62548 = ADVANCED_FACE ( 'NONE', ( #55735 ), #126912, .T. ) ;
#62549 = ORIENTED_EDGE ( 'NONE', *, *, #41212, .T. ) ;
#62550 = CARTESIAN_POINT ( 'NONE',  ( 17.50000000000000000, 2.499999999999999556, -1.333333333333329929 ) ) ;
#62552 = AXIS2_PLACEMENT_3D ( 'NONE', #108487, #117002, #47650 ) ;
#62551 = VECTOR ( 'NONE', #18453, 1000.000000000000000 ) ;
#62553 = DIRECTION ( 'NONE',  ( 0.000000000000000000, 0.000000000000000000, -1.000000000000000000 ) ) ;
#62554 = DIRECTION ( 'NONE',  ( 0.000000000000000000, 0.000000000000000000, 1.000000000000000000 ) ) ;
#62556 = EDGE_CURVE ( 'NONE', #98451, #4284, #97657, .T. ) ;
#62555 = FACE_OUTER_BOUND ( 'NONE', #116515, .T. ) ;
#62557 = CARTESIAN_POINT ( 'NONE',  ( -13.74999999999995381, 2.500000000000000000, 2.265063509461101354 ) ) ;
#62558 = ADVANCED_FACE ( 'NONE', ( #124486 ), #41245, .T. ) ;
#62559 = ORIENTED_EDGE ( 'NONE', *, *, #124463, .F. ) ;
#62560 = DIRECTION ( 'NONE',  ( 0.000000000000000000, 0.000000000000000000, -1.000000000000000000 ) ) ;
#62562 = VECTOR ( 'NONE', #94617, 1000.000000000000000 ) ;
#62561 = AXIS2_PLACEMENT_3D ( 'NONE', #75736, #123544, #115659 ) ;
#62563 = ADVANCED_FACE ( 'NONE', ( #26288 ), #49556, .T. ) ;
#62564 = PLANE ( 'NONE',  #111469 ) ;
#62565 = VERTEX_POINT ( 'NONE', #44632 ) ;
#62566 = ADVANCED_FACE ( 'NONE', ( #34178 ), #83011, .T. ) ;
#62567 = EDGE_LOOP ( 'NONE', ( #41, #65889 ) ) ;
#62568 = ORIENTED_EDGE ( 'NONE', *, *, #15719, .T. ) ;
#62569 = CARTESIAN_POINT ( 'NONE',  ( 17.50000000000000000, -2.750000000000000444, 4.000000000000001776 ) ) ;
#62570 = CARTESIAN_POINT ( 'NONE',  ( -4.999999999999986677, 2.500000000000000000, -0.1000000000000022815 ) ) ;
#62571 = EDGE_CURVE ( 'NONE', #64176, #54972, #60151, .T. ) ;
#62572 = CARTESIAN_POINT ( 'NONE',  ( 186.5260416670080588, -6.551208109652273848, -3.782341765625003571 ) ) ;
#62573 = CARTESIAN_POINT ( 'NONE',  ( 5.399999999999936406, 12.50000000000000000, -3.702399969078687292 ) ) ;
#62574 = CARTESIAN_POINT ( 'NONE',  ( -14.59999999999998366, 12.50000000000000000, -0.6928203230275520319 ) ) ;
#62575 = DIRECTION ( 'NONE',  ( 0.000000000000000000, 1.000000000000000000, 0.000000000000000000 ) ) ;
#62576 = DIRECTION ( 'NONE',  ( -0.000000000000000000, 1.000000000000000000, -0.000000000000000000 ) ) ;
#62577 = CIRCLE ( 'NONE', #125252, 0.06509327318403745899 ) ;
#62578 = CARTESIAN_POINT ( 'NONE',  ( -4.150000000000025224, 12.50000000000000000, 2.792790559304612064 ) ) ;
#62579 = VECTOR ( 'NONE', #43763, 1000.000000000000000 ) ;
#62580 = ORIENTED_EDGE ( 'NONE', *, *, #57078, .T. ) ;
#62581 = CARTESIAN_POINT ( 'NONE',  ( -1.250000000000001110, 2.500000000000000000, -6.395190528383301931 ) ) ;
#62582 = FACE_OUTER_BOUND ( 'NONE', #49274, .T. ) ;
#62583 = DIRECTION ( 'NONE',  ( -0.000000000000000000, 1.000000000000000000, -0.000000000000000000 ) ) ;
#62584 = DIRECTION ( 'NONE',  ( 0.000000000000000000, 0.000000000000000000, -1.000000000000000000 ) ) ;
#62585 = AXIS2_PLACEMENT_3D ( 'NONE', #87182, #116006, #97658 ) ;
#62586 = ORIENTED_EDGE ( 'NONE', *, *, #21229, .F. ) ;
#62587 = AXIS2_PLACEMENT_3D ( 'NONE', #17440, #57390, #8273 ) ;
#62588 = DIRECTION ( 'NONE',  ( 0.000000000000000000, 0.000000000000000000, 1.000000000000000000 ) ) ;
#62589 = AXIS2_PLACEMENT_3D ( 'NONE', #99555, #50437, #68135 ) ;
#62590 = LINE ( 'NONE', #52748, #34598 ) ;
#62592 = ORIENTED_EDGE ( 'NONE', *, *, #120970, .T. ) ;
#62591 = CARTESIAN_POINT ( 'NONE',  ( 7.899999999999924860, 2.500000000000000000, 3.737306695894644371 ) ) ;
#62593 = VECTOR ( 'NONE', #15256, 1000.000000000000000 ) ;
#62594 = ORIENTED_EDGE ( 'NONE', *, *, #66063, .T. ) ;
#62595 = CARTESIAN_POINT ( 'NONE',  ( 127.5000000000000000, 2.000000000000000000, 2.000000000000001776 ) ) ;
#62596 = AXIS2_PLACEMENT_3D ( 'NONE', #101047, #81420, #11374 ) ;
#62597 = VECTOR ( 'NONE', #59730, 1000.000000000000000 ) ;
#62598 = ORIENTED_EDGE ( 'NONE', *, *, #14658, .F. ) ;
#62599 = ORIENTED_EDGE ( 'NONE', *, *, #103718, .F. ) ;
#62600 = CARTESIAN_POINT ( 'NONE',  ( -3.550000000000027800, 2.500000000000000000, 6.048780366869520364 ) ) ;
#62601 = ADVANCED_FACE ( 'NONE', ( #19685 ), #18230, .T. ) ;
#62602 = EDGE_CURVE ( 'NONE', #79916, #92862, #29505, .T. ) ;
#62603 = CARTESIAN_POINT ( 'NONE',  ( 18.09676523922475511, 2.526776815559031331, -2.684906793686053561 ) ) ;
#62605 = EDGE_CURVE ( 'NONE', #83312, #73015, #128993, .T. ) ;
#62604 = PLANE ( 'NONE',  #40062 ) ;
#62606 = CARTESIAN_POINT ( 'NONE',  ( 8.749999999999921840, 12.50000000000000000, -5.802370205355749988 ) ) ;
#62607 = ORIENTED_EDGE ( 'NONE', *, *, #53003, .F. ) ;
#62608 = DIRECTION ( 'NONE',  ( 0.000000000000000000, 1.000000000000000000, 0.000000000000000000 ) ) ;
#62610 = ORIENTED_EDGE ( 'NONE', *, *, #35531, .T. ) ;
#62609 = FACE_OUTER_BOUND ( 'NONE', #96871, .T. ) ;
#62611 = VECTOR ( 'NONE', #117367, 1000.000000000000000 ) ;
#62612 = ADVANCED_FACE ( 'NONE', ( #88400 ), #22371, .T. ) ;
#62613 = CARTESIAN_POINT ( 'NONE',  ( 108.0000000000000142, 8.700999999999998735, 0.000000000000000000 ) ) ;
#62614 = ADVANCED_FACE ( 'NONE', ( #116579 ), #48496, .T. ) ;
#62615 = CARTESIAN_POINT ( 'NONE',  ( 7.099999999999927702, 12.50000000000000000, 5.022947341949748790 ) ) ;
#62616 = EDGE_CURVE ( 'NONE', #29998, #34079, #124855, .T. ) ;
#62617 = EDGE_LOOP ( 'NONE', ( #14757, #92189 ) ) ;
#62618 = EDGE_CURVE ( 'NONE', #59390, #18883, #116424, .T. ) ;
#62619 = ADVANCED_FACE ( 'NONE', ( #107413 ), #118485, .T. ) ;
#62620 = EDGE_LOOP ( 'NONE', ( #61432, #874 ) ) ;
#62621 = ORIENTED_EDGE ( 'NONE', *, *, #59204, .F. ) ;
#62622 = ORIENTED_EDGE ( 'NONE', *, *, #46082, .T. ) ;
#62623 = DIRECTION ( 'NONE',  ( -4.274815082592931898E-19, -0.9999939076577903929, -0.003490651415223739937 ) ) ;
#62624 = CARTESIAN_POINT ( 'NONE',  ( 12.31005523291756809, 2.499999999999999556, 7.488833080794197627 ) ) ;
#62625 = DIRECTION ( 'NONE',  ( 0.000000000000000000, 1.000000000000000000, 0.000000000000000000 ) ) ;
#62626 = FACE_BOUND ( 'NONE', #70173, .T. ) ;
#62627 = ORIENTED_EDGE ( 'NONE', *, *, #12907, .F. ) ;
#62628 = CARTESIAN_POINT ( 'NONE',  ( 185.8645833340161175, -6.668395609140180369, 3.849999999999994760 ) ) ;
#62629 = AXIS2_PLACEMENT_3D ( 'NONE', #72209, #112130, #22475 ) ;
#62630 = ADVANCED_FACE ( 'NONE', ( #127695 ), #76735, .T. ) ;
#62631 = CARTESIAN_POINT ( 'NONE',  ( -8.150000000000009237, 2.500000000000000000, 6.148780366869520009 ) ) ;
#62632 = DIRECTION ( 'NONE',  ( 0.000000000000000000, 0.000000000000000000, -1.000000000000000000 ) ) ;
#62633 = DIRECTION ( 'NONE',  ( 0.000000000000000000, 0.000000000000000000, -1.000000000000000000 ) ) ;
#62634 = DIRECTION ( 'NONE',  ( 0.6795087154617358571, 9.398010995470537367E-14, -0.7336674352944538846 ) ) ;
#62635 = AXIS2_PLACEMENT_3D ( 'NONE', #41450, #80719, #90517 ) ;
#62636 = CARTESIAN_POINT ( 'NONE',  ( -3.150000000000030109, 12.50000000000000000, -2.511473670974877948 ) ) ;
#62637 = CARTESIAN_POINT ( 'NONE',  ( -1.850000000000033840, 2.500000000000000000, 6.248780366869521430 ) ) ;
#62639 = AXIS2_PLACEMENT_3D ( 'NONE', #104466, #122829, #32535 ) ;
#62638 = CIRCLE ( 'NONE', #114841, 0.06509327318403745899 ) ;
#62640 = EDGE_LOOP ( 'NONE', ( #105420, #10824, #26706, #3687 ) ) ;
#62641 = ORIENTED_EDGE ( 'NONE', *, *, #124497, .F. ) ;
#62642 = ORIENTED_EDGE ( 'NONE', *, *, #101142, .F. ) ;
#62643 = ORIENTED_EDGE ( 'NONE', *, *, #102989, .T. ) ;
#62644 = ORIENTED_EDGE ( 'NONE', *, *, #5764, .T. ) ;
#62645 = LINE ( 'NONE', #3702, #14618 ) ;
#62646 = CIRCLE ( 'NONE', #29205, 0.1000000000000000472 ) ;
#62647 = DIRECTION ( 'NONE',  ( 0.000000000000000000, -0.000000000000000000, 1.000000000000000000 ) ) ;
#62648 = VERTEX_POINT ( 'NONE', #71339 ) ;
#62649 = FACE_BOUND ( 'NONE', #84097, .T. ) ;
#62650 = CARTESIAN_POINT ( 'NONE',  ( -1.650000000000034772, 12.50000000000000000, 6.495190528383297135 ) ) ;
#62652 = AXIS2_PLACEMENT_3D ( 'NONE', #76926, #87373, #85446 ) ;
#62651 = AXIS2_PLACEMENT_3D ( 'NONE', #105856, #68498, #96654 ) ;
#62653 = ORIENTED_EDGE ( 'NONE', *, *, #71914, .T. ) ;
#62654 = DIRECTION ( 'NONE',  ( 0.000000000000000000, -0.9999939076577903929, 0.003490651415223739937 ) ) ;
#62655 = DIRECTION ( 'NONE',  ( 0.000000000000000000, -0.000000000000000000, 1.000000000000000000 ) ) ;
#62656 = LINE ( 'NONE', #94035, #60037 ) ;
#62657 = ORIENTED_EDGE ( 'NONE', *, *, #3650, .F. ) ;
#62658 = CARTESIAN_POINT ( 'NONE',  ( 139.9358549477330200, 0.5000000000000000000, -3.576063159858998475 ) ) ;
#62659 = EDGE_LOOP ( 'NONE', ( #63729, #102337, #127911, #115813 ) ) ;
#62660 = EDGE_CURVE ( 'NONE', #34783, #115836, #90998, .T. ) ;
#62661 = ORIENTED_EDGE ( 'NONE', *, *, #83241, .T. ) ;
#62662 = ORIENTED_EDGE ( 'NONE', *, *, #22671, .F. ) ;
#62663 = CIRCLE ( 'NONE', #108615, 0.06509327318403745899 ) ;
#62664 = CARTESIAN_POINT ( 'NONE',  ( -6.249999999999984901, 12.50000000000000000, -2.230156782645139391 ) ) ;
#62665 = FACE_OUTER_BOUND ( 'NONE', #88289, .T. ) ;
#62666 = CARTESIAN_POINT ( 'NONE',  ( -0.4000000000000396572, 2.500000000000000000, 3.637306695894644726 ) ) ;
#62667 = ORIENTED_EDGE ( 'NONE', *, *, #125933, .T. ) ;
#62668 = DIRECTION ( 'NONE',  ( 0.000000000000000000, 0.000000000000000000, 1.000000000000000000 ) ) ;
#62669 = AXIS2_PLACEMENT_3D ( 'NONE', #31462, #110652, #22301 ) ;
#62670 = LINE ( 'NONE', #50264, #92884 ) ;
#62671 = AXIS2_PLACEMENT_3D ( 'NONE', #94747, #73183, #64007 ) ;
#62672 = DIRECTION ( 'NONE',  ( 0.000000000000000000, 0.000000000000000000, 1.000000000000000000 ) ) ;
#62673 = DIRECTION ( 'NONE',  ( 0.000000000000000000, 1.000000000000000000, 0.000000000000000000 ) ) ;
#62674 = ORIENTED_EDGE ( 'NONE', *, *, #106007, .T. ) ;
#62675 = ADVANCED_FACE ( 'NONE', ( #2595 ), #20966, .T. ) ;
#62676 = DIRECTION ( 'NONE',  ( 0.000000000000000000, 1.000000000000000000, 0.000000000000000000 ) ) ;
#62678 = EDGE_LOOP ( 'NONE', ( #19848, #88616 ) ) ;
#62677 = VECTOR ( 'NONE', #738, 1000.000000000000000 ) ;
#62679 = CARTESIAN_POINT ( 'NONE',  ( 3.099999999999945022, 12.50000000000000000, -0.3464101615137783474 ) ) ;
#62681 = AXIS2_PLACEMENT_3D ( 'NONE', #60909, #49186, #128390 ) ;
#62680 = CIRCLE ( 'NONE', #28946, 0.1000000000000002554 ) ;
#62682 = ORIENTED_EDGE ( 'NONE', *, *, #46942, .F. ) ;
#62683 = ORIENTED_EDGE ( 'NONE', *, *, #106217, .T. ) ;
#62684 = DIRECTION ( 'NONE',  ( 0.000000000000000000, 0.000000000000000000, -1.000000000000000000 ) ) ;
#62685 = FACE_OUTER_BOUND ( 'NONE', #873, .T. ) ;
#62686 = PLANE ( 'NONE',  #6950 ) ;
#62687 = CARTESIAN_POINT ( 'NONE',  ( 13.29999999999990301, 2.500000000000000000, -4.430127018922202176 ) ) ;
#62688 = DIRECTION ( 'NONE',  ( -0.000000000000000000, 1.000000000000000000, -0.000000000000000000 ) ) ;
#62689 = EDGE_LOOP ( 'NONE', ( #125515, #53240 ) ) ;
#62690 = ORIENTED_EDGE ( 'NONE', *, *, #67560, .F. ) ;
#62691 = AXIS2_PLACEMENT_3D ( 'NONE', #28293, #8621, #78028 ) ;
#62692 = LINE ( 'NONE', #30663, #60233 ) ;
#62693 = FACE_OUTER_BOUND ( 'NONE', #83694, .T. ) ;
#62694 = CARTESIAN_POINT ( 'NONE',  ( 12.09999999999990195, 12.50000000000000000, 0.06509327318403515528 ) ) ;
#62695 = VERTEX_POINT ( 'NONE', #111930 ) ;
#62696 = EDGE_LOOP ( 'NONE', ( #73543, #106048 ) ) ;
#62697 = FACE_OUTER_BOUND ( 'NONE', #59139, .T. ) ;
#62698 = CONICAL_SURFACE ( 'NONE', #8293, 0.1000000000000000472, 0.003490658503988666988 ) ;
#62699 = EDGE_LOOP ( 'NONE', ( #15462, #7060, #85072, #56272 ) ) ;
#62700 = DIRECTION ( 'NONE',  ( 0.000000000000000000, 0.000000000000000000, 1.000000000000000000 ) ) ;
#62701 = DIRECTION ( 'NONE',  ( -0.000000000000000000, -1.000000000000000000, -0.000000000000000000 ) ) ;
#62702 = EDGE_CURVE ( 'NONE', #19796, #103770, #21616, .T. ) ;
#62703 = DIRECTION ( 'NONE',  ( 0.000000000000000000, 0.000000000000000000, 1.000000000000000000 ) ) ;
#62704 = ORIENTED_EDGE ( 'NONE', *, *, #68480, .F. ) ;
#62705 = PLANE ( 'NONE',  #39877 ) ;
#62706 = CARTESIAN_POINT ( 'NONE',  ( 5.849999999999931255, 2.500000000000000000, 2.857883832488649301 ) ) ;
#62707 = CARTESIAN_POINT ( 'NONE',  ( -12.49999999999999289, 2.500000000000000000, 3.637306695894644726 ) ) ;
#62708 = AXIS2_PLACEMENT_3D ( 'NONE', #4003, #5288, #34132 ) ;
#62709 = CARTESIAN_POINT ( 'NONE',  ( 11.89999999999990443, 12.50000000000000000, 0.3464101615137736845 ) ) ;
#62710 = PLANE ( 'NONE',  #64624 ) ;
#62711 = ADVANCED_FACE ( 'NONE', ( #51728 ), #675, .T. ) ;
#62712 = ORIENTED_EDGE ( 'NONE', *, *, #24349, .T. ) ;
#62713 = CARTESIAN_POINT ( 'NONE',  ( -14.14999999999998614, 2.500000000000000000, -2.857883832488651521 ) ) ;
#62714 = CARTESIAN_POINT ( 'NONE',  ( 87.50000000000001421, -3.974992050023846257, 6.359987280038162716 ) ) ;
#62715 = EDGE_CURVE ( 'NONE', #6628, #107306, #90328, .T. ) ;
#62716 = VERTEX_POINT ( 'NONE', #61550 ) ;
#62717 = EDGE_CURVE ( 'NONE', #77053, #5250, #110633, .T. ) ;
#62718 = ORIENTED_EDGE ( 'NONE', *, *, #101038, .T. ) ;
#62719 = ADVANCED_FACE ( 'NONE', ( #81808 ), #122792, .T. ) ;
#62720 = CARTESIAN_POINT ( 'NONE',  ( 184.9843750003414016, -8.734944146203032389, -1.604583208406768146E-15 ) ) ;
#62722 = EDGE_CURVE ( 'NONE', #37252, #123620, #91639, .T. ) ;
#62721 = CARTESIAN_POINT ( 'NONE',  ( -10.40000000000000213, 2.500000000000000000, 5.122947341949749323 ) ) ;
#62723 = ADVANCED_FACE ( 'NONE', ( #111252 ), #35073, .T. ) ;
#62724 = CARTESIAN_POINT ( 'NONE',  ( 179.5000000000000000, 0.6250000000000000000, 6.000000000000000000 ) ) ;
#62725 = CARTESIAN_POINT ( 'NONE',  ( -7.950000000000012612, 2.500000000000000000, 2.265063509461097357 ) ) ;
#62726 = DIRECTION ( 'NONE',  ( 0.000000000000000000, 1.000000000000000000, 0.000000000000000000 ) ) ;
#62727 = CARTESIAN_POINT ( 'NONE',  ( 7.299999999999926104, 2.500000000000000000, -0.3464101615137782364 ) ) ;
#62728 = DIRECTION ( 'NONE',  ( 0.000000000000000000, 0.000000000000000000, 1.000000000000000000 ) ) ;
#62729 = CARTESIAN_POINT ( 'NONE',  ( 12.89999999999989910, 2.500000000000000000, -0.5928203230275542746 ) ) ;
#62730 = AXIS2_PLACEMENT_3D ( 'NONE', #85687, #37256, #56856 ) ;
#62731 = EDGE_CURVE ( 'NONE', #39246, #5618, #116522, .T. ) ;
#62732 = PLANE ( 'NONE',  #70973 ) ;
#62733 = VERTEX_POINT ( 'NONE', #102110 ) ;
#62734 = EDGE_CURVE ( 'NONE', #80247, #14617, #30160, .T. ) ;
#62735 = ORIENTED_EDGE ( 'NONE', *, *, #21225, .F. ) ;
#62737 = AXIS2_PLACEMENT_3D ( 'NONE', #4308, #93367, #123455 ) ;
#62736 = AXIS2_PLACEMENT_3D ( 'NONE', #63212, #13460, #93325 ) ;
#62738 = ORIENTED_EDGE ( 'NONE', *, *, #13295, .T. ) ;
#62739 = EDGE_LOOP ( 'NONE', ( #29310, #65185 ) ) ;
#62740 = CARTESIAN_POINT ( 'NONE',  ( 10.64999999999991331, 12.50000000000000000, -2.511473670974877948 ) ) ;
#62741 = DIRECTION ( 'NONE',  ( 0.000000000000000000, 1.000000000000000000, 0.000000000000000000 ) ) ;
#62744 = ORIENTED_EDGE ( 'NONE', *, *, #104778, .F. ) ;
#62743 = CIRCLE ( 'NONE', #14591, 0.1000000000000002554 ) ;
#62742 = AXIS2_PLACEMENT_3D ( 'NONE', #91866, #44051, #114714 ) ;
#62745 = DIRECTION ( 'NONE',  ( 1.000000000000000000, 0.000000000000000000, 0.000000000000000000 ) ) ;
#62746 = CARTESIAN_POINT ( 'NONE',  ( -7.100000000000013856, 2.500000000000000000, 3.637306695894644726 ) ) ;
#62748 = ORIENTED_EDGE ( 'NONE', *, *, #36312, .T. ) ;
#62747 = CARTESIAN_POINT ( 'NONE',  ( -8.950000000000008171, 12.50000000000000000, 1.883746621131358934 ) ) ;
#62749 = CARTESIAN_POINT ( 'NONE',  ( -12.09999999999999609, 2.500000000000000000, -4.430127018922199511 ) ) ;
#62750 = DIRECTION ( 'NONE',  ( 0.000000000000000000, 1.000000000000000000, 0.000000000000000000 ) ) ;
#62751 = ORIENTED_EDGE ( 'NONE', *, *, #41884, .T. ) ;
#62752 = ORIENTED_EDGE ( 'NONE', *, *, #93173, .T. ) ;
#62753 = ORIENTED_EDGE ( 'NONE', *, *, #115140, .F. ) ;
#62754 = VERTEX_POINT ( 'NONE', #11784 ) ;
#62755 = DIRECTION ( 'NONE',  ( 0.000000000000000000, 0.000000000000000000, 1.000000000000000000 ) ) ;
#62756 = DIRECTION ( 'NONE',  ( 0.000000000000000000, 0.000000000000000000, -1.000000000000000000 ) ) ;
#62758 = ADVANCED_FACE ( 'NONE', ( #32096 ), #64298, .T. ) ;
#62757 = DIRECTION ( 'NONE',  ( 0.000000000000000000, 0.000000000000000000, 1.000000000000000000 ) ) ;
#62759 = DIRECTION ( 'NONE',  ( -0.000000000000000000, -1.000000000000000000, -0.000000000000000000 ) ) ;
#62760 = CONICAL_SURFACE ( 'NONE', #25090, 0.1000000000000002554, 0.003490658503988666988 ) ;
#62761 = VERTEX_POINT ( 'NONE', #82481 ) ;
#62762 = EDGE_CURVE ( 'NONE', #110935, #22979, #118672, .T. ) ;
#62763 = FACE_OUTER_BOUND ( 'NONE', #88473, .T. ) ;
#62764 = ORIENTED_EDGE ( 'NONE', *, *, #112579, .T. ) ;
#62765 = FACE_OUTER_BOUND ( 'NONE', #88947, .T. ) ;
#62766 = LINE ( 'NONE', #52295, #104026 ) ;
#62767 = CARTESIAN_POINT ( 'NONE',  ( 6.849999999999930367, 2.500000000000000000, -6.048780366869526581 ) ) ;
#62768 = FACE_OUTER_BOUND ( 'NONE', #109022, .T. ) ;
#62769 = EDGE_CURVE ( 'NONE', #129537, #76489, #29929, .T. ) ;
#62770 = CONICAL_SURFACE ( 'NONE', #64806, 0.1000000000000002554, 0.003490658503988666988 ) ;
#62771 = EDGE_CURVE ( 'NONE', #33584, #89626, #50218, .T. ) ;
#62772 = EDGE_LOOP ( 'NONE', ( #38554, #9436 ) ) ;
#62773 = ADVANCED_FACE ( 'NONE', ( #69847 ), #70556, .T. ) ;
#62774 = ORIENTED_EDGE ( 'NONE', *, *, #103669, .F. ) ;
#62775 = ORIENTED_EDGE ( 'NONE', *, *, #125876, .F. ) ;
#62776 = CARTESIAN_POINT ( 'NONE',  ( 6.049999999999930544, 12.50000000000000000, 2.576566944158910744 ) ) ;
#62777 = DIRECTION ( 'NONE',  ( 0.000000000000000000, 0.000000000000000000, 1.000000000000000000 ) ) ;
#62778 = CARTESIAN_POINT ( 'NONE',  ( 4.599999999999936584, 12.50000000000000000, 3.572213422710607489 ) ) ;
#62779 = FACE_BOUND ( 'NONE', #94245, .T. ) ;
#62780 = AXIS2_PLACEMENT_3D ( 'NONE', #26250, #40436, #126379 ) ;
#62781 = CARTESIAN_POINT ( 'NONE',  ( -6.250000000000021316, 12.50000000000000000, -5.802370205355749988 ) ) ;
#62782 = DIRECTION ( 'NONE',  ( -0.000000000000000000, 1.000000000000000000, -0.000000000000000000 ) ) ;
#62783 = EDGE_CURVE ( 'NONE', #89626, #6313, #28808, .T. ) ;
#62784 = CARTESIAN_POINT ( 'NONE',  ( 2.299999999999948752, 12.50000000000000000, 0.4115034346978109769 ) ) ;
#62785 = CIRCLE ( 'NONE', #23063, 0.06509327318403743123 ) ;
#62786 = AXIS2_PLACEMENT_3D ( 'NONE', #37813, #48936, #77718 ) ;
#62787 = CARTESIAN_POINT ( 'NONE',  ( 187.0052083336747444, -6.551208109652278289, 3.782341765624995134 ) ) ;
#62788 = DIRECTION ( 'NONE',  ( 0.000000000000000000, 0.000000000000000000, 1.000000000000000000 ) ) ;
#62789 = DIRECTION ( 'NONE',  ( 0.000000000000000000, 0.000000000000000000, 1.000000000000000000 ) ) ;
#62790 = ORIENTED_EDGE ( 'NONE', *, *, #11742, .F. ) ;
#62791 = CIRCLE ( 'NONE', #37742, 0.1000000000000002554 ) ;
#62792 = LINE ( 'NONE', #15596, #99519 ) ;
#62793 = CIRCLE ( 'NONE', #16691, 0.06509327318403745899 ) ;
#62794 = EDGE_LOOP ( 'NONE', ( #61950, #81273, #111343, #116406 ) ) ;
#62795 = ORIENTED_EDGE ( 'NONE', *, *, #99190, .T. ) ;
#62796 = CARTESIAN_POINT ( 'NONE',  ( 14.59999999999989484, 2.500000000000000000, -2.276824562219559311E-15 ) ) ;
#62797 = CARTESIAN_POINT ( 'NONE',  ( -7.500000000000016875, 2.500000000000000000, 0.7928203230275495672 ) ) ;
#62798 = EDGE_CURVE ( 'NONE', #23803, #27914, #129440, .T. ) ;
#62799 = FACE_BOUND ( 'NONE', #38044, .T. ) ;
#62800 = DIRECTION ( 'NONE',  ( -0.000000000000000000, 1.000000000000000000, -0.000000000000000000 ) ) ;
#62801 = VERTEX_POINT ( 'NONE', #39127 ) ;
#62802 = CARTESIAN_POINT ( 'NONE',  ( -12.29999999999999716, 12.50000000000000000, -3.983716857408423628 ) ) ;
#62803 = LINE ( 'NONE', #102702, #22779 ) ;
#62804 = ORIENTED_EDGE ( 'NONE', *, *, #31382, .F. ) ;
#62805 = DIRECTION ( 'NONE',  ( -0.000000000000000000, -1.000000000000000000, -0.000000000000000000 ) ) ;
#62806 = CARTESIAN_POINT ( 'NONE',  ( 5.399999999999932854, 12.50000000000000000, 5.022947341949748790 ) ) ;
#62807 = ADVANCED_FACE ( 'NONE', ( #48270 ), #114469, .T. ) ;
#62808 = CIRCLE ( 'NONE', #29369, 0.06509327318403745899 ) ;
#62809 = ORIENTED_EDGE ( 'NONE', *, *, #19225, .T. ) ;
#62810 = DIRECTION ( 'NONE',  ( 0.000000000000000000, 0.000000000000000000, 1.000000000000000000 ) ) ;
#62811 = AXIS2_PLACEMENT_3D ( 'NONE', #36466, #106466, #16130 ) ;
#62812 = DIRECTION ( 'NONE',  ( 0.000000000000000000, 0.000000000000000000, 1.000000000000000000 ) ) ;
#62813 = EDGE_LOOP ( 'NONE', ( #13846, #106562, #17092, #61119 ) ) ;
#62814 = DIRECTION ( 'NONE',  ( 0.000000000000000000, 1.000000000000000000, 0.000000000000000000 ) ) ;
#62816 = CONICAL_SURFACE ( 'NONE', #117079, 0.1000000000000002554, 0.003490658503988666988 ) ;
#62815 = VECTOR ( 'NONE', #32978, 1000.000000000000000 ) ;
#62817 = DIRECTION ( 'NONE',  ( 1.000000000000000000, -0.000000000000000000, -0.000000000000000000 ) ) ;
#62818 = CARTESIAN_POINT ( 'NONE',  ( 8.749999999999923617, 12.50000000000000000, -7.188010851410854052 ) ) ;
#62819 = ORIENTED_EDGE ( 'NONE', *, *, #72373, .F. ) ;
#62820 = ORIENTED_EDGE ( 'NONE', *, *, #33174, .F. ) ;
#62821 = EDGE_CURVE ( 'NONE', #17776, #16630, #18156, .T. ) ;
#62822 = CARTESIAN_POINT ( 'NONE',  ( 184.5000000000000000, 0.000000000000000000, 0.000000000000000000 ) ) ;
#62823 = ORIENTED_EDGE ( 'NONE', *, *, #72157, .F. ) ;
#62824 = CARTESIAN_POINT ( 'NONE',  ( -6.850000000000013856, 2.500000000000000000, 1.718653347947321386 ) ) ;
#62825 = DIRECTION ( 'NONE',  ( -0.000000000000000000, -1.000000000000000000, -0.000000000000000000 ) ) ;
#62826 = VERTEX_POINT ( 'NONE', #128127 ) ;
#62827 = DIRECTION ( 'NONE',  ( 1.000000000000000000, 0.000000000000000000, 0.000000000000000000 ) ) ;
#62828 = FACE_OUTER_BOUND ( 'NONE', #107974, .T. ) ;
#62829 = DIRECTION ( 'NONE',  ( -0.000000000000000000, -1.000000000000000000, -0.000000000000000000 ) ) ;
#62830 = LINE ( 'NONE', #63475, #52865 ) ;
#62831 = CARTESIAN_POINT ( 'NONE',  ( 108.0000000000000142, 8.500000000000000000, 2.249999999999996891 ) ) ;
#62832 = EDGE_LOOP ( 'NONE', ( #99138, #90717, #68305, #36933 ) ) ;
#62833 = ORIENTED_EDGE ( 'NONE', *, *, #92188, .F. ) ;
#62834 = DIRECTION ( 'NONE',  ( -0.000000000000000000, 1.000000000000000000, -0.000000000000000000 ) ) ;
#62835 = ORIENTED_EDGE ( 'NONE', *, *, #126328, .F. ) ;
#62836 = CARTESIAN_POINT ( 'NONE',  ( -5.400000000000019895, 2.500000000000000000, -0.6928203230275541413 ) ) ;
#62838 = ORIENTED_EDGE ( 'NONE', *, *, #109411, .T. ) ;
#62837 = ORIENTED_EDGE ( 'NONE', *, *, #109523, .T. ) ;
#62839 = VERTEX_POINT ( 'NONE', #87540 ) ;
#62840 = CARTESIAN_POINT ( 'NONE',  ( 0.6499999999999561684, 12.50000000000000000, 2.511473670974873507 ) ) ;
#62841 = AXIS2_PLACEMENT_3D ( 'NONE', #60326, #21673, #62248 ) ;
#62842 = CARTESIAN_POINT ( 'NONE',  ( 2.891205793294708895E-16, 5.000000000000000000, 2.000000000000020428 ) ) ;
#62843 = CONICAL_SURFACE ( 'NONE', #52378, 0.1000000000000000056, 0.003490658503988666988 ) ;
#62844 = CARTESIAN_POINT ( 'NONE',  ( -14.99999999999998401, 12.50000000000000000, 0.6928203230275518099 ) ) ;
#62845 = EDGE_CURVE ( 'NONE', #14124, #84685, #74774, .T. ) ;
#62846 = CARTESIAN_POINT ( 'NONE',  ( -5.400000000000019895, 12.50000000000000000, 4.330127018922196314 ) ) ;
#62847 = DIRECTION ( 'NONE',  ( 0.000000000000000000, 0.000000000000000000, -1.000000000000000000 ) ) ;
#62848 = PLANE ( 'NONE',  #29780 ) ;
#62849 = DIRECTION ( 'NONE',  ( 0.000000000000000000, 1.000000000000000000, 0.000000000000000000 ) ) ;
#62850 = DIRECTION ( 'NONE',  ( 0.000000000000000000, 0.000000000000000000, 1.000000000000000000 ) ) ;
#62852 = AXIS2_PLACEMENT_3D ( 'NONE', #86892, #128786, #56138 ) ;
#62851 = CARTESIAN_POINT ( 'NONE',  ( -4.150000000000024336, 12.50000000000000000, 2.099970236277060032 ) ) ;
#62853 = EDGE_CURVE ( 'NONE', #83526, #126341, #104015, .T. ) ;
#62854 = ORIENTED_EDGE ( 'NONE', *, *, #31123, .F. ) ;
#62855 = CARTESIAN_POINT ( 'NONE',  ( -16.50000000000000000, -2.500000000000000000, 1.734723475976807094E-15 ) ) ;
#62856 = ADVANCED_FACE ( 'NONE', ( #20103 ), #118578, .T. ) ;
#62857 = ORIENTED_EDGE ( 'NONE', *, *, #102191, .T. ) ;
#62858 = EDGE_CURVE ( 'NONE', #87021, #101722, #60122, .T. ) ;
#62859 = ORIENTED_EDGE ( 'NONE', *, *, #21775, .F. ) ;
#62860 = EDGE_CURVE ( 'NONE', #50743, #34595, #8976, .T. ) ;
#62861 = DIRECTION ( 'NONE',  ( 0.000000000000000000, 0.000000000000000000, -1.000000000000000000 ) ) ;
#62863 = EDGE_CURVE ( 'NONE', #121543, #55871, #95604, .T. ) ;
#62862 = DIRECTION ( 'NONE',  ( 0.000000000000000000, 0.000000000000000000, 1.000000000000000000 ) ) ;
#62864 = DIRECTION ( 'NONE',  ( 0.000000000000000000, 0.000000000000000000, -1.000000000000000000 ) ) ;
#62865 = AXIS2_PLACEMENT_3D ( 'NONE', #29430, #99465, #9777 ) ;
#62866 = CARTESIAN_POINT ( 'NONE',  ( 1.249999999999952038, 2.500000000000000000, -1.372243186433550033 ) ) ;
#62867 = VECTOR ( 'NONE', #110414, 1000.000000000000000 ) ;
#62868 = DIRECTION ( 'NONE',  ( 0.000000000000000000, 1.000000000000000000, 0.000000000000000000 ) ) ;
#62869 = ADVANCED_FACE ( 'NONE', ( #19445 ), #39198, .T. ) ;
#62870 = DIRECTION ( 'NONE',  ( 0.000000000000000000, 1.000000000000000000, 0.000000000000000000 ) ) ;
#62871 = EDGE_CURVE ( 'NONE', #16061, #40173, #53843, .T. ) ;
#62872 = DIRECTION ( 'NONE',  ( -0.000000000000000000, -1.000000000000000000, -0.000000000000000000 ) ) ;
#62873 = EDGE_LOOP ( 'NONE', ( #285, #74770, #109958, #60690 ) ) ;
#62874 = ADVANCED_FACE ( 'NONE', ( #27320 ), #7854, .T. ) ;
#62875 = EDGE_CURVE ( 'NONE', #116833, #49326, #58057, .T. ) ;
#62876 = CIRCLE ( 'NONE', #52402, 0.09999999999999982514 ) ;
#62877 = EDGE_CURVE ( 'NONE', #80574, #84780, #55885, .T. ) ;
#62878 = ORIENTED_EDGE ( 'NONE', *, *, #88422, .F. ) ;
#62879 = ADVANCED_FACE ( 'NONE', ( #39765 ), #18321, .T. ) ;
#62880 = ORIENTED_EDGE ( 'NONE', *, *, #74984, .F. ) ;
#62881 = AXIS2_PLACEMENT_3D ( 'NONE', #97235, #7552, #9506 ) ;
#62882 = ORIENTED_EDGE ( 'NONE', *, *, #83562, .T. ) ;
#62883 = VERTEX_POINT ( 'NONE', #59658 ) ;
#62884 = EDGE_CURVE ( 'NONE', #59076, #99205, #58983, .T. ) ;
#62885 = FACE_OUTER_BOUND ( 'NONE', #108575, .T. ) ;
#62886 = DIRECTION ( 'NONE',  ( 0.000000000000000000, 0.000000000000000000, -1.000000000000000000 ) ) ;
#62887 = DIRECTION ( 'NONE',  ( 0.000000000000000000, 1.000000000000000000, 0.000000000000000000 ) ) ;
#62888 = DIRECTION ( 'NONE',  ( -0.000000000000000000, -1.000000000000000000, -0.000000000000000000 ) ) ;
#62889 = CARTESIAN_POINT ( 'NONE',  ( 3.349999999999941025, 12.50000000000000000, 7.188010851410848723 ) ) ;
#62890 = EDGE_LOOP ( 'NONE', ( #62820, #68531 ) ) ;
#62891 = CARTESIAN_POINT ( 'NONE',  ( -7.050000000000016698, 2.500000000000000000, -6.595190528383302109 ) ) ;
#62892 = CARTESIAN_POINT ( 'NONE',  ( -1.850000000000033840, 2.500000000000000000, 6.148780366869520897 ) ) ;
#62893 = CARTESIAN_POINT ( 'NONE',  ( -10.85000000000000142, 12.50000000000000000, -7.188010851410850499 ) ) ;
#62894 = CARTESIAN_POINT ( 'NONE',  ( 14.79999999999989413, 2.500000000000000000, -0.4464101615137782142 ) ) ;
#62895 = EDGE_LOOP ( 'NONE', ( #9286, #122839, #106084, #106659 ) ) ;
#62896 = EDGE_LOOP ( 'NONE', ( #115051, #83812 ) ) ;
#62897 = EDGE_LOOP ( 'NONE', ( #24680, #60660, #118032, #68112 ) ) ;
#62898 = AXIS2_PLACEMENT_3D ( 'NONE', #54328, #81838, #82517 ) ;
#62899 = DIRECTION ( 'NONE',  ( -0.000000000000000000, 1.000000000000000000, -0.000000000000000000 ) ) ;
#62900 = AXIS2_PLACEMENT_3D ( 'NONE', #50013, #30369, #89908 ) ;
#62901 = CONICAL_SURFACE ( 'NONE', #16881, 0.1000000000000002554, 0.003490658503988666988 ) ;
#62902 = DIRECTION ( 'NONE',  ( 0.000000000000000000, -0.9999939076577903929, 0.003490651415223739937 ) ) ;
#62903 = CARTESIAN_POINT ( 'NONE',  ( -0.8000000000000381251, 2.500000000000000000, 4.230127018922196669 ) ) ;
#62904 = CONICAL_SURFACE ( 'NONE', #4286, 0.1000000000000002554, 0.003490658503988666988 ) ;
#62906 = VERTEX_POINT ( 'NONE', #47881 ) ;
#62905 = CONICAL_SURFACE ( 'NONE', #94283, 0.1000000000000002554, 0.003490658503988666988 ) ;
#62907 = CARTESIAN_POINT ( 'NONE',  ( -10.00000000000000355, 2.500000000000000000, 3.537306695894645081 ) ) ;
#62908 = DIRECTION ( 'NONE',  ( -0.000000000000000000, -1.000000000000000000, -0.000000000000000000 ) ) ;
#62909 = DIRECTION ( 'NONE',  ( 0.000000000000000000, 1.000000000000000000, 0.000000000000000000 ) ) ;
#62910 = CARTESIAN_POINT ( 'NONE',  ( -2.950000000000029932, 12.50000000000000000, -2.099970236277064473 ) ) ;
#62911 = EDGE_CURVE ( 'NONE', #25124, #121281, #129086, .T. ) ;
#62912 = CARTESIAN_POINT ( 'NONE',  ( 6.649999999999928413, 2.500000000000000000, 2.957883832488649389 ) ) ;
#62913 = ADVANCED_FACE ( 'NONE', ( #119828 ), #10505, .T. ) ;
#62914 = VERTEX_POINT ( 'NONE', #39366 ) ;
#62915 = ORIENTED_EDGE ( 'NONE', *, *, #13510, .T. ) ;
#62916 = CARTESIAN_POINT ( 'NONE',  ( -12.49999999999995737, 2.500000000000000000, 4.430127018922196847 ) ) ;
#62917 = FACE_OUTER_BOUND ( 'NONE', #6808, .T. ) ;
#62918 = CARTESIAN_POINT ( 'NONE',  ( 6.899999999999928413, 2.500000000000000000, -3.983716857408426293 ) ) ;
#62919 = ADVANCED_FACE ( 'NONE', ( #69428 ), #97831, .T. ) ;
#62920 = DIRECTION ( 'NONE',  ( 0.000000000000000000, 0.000000000000000000, 1.000000000000000000 ) ) ;
#62921 = VERTEX_POINT ( 'NONE', #7930 ) ;
#62922 = EDGE_LOOP ( 'NONE', ( #107425, #48365, #57848, #11167 ) ) ;
#62923 = CARTESIAN_POINT ( 'NONE',  ( 5.399999999999935518, 12.50000000000000000, -4.265033745738164406 ) ) ;
#62924 = DIRECTION ( 'NONE',  ( -4.274815082592931898E-19, -0.9999939076577903929, -0.003490651415223739937 ) ) ;
#62925 = DIRECTION ( 'NONE',  ( 0.000000000000000000, 0.000000000000000000, 1.000000000000000000 ) ) ;
#62926 = CARTESIAN_POINT ( 'NONE',  ( -1.650000000000034328, 2.500000000000000000, -6.495190528383302464 ) ) ;
#62927 = EDGE_LOOP ( 'NONE', ( #100487, #6436, #115974, #30213 ) ) ;
#62928 = VECTOR ( 'NONE', #120367, 1000.000000000000000 ) ;
#62929 = FACE_OUTER_BOUND ( 'NONE', #113028, .T. ) ;
#62930 = CIRCLE ( 'NONE', #44151, 0.1000000000000002554 ) ;
#62931 = CARTESIAN_POINT ( 'NONE',  ( -11.44999999999999751, 2.500000000000000000, 6.941600689897073018 ) ) ;
#62932 = ORIENTED_EDGE ( 'NONE', *, *, #31433, .T. ) ;
#62933 = CARTESIAN_POINT ( 'NONE',  ( 9.999999999999914735, 2.500000000000000000, 0.6928203230275494784 ) ) ;
#62934 = ORIENTED_EDGE ( 'NONE', *, *, #81501, .F. ) ;
#62935 = AXIS2_PLACEMENT_3D ( 'NONE', #11345, #214, #41475 ) ;
#62936 = DIRECTION ( 'NONE',  ( 0.000000000000000000, 1.000000000000000000, 0.000000000000000000 ) ) ;
#62937 = AXIS2_PLACEMENT_3D ( 'NONE', #108732, #10525, #90370 ) ;
#62938 = ORIENTED_EDGE ( 'NONE', *, *, #77105, .T. ) ;
#62939 = CARTESIAN_POINT ( 'NONE',  ( -11.25000000000000178, 2.500000000000000000, -1.572243186433546214 ) ) ;
#62940 = DIRECTION ( 'NONE',  ( 0.000000000000000000, -0.9999939076577903929, 0.003490651415223739937 ) ) ;
#62941 = ORIENTED_EDGE ( 'NONE', *, *, #112935, .T. ) ;
#62942 = ORIENTED_EDGE ( 'NONE', *, *, #7695, .F. ) ;
#62943 = CARTESIAN_POINT ( 'NONE',  ( 184.7968750003414016, 8.734944146203032389, 5.348610694689227483E-16 ) ) ;
#62944 = CARTESIAN_POINT ( 'NONE',  ( 14.39999999999989555, 2.500000000000000000, -0.2464101615137782308 ) ) ;
#62946 = CARTESIAN_POINT ( 'NONE',  ( 186.6718750003414016, 9.264065473108010111E-16, -7.564683531250000925 ) ) ;
#62945 = AXIS2_PLACEMENT_3D ( 'NONE', #26048, #5100, #16199 ) ;
#62947 = CARTESIAN_POINT ( 'NONE',  ( 183.9010416670080588, -4.367472073101520635, 7.564683531249999149 ) ) ;
#62948 = AXIS2_PLACEMENT_3D ( 'NONE', #33788, #126021, #54078 ) ;
#62949 = DIRECTION ( 'NONE',  ( -0.000000000000000000, 1.000000000000000000, -0.000000000000000000 ) ) ;
#62950 = CARTESIAN_POINT ( 'NONE',  ( -12.09999999999999609, 2.500000000000000000, 0.6928203230275535862 ) ) ;
#62951 = CARTESIAN_POINT ( 'NONE',  ( -1.900000000000034994, 2.500000000000000000, -4.676537180435978769 ) ) ;
#62952 = CARTESIAN_POINT ( 'NONE',  ( -1.450000000000036371, 12.50000000000000000, 2.511473670974873507 ) ) ;
#62953 = CARTESIAN_POINT ( 'NONE',  ( -9.350000000000008527, 2.500000000000000000, -6.841600689897072485 ) ) ;
#62954 = AXIS2_PLACEMENT_3D ( 'NONE', #33168, #12834, #110416 ) ;
#62955 = VERTEX_POINT ( 'NONE', #79276 ) ;
#62956 = EDGE_LOOP ( 'NONE', ( #27148, #82585 ) ) ;
#62957 = DIRECTION ( 'NONE',  ( 0.000000000000000000, -0.9999939076577903929, 0.003490651415223739937 ) ) ;
#62958 = EDGE_LOOP ( 'NONE', ( #9088, #104268, #85998, #25017 ) ) ;
#62959 = CIRCLE ( 'NONE', #31575, 0.06509327318403745899 ) ;
#62960 = CONICAL_SURFACE ( 'NONE', #56679, 0.1000000000000002554, 0.003490658503988666988 ) ;
#62961 = CARTESIAN_POINT ( 'NONE',  ( 2.699999999999947331, 2.500000000000000000, -4.676537180435978769 ) ) ;
#62962 = CARTESIAN_POINT ( 'NONE',  ( 13.74999999999989697, 2.500000000000000000, 2.857883832488649301 ) ) ;
#62963 = EDGE_CURVE ( 'NONE', #16380, #110762, #41434, .T. ) ;
#62964 = CARTESIAN_POINT ( 'NONE',  ( 6.849999999999929479, 12.50000000000000000, 6.776507416713035248 ) ) ;
#62966 = VERTEX_POINT ( 'NONE', #28885 ) ;
#62965 = VERTEX_POINT ( 'NONE', #89722 ) ;
#62967 = FACE_BOUND ( 'NONE', #13712, .T. ) ;
#62968 = VERTEX_POINT ( 'NONE', #98247 ) ;
#62969 = ADVANCED_FACE ( 'NONE', ( #58350 ), #9237, .T. ) ;
#62970 = CARTESIAN_POINT ( 'NONE',  ( 11.24999999999990763, 12.50000000000000000, 1.472243186433545459 ) ) ;
#62971 = CARTESIAN_POINT ( 'NONE',  ( -11.05000000000000071, 2.500000000000000000, 6.941600689897073018 ) ) ;
#62972 = DIRECTION ( 'NONE',  ( -4.274815082592931898E-19, -0.9999939076577903929, -0.003490651415223739937 ) ) ;
#62973 = CARTESIAN_POINT ( 'NONE',  ( -1.450000000000035483, 2.500000000000000000, 1.918653347947321564 ) ) ;
#62974 = CARTESIAN_POINT ( 'NONE',  ( 184.5312500006828031, 9.429780353434619030E-16, -7.700000000000000178 ) ) ;
#62975 = CARTESIAN_POINT ( 'NONE',  ( -11.25000000000000178, 2.500000000000000000, -1.472243186433546125 ) ) ;
#62976 = DIRECTION ( 'NONE',  ( 0.000000000000000000, 0.000000000000000000, 1.000000000000000000 ) ) ;
#62977 = CARTESIAN_POINT ( 'NONE',  ( 6.249999999999930722, 12.50000000000000000, 7.253104124594885960 ) ) ;
#62978 = EDGE_CURVE ( 'NONE', #47871, #89250, #1688, .T. ) ;
#62979 = DIRECTION ( 'NONE',  ( 0.000000000000000000, 0.000000000000000000, 1.000000000000000000 ) ) ;
#62980 = CARTESIAN_POINT ( 'NONE',  ( 6.049999999999934097, 2.500000000000000000, 6.148780366869520897 ) ) ;
#62981 = CARTESIAN_POINT ( 'NONE',  ( -4.800000000000026468, 2.500000000000000000, -4.576537180435978236 ) ) ;
#62982 = ORIENTED_EDGE ( 'NONE', *, *, #61884, .T. ) ;
#62983 = EDGE_LOOP ( 'NONE', ( #58641, #88389 ) ) ;
#62984 = EDGE_LOOP ( 'NONE', ( #129490, #110047 ) ) ;
#62985 = DIRECTION ( 'NONE',  ( 0.000000000000000000, -0.000000000000000000, 1.000000000000000000 ) ) ;
#62986 = ORIENTED_EDGE ( 'NONE', *, *, #94442, .T. ) ;
#62987 = AXIS2_PLACEMENT_3D ( 'NONE', #16310, #56252, #57558 ) ;
#62988 = DIRECTION ( 'NONE',  ( 0.000000000000000000, 0.000000000000000000, 1.000000000000000000 ) ) ;
#62989 = CIRCLE ( 'NONE', #48317, 0.1000000000000002554 ) ;
#62990 = AXIS2_PLACEMENT_3D ( 'NONE', #7459, #17259, #127891 ) ;
#62992 = ORIENTED_EDGE ( 'NONE', *, *, #90423, .F. ) ;
#62991 = VERTEX_POINT ( 'NONE', #118531 ) ;
#62993 = VERTEX_POINT ( 'NONE', #68140 ) ;
#62994 = CARTESIAN_POINT ( 'NONE',  ( 5.599999999999933031, 2.500000000000000000, 0.2464101615137735679 ) ) ;
#62995 = VECTOR ( 'NONE', #24916, 1000.000000000000000 ) ;
#62996 = DIRECTION ( 'NONE',  ( 0.000000000000000000, 0.000000000000000000, -1.000000000000000000 ) ) ;
#62998 = ADVANCED_FACE ( 'NONE', ( #60294 ), #55969, .T. ) ;
#62997 = AXIS2_PLACEMENT_3D ( 'NONE', #73758, #124159, #113703 ) ;
#62999 = LINE ( 'NONE', #93117, #70644 ) ;
#63000 = DIRECTION ( 'NONE',  ( -4.274815082592931898E-19, -0.9999939076577903929, -0.003490651415223739937 ) ) ;
#63001 = CARTESIAN_POINT ( 'NONE',  ( 185.2812500006828031, 0.000000000000000000, 7.700000000000000178 ) ) ;
#63002 = AXIS2_PLACEMENT_3D ( 'NONE', #105672, #4869, #25819 ) ;
#63003 = LINE ( 'NONE', #13236, #24566 ) ;
#63004 = ORIENTED_EDGE ( 'NONE', *, *, #14656, .T. ) ;
#63005 = CARTESIAN_POINT ( 'NONE',  ( 1.449999999999950440, 12.50000000000000000, 6.148780366869520009 ) ) ;
#63006 = ORIENTED_EDGE ( 'NONE', *, *, #96376, .F. ) ;
#63007 = EDGE_CURVE ( 'NONE', #128448, #120284, #128388, .T. ) ;
#63008 = ORIENTED_EDGE ( 'NONE', *, *, #121214, .T. ) ;
#63009 = VERTEX_POINT ( 'NONE', #29521 ) ;
#63010 = LINE ( 'NONE', #20521, #25466 ) ;
#63011 = ADVANCED_FACE ( 'NONE', ( #18406 ), #116616, .T. ) ;
#63012 = ORIENTED_EDGE ( 'NONE', *, *, #68458, .T. ) ;
#63013 = EDGE_CURVE ( 'NONE', #13525, #4435, #99559, .T. ) ;
#63014 = EDGE_LOOP ( 'NONE', ( #84515, #78850, #81323, #53714 ) ) ;
#63015 = EDGE_CURVE ( 'NONE', #67345, #22620, #26740, .T. ) ;
#63016 = ORIENTED_EDGE ( 'NONE', *, *, #118755, .T. ) ;
#63017 = EDGE_CURVE ( 'NONE', #33832, #24400, #57698, .T. ) ;
#63018 = SURFACE_SIDE_STYLE ('',( #91190 ) ) ;
#63019 = CARTESIAN_POINT ( 'NONE',  ( -14.34999999999998543, 12.50000000000000000, -2.511473670974875727 ) ) ;
#63020 = DIRECTION ( 'NONE',  ( -0.000000000000000000, 1.000000000000000000, -0.000000000000000000 ) ) ;
#63021 = DIRECTION ( 'NONE',  ( 0.000000000000000000, 0.000000000000000000, -1.000000000000000000 ) ) ;
#63022 = ADVANCED_FACE ( 'NONE', ( #108715 ), #72714, .T. ) ;
#63023 = LINE ( 'NONE', #4091, #109429 ) ;
#63024 = ADVANCED_FACE ( 'NONE', ( #110021 ), #83142, .T. ) ;
#63025 = DIRECTION ( 'NONE',  ( 0.000000000000000000, 0.000000000000000000, 1.000000000000000000 ) ) ;
#63026 = VECTOR ( 'NONE', #55488, 1000.000000000000000 ) ;
#63027 = AXIS2_PLACEMENT_3D ( 'NONE', #85396, #125321, #95866 ) ;
#63028 = ORIENTED_EDGE ( 'NONE', *, *, #70170, .T. ) ;
#63029 = CARTESIAN_POINT ( 'NONE',  ( -6.450000000000017941, 12.50000000000000000, -6.841600689897077814 ) ) ;
#63030 = EDGE_CURVE ( 'NONE', #128895, #110043, #12153, .T. ) ;
#63031 = VERTEX_POINT ( 'NONE', #71355 ) ;
#63032 = DIRECTION ( 'NONE',  ( 0.000000000000000000, -1.000000000000000000, 0.000000000000000000 ) ) ;
#63033 = ORIENTED_EDGE ( 'NONE', *, *, #27831, .F. ) ;
#63034 = EDGE_CURVE ( 'NONE', #16842, #123754, #81132, .T. ) ;
#63035 = ORIENTED_EDGE ( 'NONE', *, *, #21666, .F. ) ;
#63037 = EDGE_CURVE ( 'NONE', #6359, #66455, #120834, .T. ) ;
#63036 = VECTOR ( 'NONE', #19610, 1000.000000000000000 ) ;
#63038 = DIRECTION ( 'NONE',  ( 0.000000000000000000, -0.9999939076577903929, 0.003490651415223739937 ) ) ;
#63039 = AXIS2_PLACEMENT_3D ( 'NONE', #106014, #26807, #125003 ) ;
#63040 = AXIS2_PLACEMENT_3D ( 'NONE', #77679, #65932, #27951 ) ;
#63041 = CARTESIAN_POINT ( 'NONE',  ( -3.950000000000028155, 2.500000000000000000, -6.941600689897077459 ) ) ;
#63042 = ORIENTED_EDGE ( 'NONE', *, *, #28461, .T. ) ;
#63043 = VERTEX_POINT ( 'NONE', #82499 ) ;
#63044 = CARTESIAN_POINT ( 'NONE',  ( 3.749999999999940492, 2.500000000000000000, 2.857883832488649301 ) ) ;
#63045 = CARTESIAN_POINT ( 'NONE',  ( 5.399999999999933742, 12.50000000000000000, -2.385244779468109755E-15 ) ) ;
#63046 = FACE_OUTER_BOUND ( 'NONE', #78855, .T. ) ;
#63047 = DIRECTION ( 'NONE',  ( -0.000000000000000000, 1.000000000000000000, -0.000000000000000000 ) ) ;
#63048 = VECTOR ( 'NONE', #42314, 1000.000000000000000 ) ;
#63049 = CONICAL_SURFACE ( 'NONE', #71432, 0.1000000000000002554, 0.003490658503988666988 ) ;
#63050 = FACE_OUTER_BOUND ( 'NONE', #114319, .T. ) ;
#63051 = EDGE_LOOP ( 'NONE', ( #90180, #110030, #66479, #27876 ) ) ;
#63052 = CARTESIAN_POINT ( 'NONE',  ( -5.850000000000021849, 2.500000000000000000, -7.188010851410854052 ) ) ;
#63053 = AXIS2_PLACEMENT_3D ( 'NONE', #17476, #50200, #19412 ) ;
#63054 = AXIS2_PLACEMENT_3D ( 'NONE', #41547, #81458, #121362 ) ;
#63055 = ORIENTED_EDGE ( 'NONE', *, *, #122697, .T. ) ;
#63056 = DIRECTION ( 'NONE',  ( 0.000000000000000000, 0.000000000000000000, 1.000000000000000000 ) ) ;
#63057 = FACE_OUTER_BOUND ( 'NONE', #74834, .T. ) ;
#63058 = AXIS2_PLACEMENT_3D ( 'NONE', #81315, #122527, #40768 ) ;
#63059 = AXIS2_PLACEMENT_3D ( 'NONE', #69125, #59991, #70428 ) ;
#63060 = CARTESIAN_POINT ( 'NONE',  ( 185.1302083336747160, -4.367472073101514418, -7.564683531250002702 ) ) ;
#63061 = DIRECTION ( 'NONE',  ( 0.000000000000000000, -0.9999939076577903929, 0.003490651415223739937 ) ) ;
#63062 = FACE_OUTER_BOUND ( 'NONE', #122489, .T. ) ;
#63063 = DIRECTION ( 'NONE',  ( -0.000000000000000000, 1.000000000000000000, -0.000000000000000000 ) ) ;
#63064 = CARTESIAN_POINT ( 'NONE',  ( 4.149999999999938183, 2.500000000000000000, 2.165063509461097713 ) ) ;
#63065 = ORIENTED_EDGE ( 'NONE', *, *, #123171, .F. ) ;
#63067 = EDGE_CURVE ( 'NONE', #118565, #56267, #51886, .T. ) ;
#63066 = CARTESIAN_POINT ( 'NONE',  ( -12.89999999999999325, 2.500000000000000000, -3.537306695894647302 ) ) ;
#63068 = CARTESIAN_POINT ( 'NONE',  ( -6.650000000000014566, 2.500000000000000000, 1.472243186433545459 ) ) ;
#63069 = DIRECTION ( 'NONE',  ( 0.000000000000000000, 0.000000000000000000, 1.000000000000000000 ) ) ;
#63070 = EDGE_CURVE ( 'NONE', #43290, #850, #129177, .T. ) ;
#63071 = ORIENTED_EDGE ( 'NONE', *, *, #23366, .T. ) ;
#63072 = DIRECTION ( 'NONE',  ( -0.000000000000000000, -1.000000000000000000, -0.000000000000000000 ) ) ;
#63073 = ORIENTED_EDGE ( 'NONE', *, *, #58574, .T. ) ;
#63074 = ORIENTED_EDGE ( 'NONE', *, *, #39272, .T. ) ;
#63075 = CARTESIAN_POINT ( 'NONE',  ( -9.800000000000006040, 2.500000000000000000, 0.3464101615137735735 ) ) ;
#63076 = AXIS2_PLACEMENT_3D ( 'NONE', #88857, #120262, #80336 ) ;
#63077 = AXIS2_PLACEMENT_3D ( 'NONE', #109054, #70451, #20708 ) ;
#63078 = AXIS2_PLACEMENT_3D ( 'NONE', #125165, #44033, #75403 ) ;
#63079 = ORIENTED_EDGE ( 'NONE', *, *, #49690, .F. ) ;
#63080 = CARTESIAN_POINT ( 'NONE',  ( 20.80581321129333361, -0.6997403544382545526, -4.161084241360549107 ) ) ;
#63081 = FACE_OUTER_BOUND ( 'NONE', #94274, .T. ) ;
#63082 = CARTESIAN_POINT ( 'NONE',  ( -13.94999999999998685, 12.50000000000000000, -2.446380397790838046 ) ) ;
#63083 = ORIENTED_EDGE ( 'NONE', *, *, #57259, .F. ) ;
#63084 = CARTESIAN_POINT ( 'NONE',  ( -13.09999999999999254, 2.500000000000000000, 0.4464101615137777701 ) ) ;
#63085 = AXIS2_PLACEMENT_3D ( 'NONE', #76686, #53348, #56386 ) ;
#63086 = PLANE ( 'NONE',  #99734 ) ;
#63087 = CIRCLE ( 'NONE', #17082, 0.06509327318403745899 ) ;
#63088 = AXIS2_PLACEMENT_3D ( 'NONE', #113455, #12660, #51974 ) ;
#63089 = VERTEX_POINT ( 'NONE', #1977 ) ;
#63090 = CIRCLE ( 'NONE', #50566, 0.1000000000000000472 ) ;
#63091 = ORIENTED_EDGE ( 'NONE', *, *, #43513, .T. ) ;
#63092 = ORIENTED_EDGE ( 'NONE', *, *, #125327, .F. ) ;
#63093 = DIRECTION ( 'NONE',  ( 0.000000000000000000, 1.000000000000000000, 0.000000000000000000 ) ) ;
#63094 = LINE ( 'NONE', #82758, #73049 ) ;
#63095 = CARTESIAN_POINT ( 'NONE',  ( -4.150000000000024336, 12.50000000000000000, -2.792790559304616504 ) ) ;
#63096 = VERTEX_POINT ( 'NONE', #100814 ) ;
#63097 = CARTESIAN_POINT ( 'NONE',  ( -1.250000000000001110, 2.500000000000000000, -6.495190528383302464 ) ) ;
#63098 = CARTESIAN_POINT ( 'NONE',  ( 2.099999999999948574, 2.500000000000000000, 3.737306695894644371 ) ) ;
#63099 = ORIENTED_EDGE ( 'NONE', *, *, #50726, .F. ) ;
#63101 = ADVANCED_FACE ( 'NONE', ( #13072 ), #16247, .T. ) ;
#63100 = CARTESIAN_POINT ( 'NONE',  ( -10.85000000000000142, 2.500000000000000000, -2.757883832488650100 ) ) ;
#63102 = CARTESIAN_POINT ( 'NONE',  ( 9.599999999999917932, 12.50000000000000000, -0.6928203230275541413 ) ) ;
#63103 = CARTESIAN_POINT ( 'NONE',  ( 1.649999999999951505, 12.50000000000000000, -2.857883832488653741 ) ) ;
#63104 = CARTESIAN_POINT ( 'NONE',  ( 3.099999999999945022, 12.50000000000000000, -4.741630453620016006 ) ) ;
#63105 = DIRECTION ( 'NONE',  ( -0.000000000000000000, -1.000000000000000000, -0.000000000000000000 ) ) ;
#63106 = FACE_OUTER_BOUND ( 'NONE', #29690, .T. ) ;
#63107 = DIRECTION ( 'NONE',  ( 0.000000000000000000, 1.000000000000000000, 0.000000000000000000 ) ) ;
#63108 = EDGE_CURVE ( 'NONE', #33313, #78466, #118768, .T. ) ;
#63109 = CIRCLE ( 'NONE', #125791, 0.1000000000000000056 ) ;
#63110 = ORIENTED_EDGE ( 'NONE', *, *, #26404, .F. ) ;
#63111 = ORIENTED_EDGE ( 'NONE', *, *, #46765, .F. ) ;
#63112 = EDGE_LOOP ( 'NONE', ( #5551, #64776, #44288, #63099 ) ) ;
#63113 = ORIENTED_EDGE ( 'NONE', *, *, #9962, .F. ) ;
#63114 = DIRECTION ( 'NONE',  ( 0.000000000000000000, 0.000000000000000000, -1.000000000000000000 ) ) ;
#63115 = LINE ( 'NONE', #114158, #97953 ) ;
#63116 = EDGE_CURVE ( 'NONE', #17230, #85684, #102056, .T. ) ;
#63117 = CARTESIAN_POINT ( 'NONE',  ( 7.299999999999926104, 2.500000000000000000, 4.676537180435972552 ) ) ;
#63118 = ORIENTED_EDGE ( 'NONE', *, *, #96712, .F. ) ;
#63119 = FACE_BOUND ( 'NONE', #71458, .T. ) ;
#63120 = ADVANCED_FACE ( 'NONE', ( #22926 ), #93644, .T. ) ;
#63121 = VECTOR ( 'NONE', #50217, 1000.000000000000000 ) ;
#63122 = DIRECTION ( 'NONE',  ( -4.274815082592931898E-19, -0.9999939076577903929, -0.003490651415223739937 ) ) ;
#63123 = FACE_OUTER_BOUND ( 'NONE', #57323, .T. ) ;
#63124 = CIRCLE ( 'NONE', #29680, 0.09999999999999982514 ) ;
#63125 = DIRECTION ( 'NONE',  ( 0.000000000000000000, 0.000000000000000000, -1.000000000000000000 ) ) ;
#63126 = CARTESIAN_POINT ( 'NONE',  ( 13.29999999999989946, 2.500000000000000000, -2.385244779468109755E-15 ) ) ;
#63127 = DIRECTION ( 'NONE',  ( -4.274815082592931898E-19, -0.9999939076577903929, -0.003490651415223739937 ) ) ;
#63128 = DIRECTION ( 'NONE',  ( -4.274815082592931898E-19, -0.9999939076577903929, -0.003490651415223739937 ) ) ;
#63129 = DIRECTION ( 'NONE',  ( 0.000000000000000000, 0.000000000000000000, 1.000000000000000000 ) ) ;
#63130 = DIRECTION ( 'NONE',  ( 0.000000000000000000, 0.000000000000000000, 1.000000000000000000 ) ) ;
#63131 = ADVANCED_FACE ( 'NONE', ( #92960 ), #3280, .T. ) ;
#63132 = DIRECTION ( 'NONE',  ( 0.000000000000000000, 0.000000000000000000, -1.000000000000000000 ) ) ;
#63133 = CIRCLE ( 'NONE', #90302, 0.06509327318403743123 ) ;
#63134 = ORIENTED_EDGE ( 'NONE', *, *, #43425, .F. ) ;
#63135 = CIRCLE ( 'NONE', #60981, 0.1000000000000002554 ) ;
#63136 = ORIENTED_EDGE ( 'NONE', *, *, #68211, .T. ) ;
#63137 = ORIENTED_EDGE ( 'NONE', *, *, #100229, .T. ) ;
#63138 = EDGE_LOOP ( 'NONE', ( #45271, #23874, #73928, #2362 ) ) ;
#63140 = ORIENTED_EDGE ( 'NONE', *, *, #104529, .T. ) ;
#63139 = AXIS2_PLACEMENT_3D ( 'NONE', #49929, #59090, #9335 ) ;
#63141 = AXIS2_PLACEMENT_3D ( 'NONE', #91183, #1502, #100996 ) ;
#63142 = CIRCLE ( 'NONE', #98935, 0.06509327318403745899 ) ;
#63143 = EDGE_LOOP ( 'NONE', ( #45475, #55202, #9640, #122650 ) ) ;
#63144 = CARTESIAN_POINT ( 'NONE',  ( -8.150000000000012790, 2.500000000000000000, 1.918653347947321564 ) ) ;
#63145 = ORIENTED_EDGE ( 'NONE', *, *, #65200, .T. ) ;
#63146 = VERTEX_POINT ( 'NONE', #23559 ) ;
#63147 = AXIS2_PLACEMENT_3D ( 'NONE', #36714, #77269, #117164 ) ;
#63148 = AXIS2_PLACEMENT_3D ( 'NONE', #28192, #96916, #39328 ) ;
#63149 = CARTESIAN_POINT ( 'NONE',  ( 9.399999999999915090, 12.50000000000000000, -4.611443907251939756 ) ) ;
#63150 = DIRECTION ( 'NONE',  ( -0.000000000000000000, -1.000000000000000000, -0.000000000000000000 ) ) ;
#63151 = PLANE ( 'NONE',  #46785 ) ;
#63152 = EDGE_LOOP ( 'NONE', ( #24578, #5347 ) ) ;
#63153 = DIRECTION ( 'NONE',  ( 0.000000000000000000, -0.000000000000000000, 1.000000000000000000 ) ) ;
#63154 = ORIENTED_EDGE ( 'NONE', *, *, #86997, .T. ) ;
#63155 = EDGE_CURVE ( 'NONE', #14213, #81272, #43479, .T. ) ;
#63156 = ORIENTED_EDGE ( 'NONE', *, *, #18915, .F. ) ;
#63157 = CARTESIAN_POINT ( 'NONE',  ( -12.09999999999999609, 12.50000000000000000, -3.637306695894647390 ) ) ;
#63158 = DIRECTION ( 'NONE',  ( -0.000000000000000000, -1.000000000000000000, -0.000000000000000000 ) ) ;
#63159 = ADVANCED_FACE ( 'NONE', ( #121753 ), #5879, .T. ) ;
#63160 = ORIENTED_EDGE ( 'NONE', *, *, #23880, .T. ) ;
#63162 = EDGE_CURVE ( 'NONE', #129597, #94263, #3915, .T. ) ;
#63161 = ORIENTED_EDGE ( 'NONE', *, *, #127465, .F. ) ;
#63163 = LINE ( 'NONE', #125310, #92356 ) ;
#63164 = DIRECTION ( 'NONE',  ( 0.000000000000000000, 1.000000000000000000, 0.000000000000000000 ) ) ;
#63165 = DIRECTION ( 'NONE',  ( -0.000000000000000000, -1.000000000000000000, -0.000000000000000000 ) ) ;
#63167 = CARTESIAN_POINT ( 'NONE',  ( -3.300000000000028244, 2.500000000000000000, 4.430127018922196847 ) ) ;
#63166 = VECTOR ( 'NONE', #92728, 1000.000000000000000 ) ;
#63168 = AXIS2_PLACEMENT_3D ( 'NONE', #89705, #100177, #31 ) ;
#63169 = ADVANCED_FACE ( 'NONE', ( #111955 ), #70729, .T. ) ;
#63170 = VECTOR ( 'NONE', #118554, 1000.000000000000000 ) ;
#63171 = EDGE_CURVE ( 'NONE', #118, #54102, #5788, .T. ) ;
#63172 = FACE_OUTER_BOUND ( 'NONE', #115692, .T. ) ;
#63173 = ADVANCED_FACE ( 'NONE', ( #101487 ), #95705, .T. ) ;
#63174 = EDGE_CURVE ( 'NONE', #84243, #14399, #54310, .T. ) ;
#63175 = ORIENTED_EDGE ( 'NONE', *, *, #50547, .F. ) ;
#63176 = CARTESIAN_POINT ( 'NONE',  ( 8.920123399827042832, -2.500000000000000000, 8.410822907074534172 ) ) ;
#63177 = CIRCLE ( 'NONE', #31792, 0.06509327318403745899 ) ;
#63179 = ORIENTED_EDGE ( 'NONE', *, *, #72059, .T. ) ;
#63178 = CIRCLE ( 'NONE', #48513, 0.09999999999999999167 ) ;
#63180 = CARTESIAN_POINT ( 'NONE',  ( 7.899999999999923084, 12.50000000000000000, -0.6928203230275542523 ) ) ;
#63181 = CIRCLE ( 'NONE', #111272, 0.06509327318403745899 ) ;
#63182 = EDGE_CURVE ( 'NONE', #24862, #97815, #127103, .T. ) ;
#63183 = EDGE_LOOP ( 'NONE', ( #13850, #85641, #26512, #46206 ) ) ;
#63184 = CARTESIAN_POINT ( 'NONE',  ( 7.949999999999925571, 12.50000000000000000, -6.495190528383302464 ) ) ;
#63185 = CARTESIAN_POINT ( 'NONE',  ( 127.5000000000000000, 9.429780353434619030E-16, -7.700000000000000178 ) ) ;
#63186 = CIRCLE ( 'NONE', #81951, 0.1000000000000000472 ) ;
#63187 = AXIS2_PLACEMENT_3D ( 'NONE', #126277, #124346, #56862 ) ;
#63188 = DIRECTION ( 'NONE',  ( -4.274815082592931898E-19, -0.9999939076577903929, -0.003490651415223739937 ) ) ;
#63189 = DIRECTION ( 'NONE',  ( 0.000000000000000000, 0.000000000000000000, -1.000000000000000000 ) ) ;
#63190 = EDGE_LOOP ( 'NONE', ( #71775, #45060 ) ) ;
#63191 = EDGE_CURVE ( 'NONE', #39789, #118565, #44486, .T. ) ;
#63192 = AXIS2_PLACEMENT_3D ( 'NONE', #126792, #113755, #124856 ) ;
#63193 = DIRECTION ( 'NONE',  ( 0.000000000000000000, -0.000000000000000000, 1.000000000000000000 ) ) ;
#63194 = DIRECTION ( 'NONE',  ( 0.000000000000000000, 0.000000000000000000, -1.000000000000000000 ) ) ;
#63195 = ORIENTED_EDGE ( 'NONE', *, *, #5321, .F. ) ;
#63196 = ORIENTED_EDGE ( 'NONE', *, *, #8158, .T. ) ;
#63197 = ORIENTED_EDGE ( 'NONE', *, *, #1862, .F. ) ;
#63198 = PLANE ( 'NONE',  #12048 ) ;
#63199 = CARTESIAN_POINT ( 'NONE',  ( -13.34999999999999076, 2.500000000000000000, -2.957883832488651610 ) ) ;
#63200 = CARTESIAN_POINT ( 'NONE',  ( 185.5677083336747160, -4.367472073101514418, -7.564683531250002702 ) ) ;
#63201 = DIRECTION ( 'NONE',  ( 0.000000000000000000, 0.000000000000000000, 1.000000000000000000 ) ) ;
#63202 = DIRECTION ( 'NONE',  ( 0.000000000000000000, -0.9999939076577903929, 0.003490651415223739937 ) ) ;
#63203 = CARTESIAN_POINT ( 'NONE',  ( 5.649999999999934630, 2.500000000000000000, 6.248780366869521430 ) ) ;
#63204 = DIRECTION ( 'NONE',  ( 1.000000000000000000, -0.000000000000000000, -0.000000000000000000 ) ) ;
#63205 = VECTOR ( 'NONE', #9456, 1000.000000000000000 ) ;
#63206 = ORIENTED_EDGE ( 'NONE', *, *, #16603, .F. ) ;
#63207 = CARTESIAN_POINT ( 'NONE',  ( -6.249999999999984901, 2.500000000000000000, -6.595190528383302109 ) ) ;
#63208 = ORIENTED_EDGE ( 'NONE', *, *, #37308, .F. ) ;
#63209 = DIRECTION ( 'NONE',  ( 0.000000000000000000, -0.000000000000000000, 1.000000000000000000 ) ) ;
#63210 = DIRECTION ( 'NONE',  ( -0.000000000000000000, -1.000000000000000000, -0.000000000000000000 ) ) ;
#63211 = CARTESIAN_POINT ( 'NONE',  ( 5.649999999999934630, 12.50000000000000000, -2.511473670974877948 ) ) ;
#63212 = CARTESIAN_POINT ( 'NONE',  ( 7.699999999999925571, 12.50000000000000000, -4.676537180435978769 ) ) ;
#63213 = AXIS2_PLACEMENT_3D ( 'NONE', #120008, #121293, #10665 ) ;
#63214 = EDGE_LOOP ( 'NONE', ( #33500, #113628 ) ) ;
#63215 = DIRECTION ( 'NONE',  ( -4.274815082592931898E-19, -0.9999939076577903929, -0.003490651415223739937 ) ) ;
#63216 = VECTOR ( 'NONE', #80041, 1000.000000000000000 ) ;
#63217 = AXIS2_PLACEMENT_3D ( 'NONE', #20557, #108910, #100406 ) ;
#63218 = EDGE_CURVE ( 'NONE', #60850, #65138, #14998, .T. ) ;
#63219 = DIRECTION ( 'NONE',  ( -4.274815082592931898E-19, -0.9999939076577903929, -0.003490651415223739937 ) ) ;
#63221 = ORIENTED_EDGE ( 'NONE', *, *, #13698, .F. ) ;
#63220 = DIRECTION ( 'NONE',  ( -0.000000000000000000, -1.000000000000000000, -0.000000000000000000 ) ) ;
#63222 = AXIS2_PLACEMENT_3D ( 'NONE', #14442, #103494, #13800 ) ;
#63223 = ORIENTED_EDGE ( 'NONE', *, *, #19870, .F. ) ;
#63225 = CONICAL_SURFACE ( 'NONE', #29777, 0.1000000000000002554, 0.003490658503988666988 ) ;
#63224 = CARTESIAN_POINT ( 'NONE',  ( -12.09999999999999609, 2.500000000000000000, -0.5928203230275500557 ) ) ;
#63226 = ADVANCED_FACE ( 'NONE', ( #84411 ), #124985, .T. ) ;
#63227 = ORIENTED_EDGE ( 'NONE', *, *, #93893, .T. ) ;
#63228 = VECTOR ( 'NONE', #106631, 1000.000000000000000 ) ;
#63230 = ORIENTED_EDGE ( 'NONE', *, *, #20478, .F. ) ;
#63229 = AXIS2_PLACEMENT_3D ( 'NONE', #81216, #30839, #51754 ) ;
#63231 = CONICAL_SURFACE ( 'NONE', #71547, 0.1000000000000000056, 0.003490658503988666988 ) ;
#63232 = DIRECTION ( 'NONE',  ( 0.000000000000000000, 0.000000000000000000, 1.000000000000000000 ) ) ;
#63234 = ORIENTED_EDGE ( 'NONE', *, *, #18645, .T. ) ;
#63233 = VECTOR ( 'NONE', #75183, 1000.000000000000000 ) ;
#63235 = DIRECTION ( 'NONE',  ( 0.000000000000000000, -0.9999939076577903929, 0.003490651415223739937 ) ) ;
#63236 = DIRECTION ( 'NONE',  ( 0.000000000000000000, -0.000000000000000000, 1.000000000000000000 ) ) ;
#63237 = DIRECTION ( 'NONE',  ( 0.000000000000000000, 1.000000000000000000, 0.000000000000000000 ) ) ;
#63238 = EDGE_LOOP ( 'NONE', ( #123870, #16168 ) ) ;
#63239 = CIRCLE ( 'NONE', #44363, 0.06509327318403745899 ) ;
#63240 = CARTESIAN_POINT ( 'NONE',  ( -1.850000000000033840, 2.500000000000000000, 6.048780366869521252 ) ) ;
#63242 = VERTEX_POINT ( 'NONE', #34695 ) ;
#63241 = DIRECTION ( 'NONE',  ( 0.000000000000000000, 1.000000000000000000, 0.000000000000000000 ) ) ;
#63243 = LINE ( 'NONE', #81589, #79842 ) ;
#63244 = DIRECTION ( 'NONE',  ( -0.000000000000000000, 1.000000000000000000, -0.000000000000000000 ) ) ;
#63245 = ORIENTED_EDGE ( 'NONE', *, *, #14034, .T. ) ;
#63246 = ORIENTED_EDGE ( 'NONE', *, *, #4510, .F. ) ;
#63247 = ORIENTED_EDGE ( 'NONE', *, *, #127753, .F. ) ;
#63248 = ORIENTED_EDGE ( 'NONE', *, *, #50395, .T. ) ;
#63249 = DIRECTION ( 'NONE',  ( 0.000000000000000000, 0.000000000000000000, -1.000000000000000000 ) ) ;
#63250 = DIRECTION ( 'NONE',  ( 0.000000000000000000, 0.000000000000000000, 1.000000000000000000 ) ) ;
#63251 = CARTESIAN_POINT ( 'NONE',  ( 195.5000000000000000, 0.000000000000000000, -7.541925104783893552 ) ) ;
#63252 = FACE_BOUND ( 'NONE', #5187, .T. ) ;
#63253 = VERTEX_POINT ( 'NONE', #35962 ) ;
#63254 = CARTESIAN_POINT ( 'NONE',  ( 185.1145833340161175, 6.668395609140177704, -3.849999999999998312 ) ) ;
#63255 = CARTESIAN_POINT ( 'NONE',  ( -12.09999999999999609, 2.500000000000000000, -0.09999999999999827083 ) ) ;
#63256 = LINE ( 'NONE', #92063, #29201 ) ;
#63257 = EDGE_CURVE ( 'NONE', #103010, #115225, #114507, .T. ) ;
#63258 = AXIS2_PLACEMENT_3D ( 'NONE', #3896, #43852, #24194 ) ;
#63259 = DIRECTION ( 'NONE',  ( 0.000000000000000000, 0.000000000000000000, 1.000000000000000000 ) ) ;
#63260 = CARTESIAN_POINT ( 'NONE',  ( -11.44999999999999751, 2.500000000000000000, 1.718653347947321386 ) ) ;
#63261 = DIRECTION ( 'NONE',  ( 0.000000000000000000, 0.000000000000000000, 1.000000000000000000 ) ) ;
#63262 = EDGE_CURVE ( 'NONE', #25742, #47551, #30970, .T. ) ;
#63263 = CIRCLE ( 'NONE', #56984, 0.06509327318403745899 ) ;
#63264 = DIRECTION ( 'NONE',  ( -0.000000000000000000, -1.000000000000000000, -0.000000000000000000 ) ) ;
#63265 = AXIS2_PLACEMENT_3D ( 'NONE', #6196, #75585, #15369 ) ;
#63266 = ORIENTED_EDGE ( 'NONE', *, *, #29726, .T. ) ;
#63267 = VERTEX_POINT ( 'NONE', #94880 ) ;
#63268 = EDGE_LOOP ( 'NONE', ( #75121, #25935 ) ) ;
#63269 = VERTEX_POINT ( 'NONE', #5192 ) ;
#63270 = ORIENTED_EDGE ( 'NONE', *, *, #106007, .F. ) ;
#63271 = CARTESIAN_POINT ( 'NONE',  ( 0.000000000000000000, 5.000000000000000000, 0.000000000000000000 ) ) ;
#63272 = CONICAL_SURFACE ( 'NONE', #36192, 0.09999999999999982514, 0.003490658503988666988 ) ;
#63273 = EDGE_CURVE ( 'NONE', #43734, #82187, #66698, .T. ) ;
#63274 = FACE_OUTER_BOUND ( 'NONE', #100095, .T. ) ;
#63275 = VERTEX_POINT ( 'NONE', #6458 ) ;
#63276 = FACE_BOUND ( 'NONE', #107242, .T. ) ;
#63277 = ADVANCED_FACE ( 'NONE', ( #47083 ), #108394, .T. ) ;
#63278 = AXIS2_PLACEMENT_3D ( 'NONE', #7642, #27284, #128748 ) ;
#63279 = CARTESIAN_POINT ( 'NONE',  ( 8.099999999999923261, 2.500000000000000000, -4.676537180435978769 ) ) ;
#63280 = EDGE_CURVE ( 'NONE', #123030, #35299, #114650, .T. ) ;
#63281 = VERTEX_POINT ( 'NONE', #15653 ) ;
#63282 = DIRECTION ( 'NONE',  ( -0.000000000000000000, 1.000000000000000000, -0.000000000000000000 ) ) ;
#63283 = DIRECTION ( 'NONE',  ( 0.000000000000000000, 0.000000000000000000, 1.000000000000000000 ) ) ;
#63284 = EDGE_CURVE ( 'NONE', #5264, #17021, #25478, .T. ) ;
#63285 = CARTESIAN_POINT ( 'NONE',  ( -2.900000000000030553, 2.500000000000000000, 5.122947341949749323 ) ) ;
#63286 = VERTEX_POINT ( 'NONE', #104683 ) ;
#63287 = ORIENTED_EDGE ( 'NONE', *, *, #94241, .T. ) ;
#63288 = VERTEX_POINT ( 'NONE', #24211 ) ;
#63289 = ORIENTED_EDGE ( 'NONE', *, *, #84249, .T. ) ;
#63290 = DIRECTION ( 'NONE',  ( 0.000000000000000000, 1.000000000000000000, 0.000000000000000000 ) ) ;
#63291 = DIRECTION ( 'NONE',  ( -4.274815082592931898E-19, -0.9999939076577903929, -0.003490651415223739937 ) ) ;
#63292 = CARTESIAN_POINT ( 'NONE',  ( 6.849999999999930367, 12.50000000000000000, -6.083687093685488989 ) ) ;
#63293 = EDGE_LOOP ( 'NONE', ( #127610, #124500, #109224, #66908 ) ) ;
#63294 = CARTESIAN_POINT ( 'NONE',  ( 10.19999999999991047, 2.500000000000000000, 4.676537180435972552 ) ) ;
#63295 = CONICAL_SURFACE ( 'NONE', #50781, 0.1000000000000002554, 0.003490658503988666988 ) ;
#63296 = VECTOR ( 'NONE', #18018, 1000.000000000000000 ) ;
#63298 = DIRECTION ( 'NONE',  ( 0.000000000000000000, -0.000000000000000000, 1.000000000000000000 ) ) ;
#63297 = CIRCLE ( 'NONE', #13104, 0.06509327318403745899 ) ;
#63299 = DIRECTION ( 'NONE',  ( 0.000000000000000000, 1.000000000000000000, 0.000000000000000000 ) ) ;
#63300 = FACE_OUTER_BOUND ( 'NONE', #95338, .T. ) ;
#63301 = ORIENTED_EDGE ( 'NONE', *, *, #95996, .T. ) ;
#63302 = CARTESIAN_POINT ( 'NONE',  ( -1.850000000000033840, 12.50000000000000000, 2.511473670974873507 ) ) ;
#63303 = AXIS2_PLACEMENT_3D ( 'NONE', #125692, #66779, #115212 ) ;
#63304 = ORIENTED_EDGE ( 'NONE', *, *, #68057, .T. ) ;
#63305 = DIRECTION ( 'NONE',  ( 0.000000000000000000, 0.000000000000000000, 1.000000000000000000 ) ) ;
#63306 = VECTOR ( 'NONE', #67999, 1000.000000000000000 ) ;
#63307 = AXIS2_PLACEMENT_3D ( 'NONE', #51879, #92433, #74087 ) ;
#63308 = EDGE_LOOP ( 'NONE', ( #87432, #110618, #53641, #22498 ) ) ;
#63309 = ORIENTED_EDGE ( 'NONE', *, *, #115511, .F. ) ;
#63310 = DIRECTION ( 'NONE',  ( -4.274815082592931898E-19, -0.9999939076577903929, -0.003490651415223739937 ) ) ;
#63311 = FACE_OUTER_BOUND ( 'NONE', #119371, .T. ) ;
#63312 = DIRECTION ( 'NONE',  ( 0.000000000000000000, 1.000000000000000000, 0.000000000000000000 ) ) ;
#63313 = DIRECTION ( 'NONE',  ( 0.000000000000000000, 1.000000000000000000, 0.000000000000000000 ) ) ;
#63314 = DIRECTION ( 'NONE',  ( -0.000000000000000000, 1.000000000000000000, -0.000000000000000000 ) ) ;
#63315 = VECTOR ( 'NONE', #111876, 1000.000000000000000 ) ;
#63316 = ORIENTED_EDGE ( 'NONE', *, *, #110213, .F. ) ;
#63317 = EDGE_LOOP ( 'NONE', ( #90031, #38068 ) ) ;
#63318 = DIRECTION ( 'NONE',  ( 0.000000000000000000, 0.000000000000000000, -1.000000000000000000 ) ) ;
#63320 = CIRCLE ( 'NONE', #84239, 0.1000000000000000472 ) ;
#63319 = FACE_OUTER_BOUND ( 'NONE', #10024, .T. ) ;
#63321 = CIRCLE ( 'NONE', #50815, 0.1000000000000000056 ) ;
#63322 = AXIS2_PLACEMENT_3D ( 'NONE', #12424, #112582, #1319 ) ;
#63324 = EDGE_CURVE ( 'NONE', #48575, #74213, #1774, .T. ) ;
#63323 = FACE_OUTER_BOUND ( 'NONE', #42228, .T. ) ;
#63325 = ORIENTED_EDGE ( 'NONE', *, *, #17763, .F. ) ;
#63326 = ORIENTED_EDGE ( 'NONE', *, *, #113129, .T. ) ;
#63327 = EDGE_CURVE ( 'NONE', #18996, #55517, #120917, .T. ) ;
#63328 = FACE_BOUND ( 'NONE', #45745, .T. ) ;
#63329 = VECTOR ( 'NONE', #32555, 1000.000000000000000 ) ;
#63330 = EDGE_CURVE ( 'NONE', #16632, #68129, #65409, .T. ) ;
#63331 = EDGE_CURVE ( 'NONE', #8330, #124875, #26835, .T. ) ;
#63332 = ORIENTED_EDGE ( 'NONE', *, *, #67265, .F. ) ;
#63333 = CARTESIAN_POINT ( 'NONE',  ( -4.350000000000023626, 12.50000000000000000, -2.511473670974877948 ) ) ;
#63334 = FACE_OUTER_BOUND ( 'NONE', #126490, .T. ) ;
#63335 = CARTESIAN_POINT ( 'NONE',  ( 0.7999999999999612976, 12.50000000000000000, 0.06509327318403732021 ) ) ;
#63336 = ORIENTED_EDGE ( 'NONE', *, *, #19982, .T. ) ;
#63337 = CONICAL_SURFACE ( 'NONE', #2673, 0.1000000000000002554, 0.003490658503988666988 ) ;
#63338 = CARTESIAN_POINT ( 'NONE',  ( -5.000000000000022204, 2.500000000000000000, -0.7928203230275542301 ) ) ;
#63340 = ADVANCED_FACE ( 'NONE', ( #76535 ), #77005, .T. ) ;
#63339 = CARTESIAN_POINT ( 'NONE',  ( 11.64999999999990443, 2.500000000000000000, -5.902370205355750521 ) ) ;
#63341 = CARTESIAN_POINT ( 'NONE',  ( -13.29999999999998828, 2.500000000000000000, 4.230127018922196669 ) ) ;
#63342 = CARTESIAN_POINT ( 'NONE',  ( -11.64999999999999680, 12.50000000000000000, 5.737276932171707422 ) ) ;
#63343 = DIRECTION ( 'NONE',  ( 0.000000000000000000, 0.000000000000000000, -1.000000000000000000 ) ) ;
#63344 = EDGE_LOOP ( 'NONE', ( #68027, #63028 ) ) ;
#63345 = EDGE_CURVE ( 'NONE', #98888, #122658, #68685, .T. ) ;
#63346 = LINE ( 'NONE', #33878, #90583 ) ;
#63347 = EDGE_CURVE ( 'NONE', #85021, #114482, #79174, .T. ) ;
#63348 = CARTESIAN_POINT ( 'NONE',  ( 4.399999999999940847, 12.50000000000000000, -4.676537180435977881 ) ) ;
#63349 = ORIENTED_EDGE ( 'NONE', *, *, #3558, .F. ) ;
#63350 = ORIENTED_EDGE ( 'NONE', *, *, #25814, .T. ) ;
#63351 = CONICAL_SURFACE ( 'NONE', #6878, 0.1000000000000002554, 0.003490658503988666988 ) ;
#63352 = CARTESIAN_POINT ( 'NONE',  ( 186.1718750003414016, 9.264065473108010111E-16, -7.564683531250000925 ) ) ;
#63353 = CARTESIAN_POINT ( 'NONE',  ( -13.74999999999998757, 12.50000000000000000, 1.472243186433549456 ) ) ;
#63354 = CARTESIAN_POINT ( 'NONE',  ( -9.600000000000008527, 2.500000000000000000, -4.922947341949749145 ) ) ;
#63355 = DIRECTION ( 'NONE',  ( -4.274815082592931898E-19, -0.9999939076577903929, -0.003490651415223739937 ) ) ;
#63356 = CARTESIAN_POINT ( 'NONE',  ( 12.89999999999989910, 12.50000000000000000, 0.7579135962115869374 ) ) ;
#63357 = VECTOR ( 'NONE', #49562, 1000.000000000000000 ) ;
#63358 = DIRECTION ( 'NONE',  ( -0.000000000000000000, -1.000000000000000000, -0.000000000000000000 ) ) ;
#63359 = CARTESIAN_POINT ( 'NONE',  ( -8.100000000000010303, 12.50000000000000000, 4.048810130592458201 ) ) ;
#63360 = CIRCLE ( 'NONE', #42442, 0.06509327318403745899 ) ;
#63361 = DIRECTION ( 'NONE',  ( -0.000000000000000000, 1.000000000000000000, -0.000000000000000000 ) ) ;
#63362 = DIRECTION ( 'NONE',  ( 0.000000000000000000, 1.000000000000000000, 0.000000000000000000 ) ) ;
#63364 = CONICAL_SURFACE ( 'NONE', #88477, 0.1000000000000000056, 0.003490658503988666988 ) ;
#63363 = CARTESIAN_POINT ( 'NONE',  ( -8.100000000000013856, 2.500000000000000000, 0.3464101615137736845 ) ) ;
#63365 = AXIS2_PLACEMENT_3D ( 'NONE', #45503, #44186, #84109 ) ;
#63366 = DIRECTION ( 'NONE',  ( 0.000000000000000000, 0.000000000000000000, 1.000000000000000000 ) ) ;
#63367 = ORIENTED_EDGE ( 'NONE', *, *, #98583, .F. ) ;
#63368 = VECTOR ( 'NONE', #7984, 1000.000000000000000 ) ;
#63369 = EDGE_LOOP ( 'NONE', ( #110399, #21462, #113468, #123207 ) ) ;
#63370 = CIRCLE ( 'NONE', #48798, 0.06509327318403745899 ) ;
#63371 = ORIENTED_EDGE ( 'NONE', *, *, #1802, .F. ) ;
#63372 = CIRCLE ( 'NONE', #21599, 0.06509327318403743123 ) ;
#63373 = CONICAL_SURFACE ( 'NONE', #75972, 0.09999999999999999167, 0.003490658503988666988 ) ;
#63374 = ORIENTED_EDGE ( 'NONE', *, *, #8004, .T. ) ;
#63375 = CARTESIAN_POINT ( 'NONE',  ( -11.64999999999999680, 12.50000000000000000, 6.430097255199259010 ) ) ;
#63376 = FACE_OUTER_BOUND ( 'NONE', #65602, .T. ) ;
#63377 = AXIS2_PLACEMENT_3D ( 'NONE', #85878, #117258, #115997 ) ;
#63378 = ORIENTED_EDGE ( 'NONE', *, *, #85536, .F. ) ;
#63379 = DIRECTION ( 'NONE',  ( 1.000000000000000000, 0.000000000000000000, -0.000000000000000000 ) ) ;
#63380 = DIRECTION ( 'NONE',  ( -0.000000000000000000, 1.000000000000000000, -0.000000000000000000 ) ) ;
#63382 = VERTEX_POINT ( 'NONE', #80243 ) ;
#63381 = LINE ( 'NONE', #103309, #28684 ) ;
#63383 = DIRECTION ( 'NONE',  ( 0.000000000000000000, 1.000000000000000000, 0.000000000000000000 ) ) ;
#63385 = DIRECTION ( 'NONE',  ( -0.000000000000000000, -1.000000000000000000, -0.000000000000000000 ) ) ;
#63384 = VECTOR ( 'NONE', #68871, 1000.000000000000000 ) ;
#63386 = VERTEX_POINT ( 'NONE', #129364 ) ;
#63387 = EDGE_CURVE ( 'NONE', #51338, #47295, #41622, .T. ) ;
#63388 = EDGE_LOOP ( 'NONE', ( #126211, #54962, #60325, #113350 ) ) ;
#63389 = EDGE_LOOP ( 'NONE', ( #17306, #82514, #123580, #38224 ) ) ;
#63390 = VERTEX_POINT ( 'NONE', #117076 ) ;
#63391 = CARTESIAN_POINT ( 'NONE',  ( 5.649999999999934630, 2.500000000000000000, 6.048780366869521252 ) ) ;
#63393 = LINE ( 'NONE', #14895, #11148 ) ;
#63392 = VECTOR ( 'NONE', #75773, 1000.000000000000000 ) ;
#63394 = DIRECTION ( 'NONE',  ( 0.000000000000000000, 0.000000000000000000, 1.000000000000000000 ) ) ;
#63395 = CIRCLE ( 'NONE', #92637, 0.1000000000000002554 ) ;
#63396 = DIRECTION ( 'NONE',  ( -0.000000000000000000, -1.000000000000000000, -0.000000000000000000 ) ) ;
#63397 = AXIS2_PLACEMENT_3D ( 'NONE', #31859, #61321, #122814 ) ;
#63398 = VERTEX_POINT ( 'NONE', #90037 ) ;
#63399 = CARTESIAN_POINT ( 'NONE',  ( -5.650000000000019895, 12.50000000000000000, 6.841600689897072485 ) ) ;
#63400 = ORIENTED_EDGE ( 'NONE', *, *, #109843, .F. ) ;
#63401 = LINE ( 'NONE', #12355, #64265 ) ;
#63402 = LINE ( 'NONE', #2522, #99919 ) ;
#63403 = LINE ( 'NONE', #94145, #71381 ) ;
#63404 = FACE_OUTER_BOUND ( 'NONE', #71335, .T. ) ;
#63405 = AXIS2_PLACEMENT_3D ( 'NONE', #107777, #19379, #59995 ) ;
#63406 = AXIS2_PLACEMENT_3D ( 'NONE', #28543, #29204, #126746 ) ;
#63407 = EDGE_LOOP ( 'NONE', ( #57974, #39879 ) ) ;
#63408 = CIRCLE ( 'NONE', #121994, 0.06509327318403745899 ) ;
#63409 = EDGE_LOOP ( 'NONE', ( #12145, #15414, #29121, #66028 ) ) ;
#63410 = EDGE_LOOP ( 'NONE', ( #33952, #25166, #103806, #70565 ) ) ;
#63411 = DIRECTION ( 'NONE',  ( 0.000000000000000000, 0.000000000000000000, -1.000000000000000000 ) ) ;
#63412 = LINE ( 'NONE', #53601, #106227 ) ;
#63413 = DIRECTION ( 'NONE',  ( -0.000000000000000000, -1.000000000000000000, -0.000000000000000000 ) ) ;
#63414 = FACE_BOUND ( 'NONE', #73481, .T. ) ;
#63415 = CARTESIAN_POINT ( 'NONE',  ( 5.849999999999933920, 2.500000000000000000, -2.165063509461101710 ) ) ;
#63416 = DIRECTION ( 'NONE',  ( -0.000000000000000000, -1.000000000000000000, -0.000000000000000000 ) ) ;
#63417 = CARTESIAN_POINT ( 'NONE',  ( 10.59999999999990905, 2.500000000000000000, 4.776537180435972196 ) ) ;
#63418 = AXIS2_PLACEMENT_3D ( 'NONE', #1577, #121352, #52614 ) ;
#63419 = AXIS2_PLACEMENT_3D ( 'NONE', #40182, #88626, #10069 ) ;
#63420 = AXIS2_PLACEMENT_3D ( 'NONE', #42397, #100645, #1170 ) ;
#63421 = FACE_OUTER_BOUND ( 'NONE', #10765, .T. ) ;
#63422 = DIRECTION ( 'NONE',  ( 0.000000000000000000, 1.000000000000000000, 0.000000000000000000 ) ) ;
#63423 = AXIS2_PLACEMENT_3D ( 'NONE', #15443, #74385, #85493 ) ;
#63424 = DIRECTION ( 'NONE',  ( -0.000000000000000000, 1.000000000000000000, -0.000000000000000000 ) ) ;
#63425 = ORIENTED_EDGE ( 'NONE', *, *, #21162, .T. ) ;
#63426 = EDGE_CURVE ( 'NONE', #39960, #7581, #104194, .T. ) ;
#63427 = DIRECTION ( 'NONE',  ( 0.000000000000000000, -0.9999939076577903929, 0.003490651415223739937 ) ) ;
#63428 = ORIENTED_EDGE ( 'NONE', *, *, #35685, .F. ) ;
#63429 = VERTEX_POINT ( 'NONE', #126927 ) ;
#63430 = EDGE_CURVE ( 'NONE', #31133, #18092, #31783, .T. ) ;
#63431 = LINE ( 'NONE', #113827, #19307 ) ;
#63432 = FACE_BOUND ( 'NONE', #68418, .T. ) ;
#63433 = ADVANCED_FACE ( 'NONE', ( #79593 ), #67316, .T. ) ;
#63434 = CARTESIAN_POINT ( 'NONE',  ( 1.049999999999954525, 2.500000000000000000, 1.818653347947321475 ) ) ;
#63435 = ADVANCED_FACE ( 'NONE', ( #100510 ), #47770, .T. ) ;
#63436 = EDGE_CURVE ( 'NONE', #97069, #121109, #70748, .T. ) ;
#63438 = ORIENTED_EDGE ( 'NONE', *, *, #35735, .T. ) ;
#63437 = AXIS2_PLACEMENT_3D ( 'NONE', #75241, #115809, #37269 ) ;
#63440 = CIRCLE ( 'NONE', #65482, 0.06509327318403745899 ) ;
#63439 = CARTESIAN_POINT ( 'NONE',  ( 26.76314062975745856, 1.072173157153399226, 4.440523076943353686 ) ) ;
#63441 = EDGE_CURVE ( 'NONE', #72699, #31251, #119502, .T. ) ;
#63442 = ADVANCED_FACE ( 'NONE', ( #40324 ), #51978, .T. ) ;
#63443 = DIRECTION ( 'NONE',  ( 0.000000000000000000, 0.000000000000000000, -1.000000000000000000 ) ) ;
#63444 = ADVANCED_FACE ( 'NONE', ( #59982 ), #101815, .T. ) ;
#63445 = VERTEX_POINT ( 'NONE', #10208 ) ;
#63446 = CARTESIAN_POINT ( 'NONE',  ( 6.849999999999929479, 12.50000000000000000, 6.148780366869520009 ) ) ;
#63447 = CARTESIAN_POINT ( 'NONE',  ( 186.5729166673494888, 4.445597072760099522, -7.700000000000035705 ) ) ;
#63448 = AXIS2_PLACEMENT_3D ( 'NONE', #60667, #52133, #100567 ) ;
#63449 = CIRCLE ( 'NONE', #105304, 0.06509327318403745899 ) ;
#63450 = AXIS2_PLACEMENT_3D ( 'NONE', #45739, #35284, #55557 ) ;
#63451 = VECTOR ( 'NONE', #76366, 1000.000000000000000 ) ;
#63452 = ORIENTED_EDGE ( 'NONE', *, *, #54719, .F. ) ;
#63453 = DIRECTION ( 'NONE',  ( -0.000000000000000000, -1.000000000000000000, -0.000000000000000000 ) ) ;
#63455 = EDGE_CURVE ( 'NONE', #106728, #71667, #97455, .T. ) ;
#63454 = DIRECTION ( 'NONE',  ( 0.000000000000000000, 0.000000000000000000, -1.000000000000000000 ) ) ;
#63456 = AXIS2_PLACEMENT_3D ( 'NONE', #40706, #82550, #72721 ) ;
#63458 = ORIENTED_EDGE ( 'NONE', *, *, #63561, .F. ) ;
#63457 = AXIS2_PLACEMENT_3D ( 'NONE', #111681, #122784, #82217 ) ;
#63459 = CONICAL_SURFACE ( 'NONE', #23760, 0.09999999999999999167, 0.003490658503988666988 ) ;
#63460 = CARTESIAN_POINT ( 'NONE',  ( -11.44999999999999751, 2.500000000000000000, 6.841600689897072485 ) ) ;
#63461 = DIRECTION ( 'NONE',  ( -0.000000000000000000, 1.000000000000000000, -0.000000000000000000 ) ) ;
#63462 = FACE_OUTER_BOUND ( 'NONE', #5845, .T. ) ;
#63463 = AXIS2_PLACEMENT_3D ( 'NONE', #118215, #59326, #99234 ) ;
#63465 = ORIENTED_EDGE ( 'NONE', *, *, #968, .F. ) ;
#63464 = AXIS2_PLACEMENT_3D ( 'NONE', #50461, #81226, #119853 ) ;
#63466 = ORIENTED_EDGE ( 'NONE', *, *, #59161, .T. ) ;
#63467 = DIRECTION ( 'NONE',  ( 0.000000000000000000, 0.000000000000000000, -1.000000000000000000 ) ) ;
#63468 = ORIENTED_EDGE ( 'NONE', *, *, #22518, .T. ) ;
#63469 = DIRECTION ( 'NONE',  ( 0.000000000000000000, -0.000000000000000000, 1.000000000000000000 ) ) ;
#63470 = CARTESIAN_POINT ( 'NONE',  ( 10.84999999999991260, 2.500000000000000000, 7.188010851410848723 ) ) ;
#63471 = ORIENTED_EDGE ( 'NONE', *, *, #42787, .T. ) ;
#63472 = CARTESIAN_POINT ( 'NONE',  ( 9.149999999999918643, 2.500000000000000000, 2.165063509461097713 ) ) ;
#63473 = CARTESIAN_POINT ( 'NONE',  ( -6.900000000000015454, 2.500000000000000000, 4.776537180435972196 ) ) ;
#63474 = DIRECTION ( 'NONE',  ( 0.000000000000000000, 0.000000000000000000, 1.000000000000000000 ) ) ;
#63475 = CARTESIAN_POINT ( 'NONE',  ( 187.5000000000000000, -1.500000000000000000, 6.000000000000000000 ) ) ;
#63476 = DIRECTION ( 'NONE',  ( -0.000000000000000000, -1.000000000000000000, -0.000000000000000000 ) ) ;
#63477 = AXIS2_PLACEMENT_3D ( 'NONE', #21718, #53113, #14449 ) ;
#63478 = ORIENTED_EDGE ( 'NONE', *, *, #24758, .F. ) ;
#63479 = EDGE_LOOP ( 'NONE', ( #39465, #43275, #59565, #22126 ) ) ;
#63480 = CARTESIAN_POINT ( 'NONE',  ( 10.39999999999990976, 2.500000000000000000, 4.330127018922196314 ) ) ;
#63481 = FACE_OUTER_BOUND ( 'NONE', #16649, .T. ) ;
#63482 = EDGE_CURVE ( 'NONE', #69018, #123444, #20577, .T. ) ;
#63484 = ORIENTED_EDGE ( 'NONE', *, *, #13034, .T. ) ;
#63483 = ORIENTED_EDGE ( 'NONE', *, *, #83843, .F. ) ;
#63485 = ORIENTED_EDGE ( 'NONE', *, *, #117149, .T. ) ;
#63486 = EDGE_CURVE ( 'NONE', #27243, #67262, #56061, .T. ) ;
#63487 = DIRECTION ( 'NONE',  ( 0.000000000000000000, -0.000000000000000000, 1.000000000000000000 ) ) ;
#63488 = AXIS2_PLACEMENT_3D ( 'NONE', #124083, #103807, #94615 ) ;
#63489 = EDGE_CURVE ( 'NONE', #6418, #68683, #81220, .T. ) ;
#63490 = CIRCLE ( 'NONE', #11236, 0.1000000000000002554 ) ;
#63491 = DIRECTION ( 'NONE',  ( 0.000000000000000000, 1.000000000000000000, 0.000000000000000000 ) ) ;
#63492 = DIRECTION ( 'NONE',  ( -0.000000000000000000, 1.000000000000000000, -0.000000000000000000 ) ) ;
#63493 = EDGE_CURVE ( 'NONE', #50907, #120378, #90698, .T. ) ;
#63494 = DIRECTION ( 'NONE',  ( 0.000000000000000000, 0.000000000000000000, 1.000000000000000000 ) ) ;
#63495 = CARTESIAN_POINT ( 'NONE',  ( -12.49999999999999289, 2.500000000000000000, 3.637306695894644726 ) ) ;
#63496 = FACE_OUTER_BOUND ( 'NONE', #25700, .T. ) ;
#63497 = CARTESIAN_POINT ( 'NONE',  ( 129.5000000000000000, 9.429780353434619030E-16, -7.700000000000000178 ) ) ;
#63498 = CARTESIAN_POINT ( 'NONE',  ( -1.450000000000035483, 2.500000000000000000, 1.818653347947321475 ) ) ;
#63499 = EDGE_CURVE ( 'NONE', #69394, #95323, #58243, .T. ) ;
#63500 = CIRCLE ( 'NONE', #2953, 0.1000000000000002554 ) ;
#63501 = AXIS2_PLACEMENT_3D ( 'NONE', #82190, #103112, #120182 ) ;
#63502 = DIRECTION ( 'NONE',  ( -0.000000000000000000, -1.000000000000000000, -0.000000000000000000 ) ) ;
#63503 = EDGE_CURVE ( 'NONE', #82453, #75790, #28991, .T. ) ;
#63504 = AXIS2_PLACEMENT_3D ( 'NONE', #4860, #92615, #43534 ) ;
#63506 = VERTEX_POINT ( 'NONE', #62542 ) ;
#63505 = EDGE_CURVE ( 'NONE', #119953, #81870, #77173, .T. ) ;
#63507 = CIRCLE ( 'NONE', #11250, 0.1000000000000002554 ) ;
#63508 = ADVANCED_FACE ( 'NONE', ( #103745 ), #118864, .T. ) ;
#63509 = DIRECTION ( 'NONE',  ( 0.000000000000000000, 0.000000000000000000, -1.000000000000000000 ) ) ;
#63510 = EDGE_LOOP ( 'NONE', ( #37537, #54489 ) ) ;
#63511 = VERTEX_POINT ( 'NONE', #74289 ) ;
#63512 = DIRECTION ( 'NONE',  ( 0.000000000000000000, 0.000000000000000000, 1.000000000000000000 ) ) ;
#63514 = AXIS2_PLACEMENT_3D ( 'NONE', #30487, #10184, #57999 ) ;
#63513 = CARTESIAN_POINT ( 'NONE',  ( 7.099999999999927702, 12.50000000000000000, 5.022947341949748790 ) ) ;
#63515 = DIRECTION ( 'NONE',  ( 0.000000000000000000, 1.000000000000000000, 0.000000000000000000 ) ) ;
#63516 = ADVANCED_FACE ( 'NONE', ( #22625 ), #123375, .T. ) ;
#63517 = DIRECTION ( 'NONE',  ( 0.000000000000000000, 1.000000000000000000, 0.000000000000000000 ) ) ;
#63518 = LINE ( 'NONE', #33423, #115465 ) ;
#63519 = VECTOR ( 'NONE', #117300, 1000.000000000000000 ) ;
#63520 = CARTESIAN_POINT ( 'NONE',  ( 185.9479166673494603, -6.668395609140176816, -3.850000000000003642 ) ) ;
#63521 = AXIS2_PLACEMENT_3D ( 'NONE', #67148, #67820, #6941 ) ;
#63522 = DIRECTION ( 'NONE',  ( 0.000000000000000000, 1.000000000000000000, 0.000000000000000000 ) ) ;
#63523 = VERTEX_POINT ( 'NONE', #12759 ) ;
#63524 = DIRECTION ( 'NONE',  ( -0.000000000000000000, 1.000000000000000000, -0.000000000000000000 ) ) ;
#63525 = AXIS2_PLACEMENT_3D ( 'NONE', #55849, #65667, #123307 ) ;
#63526 = CARTESIAN_POINT ( 'NONE',  ( 2.899999999999946620, 12.50000000000000000, 0.7579135962115869374 ) ) ;
#63527 = VERTEX_POINT ( 'NONE', #23235 ) ;
#63528 = ORIENTED_EDGE ( 'NONE', *, *, #41317, .F. ) ;
#63529 = EDGE_LOOP ( 'NONE', ( #29816, #15302, #118723, #20104 ) ) ;
#63530 = ADVANCED_FACE ( 'NONE', ( #102456 ), #100000, .T. ) ;
#63531 = ORIENTED_EDGE ( 'NONE', *, *, #65735, .T. ) ;
#63532 = CARTESIAN_POINT ( 'NONE',  ( -9.150000000000009237, 2.500000000000000000, 1.572243186433545548 ) ) ;
#63533 = CARTESIAN_POINT ( 'NONE',  ( -0.8500000000000390576, 2.500000000000000000, -6.395190528383301931 ) ) ;
#63534 = DIRECTION ( 'NONE',  ( 0.000000000000000000, -0.9999939076577903929, 0.003490651415223739937 ) ) ;
#63535 = DIRECTION ( 'NONE',  ( 0.000000000000000000, 1.000000000000000000, 0.000000000000000000 ) ) ;
#63536 = FACE_OUTER_BOUND ( 'NONE', #84190, .T. ) ;
#63537 = VERTEX_POINT ( 'NONE', #54624 ) ;
#63538 = DIRECTION ( 'NONE',  ( 0.000000000000000000, 1.000000000000000000, 0.000000000000000000 ) ) ;
#63539 = CARTESIAN_POINT ( 'NONE',  ( -11.25000000000000000, 2.500000000000000000, 7.088010851410848190 ) ) ;
#63540 = FACE_OUTER_BOUND ( 'NONE', #43471, .T. ) ;
#63541 = DIRECTION ( 'NONE',  ( 0.000000000000000000, 0.000000000000000000, -1.000000000000000000 ) ) ;
#63542 = EDGE_LOOP ( 'NONE', ( #65839, #63247 ) ) ;
#63543 = AXIS2_PLACEMENT_3D ( 'NONE', #95909, #6220, #56607 ) ;
#63544 = CIRCLE ( 'NONE', #23835, 0.06509327318403745899 ) ;
#63545 = EDGE_CURVE ( 'NONE', #110508, #47163, #43582, .T. ) ;
#63546 = AXIS2_PLACEMENT_3D ( 'NONE', #48092, #56594, #49395 ) ;
#63547 = ORIENTED_EDGE ( 'NONE', *, *, #122850, .T. ) ;
#63548 = AXIS2_PLACEMENT_3D ( 'NONE', #63157, #72354, #103085 ) ;
#63549 = ORIENTED_EDGE ( 'NONE', *, *, #93014, .T. ) ;
#63550 = CIRCLE ( 'NONE', #6785, 0.06509327318403745899 ) ;
#63551 = CARTESIAN_POINT ( 'NONE',  ( 0.6499999999999543920, 2.500000000000000000, 6.248780366869521430 ) ) ;
#63552 = PLANE ( 'NONE',  #71821 ) ;
#63553 = CARTESIAN_POINT ( 'NONE',  ( 8.149999999999920419, 2.500000000000000000, 6.941600689897073018 ) ) ;
#63554 = AXIS2_PLACEMENT_3D ( 'NONE', #68044, #7830, #47776 ) ;
#63555 = AXIS2_PLACEMENT_3D ( 'NONE', #44503, #45806, #15014 ) ;
#63556 = CONICAL_SURFACE ( 'NONE', #23846, 0.1000000000000002554, 0.003490658503988666988 ) ;
#63557 = CONICAL_SURFACE ( 'NONE', #84383, 0.09999999999999982514, 0.003490658503988666988 ) ;
#63558 = ORIENTED_EDGE ( 'NONE', *, *, #128478, .F. ) ;
#63559 = DIRECTION ( 'NONE',  ( -0.000000000000000000, 1.000000000000000000, -0.000000000000000000 ) ) ;
#63560 = CARTESIAN_POINT ( 'NONE',  ( -9.150000000000011013, 2.500000000000000000, -5.802370205355744659 ) ) ;
#63561 = EDGE_CURVE ( 'NONE', #94318, #116685, #93737, .T. ) ;
#63562 = CARTESIAN_POINT ( 'NONE',  ( -1.250000000000037526, 2.500000000000000000, -5.902370205355750521 ) ) ;
#63563 = CARTESIAN_POINT ( 'NONE',  ( -11.64999999999999680, 2.500000000000000000, 5.802370205355744659 ) ) ;
#63564 = CARTESIAN_POINT ( 'NONE',  ( -5.450000000000023270, 2.500000000000000000, -2.165063509461101710 ) ) ;
#63565 = VECTOR ( 'NONE', #10040, 1000.000000000000000 ) ;
#63566 = EDGE_LOOP ( 'NONE', ( #29372, #17742 ) ) ;
#63567 =( BOUNDED_CURVE ( )  B_SPLINE_CURVE ( 2, ( #82501, #73956, #32770, #13729, #112599, #72673, #22930 ),
 .UNSPECIFIED., .F., .F. ) 
 B_SPLINE_CURVE_WITH_KNOTS ( ( 3, 2, 2, 3 ),
 ( 0.6428571428571433488, 0.6666666666666670737, 0.6904761904761910207, 0.7142857142857148567 ),
 .UNSPECIFIED. ) 
 CURVE ( )  GEOMETRIC_REPRESENTATION_ITEM ( )  RATIONAL_B_SPLINE_CURVE ( ( 0.9999999999999974465, 0.8660254037844412611, 1.000000000000000000, 0.8660254037844387076, 1.000000000000000000, 0.8660254037844355990, 1.000000000000003109 ) ) 
 REPRESENTATION_ITEM ( '' )  );
#63568 = EDGE_LOOP ( 'NONE', ( #73836, #56122 ) ) ;
#63569 = DIRECTION ( 'NONE',  ( 0.000000000000000000, 0.000000000000000000, 1.000000000000000000 ) ) ;
#63570 = DIRECTION ( 'NONE',  ( 0.000000000000000000, 0.000000000000000000, 1.000000000000000000 ) ) ;
#63571 = CARTESIAN_POINT ( 'NONE',  ( 7.299999999999926104, 2.500000000000000000, -3.983716857408426293 ) ) ;
#63572 = CIRCLE ( 'NONE', #59389, 0.06509327318403745899 ) ;
#63573 = CARTESIAN_POINT ( 'NONE',  ( 145.7653593504141725, 2.500000000000000000, -3.576063159858998475 ) ) ;
#63574 = PLANE ( 'NONE',  #12254 ) ;
#63575 = VERTEX_POINT ( 'NONE', #4874 ) ;
#63576 = ORIENTED_EDGE ( 'NONE', *, *, #99081, .T. ) ;
#63577 = DIRECTION ( 'NONE',  ( -0.000000000000000000, -1.000000000000000000, -0.000000000000000000 ) ) ;
#63578 = CARTESIAN_POINT ( 'NONE',  ( -5.400000000000020783, 12.50000000000000000, 5.022947341949748790 ) ) ;
#63579 = CARTESIAN_POINT ( 'NONE',  ( -9.200000000000006395, 2.500000000000000000, -0.1000000000000023925 ) ) ;
#63580 = DIRECTION ( 'NONE',  ( 0.000000000000000000, 1.000000000000000000, 0.000000000000000000 ) ) ;
#63581 = ORIENTED_EDGE ( 'NONE', *, *, #87112, .T. ) ;
#63582 = CIRCLE ( 'NONE', #13393, 0.1000000000000002554 ) ;
#63583 = AXIS2_PLACEMENT_3D ( 'NONE', #12527, #63580, #23010 ) ;
#63584 = DIRECTION ( 'NONE',  ( 0.000000000000000000, 0.000000000000000000, -1.000000000000000000 ) ) ;
#63585 = ADVANCED_FACE ( 'NONE', ( #34375 ), #35257, .T. ) ;
#63586 = CARTESIAN_POINT ( 'NONE',  ( -1.900000000000035438, 2.500000000000000000, 3.883716857408420431 ) ) ;
#63587 = VERTEX_POINT ( 'NONE', #82827 ) ;
#63588 = CARTESIAN_POINT ( 'NONE',  ( -5.850000000000018296, 12.50000000000000000, 1.472243186433545459 ) ) ;
#63589 = ORIENTED_EDGE ( 'NONE', *, *, #7139, .T. ) ;
#63590 = EDGE_CURVE ( 'NONE', #46426, #85762, #97930, .T. ) ;
#63591 = DIRECTION ( 'NONE',  ( -0.000000000000000000, -1.000000000000000000, -0.000000000000000000 ) ) ;
#63592 = ORIENTED_EDGE ( 'NONE', *, *, #36383, .F. ) ;
#63593 = DIRECTION ( 'NONE',  ( 0.000000000000000000, 0.000000000000000000, 1.000000000000000000 ) ) ;
#63594 = FACE_OUTER_BOUND ( 'NONE', #45689, .T. ) ;
#63595 = EDGE_CURVE ( 'NONE', #73050, #14821, #83474, .T. ) ;
#63596 = EDGE_LOOP ( 'NONE', ( #98346, #78475 ) ) ;
#63597 = EDGE_CURVE ( 'NONE', #80507, #3939, #2298, .T. ) ;
#63598 = EDGE_LOOP ( 'NONE', ( #94255, #42559 ) ) ;
#63599 = ADVANCED_FACE ( 'NONE', ( #82170 ), #39573, .T. ) ;
#63600 = EDGE_CURVE ( 'NONE', #65132, #89806, #54001, .T. ) ;
#63601 = CARTESIAN_POINT ( 'NONE',  ( 185.0052083336747444, -6.551208109652278289, 3.782341765624995134 ) ) ;
#63602 = CARTESIAN_POINT ( 'NONE',  ( 10.64999999999990976, 2.500000000000000000, -6.841600689897077814 ) ) ;
#63603 = CARTESIAN_POINT ( 'NONE',  ( 186.6302083336747728, -4.367472073101514418, -7.564683531250002702 ) ) ;
#63604 = CARTESIAN_POINT ( 'NONE',  ( 186.0260416670080588, -6.551208109652273848, -3.782341765625003571 ) ) ;
#63605 = CARTESIAN_POINT ( 'NONE',  ( -2.700000000000029932, 12.50000000000000000, -0.3464101615137782364 ) ) ;
#63606 = CARTESIAN_POINT ( 'NONE',  ( 1.649999999999951061, 2.500000000000000000, -6.395190528383301931 ) ) ;
#63607 = CARTESIAN_POINT ( 'NONE',  ( 142.3152275665817115, 0.5000000000000000000, 2.763522878056728693 ) ) ;
#63608 = CIRCLE ( 'NONE', #30264, 0.09999999999999982514 ) ;
#63609 = DIRECTION ( 'NONE',  ( 0.000000000000000000, 1.000000000000000000, 0.000000000000000000 ) ) ;
#63610 = ADVANCED_FACE ( 'NONE', ( #65081 ), #103093, .T. ) ;
#63611 = CIRCLE ( 'NONE', #21754, 0.06509327318403745899 ) ;
#63612 = EDGE_CURVE ( 'NONE', #47637, #107914, #3932, .T. ) ;
#63613 = ADVANCED_FACE ( 'NONE', ( #42250 ), #75045, .T. ) ;
#63614 = ORIENTED_EDGE ( 'NONE', *, *, #92577, .F. ) ;
#63615 = EDGE_LOOP ( 'NONE', ( #113085, #32794, #82546, #53292 ) ) ;
#63616 = DIRECTION ( 'NONE',  ( -0.000000000000000000, -1.000000000000000000, -0.000000000000000000 ) ) ;
#63617 = VERTEX_POINT ( 'NONE', #4231 ) ;
#63618 = FACE_OUTER_BOUND ( 'NONE', #28430, .T. ) ;
#63619 = CARTESIAN_POINT ( 'NONE',  ( -9.600000000000006750, 2.500000000000000000, 3.537306695894645081 ) ) ;
#63620 = DIRECTION ( 'NONE',  ( 0.000000000000000000, 0.000000000000000000, 1.000000000000000000 ) ) ;
#63622 = ORIENTED_EDGE ( 'NONE', *, *, #127421, .F. ) ;
#63621 = ORIENTED_EDGE ( 'NONE', *, *, #92037, .T. ) ;
#63623 = CARTESIAN_POINT ( 'NONE',  ( 0.7999999999999548583, 12.50000000000000000, 4.395220292106234439 ) ) ;
#63624 = VERTEX_POINT ( 'NONE', #104384 ) ;
#63625 = DIRECTION ( 'NONE',  ( 0.000000000000000000, 0.000000000000000000, 1.000000000000000000 ) ) ;
#63626 = CARTESIAN_POINT ( 'NONE',  ( -12.49999999999995737, 12.50000000000000000, 4.395220292106234439 ) ) ;
#63627 = DIRECTION ( 'NONE',  ( -0.000000000000000000, 1.000000000000000000, -0.000000000000000000 ) ) ;
#63628 = DIRECTION ( 'NONE',  ( 0.000000000000000000, 0.000000000000000000, 1.000000000000000000 ) ) ;
#63629 = DIRECTION ( 'NONE',  ( -4.274815082592931898E-19, -0.9999939076577903929, -0.003490651415223739937 ) ) ;
#63631 = DIRECTION ( 'NONE',  ( 0.000000000000000000, 0.000000000000000000, 1.000000000000000000 ) ) ;
#63630 = AXIS2_PLACEMENT_3D ( 'NONE', #80582, #41312, #41952 ) ;
#63632 = CIRCLE ( 'NONE', #2987, 0.09999999999999982514 ) ;
#63633 = DIRECTION ( 'NONE',  ( 0.000000000000000000, 0.000000000000000000, -1.000000000000000000 ) ) ;
#63634 = DIRECTION ( 'NONE',  ( -4.274815082592931898E-19, -0.9999939076577903929, -0.003490651415223739937 ) ) ;
#63635 = AXIS2_PLACEMENT_3D ( 'NONE', #3103, #41106, #102568 ) ;
#63636 = CARTESIAN_POINT ( 'NONE',  ( 186.2760416670080588, 6.551208109652274736, 3.782341765625001351 ) ) ;
#63637 = CARTESIAN_POINT ( 'NONE',  ( -3.750000000000027534, 2.500000000000000000, 2.857883832488649301 ) ) ;
#63638 = CARTESIAN_POINT ( 'NONE',  ( -3.749999999999991118, 2.500000000000000000, -2.265063509461101798 ) ) ;
#63639 = VECTOR ( 'NONE', #32690, 1000.000000000000000 ) ;
#63641 = EDGE_LOOP ( 'NONE', ( #52669, #50260 ) ) ;
#63640 = VECTOR ( 'NONE', #119038, 1000.000000000000000 ) ;
#63642 = VERTEX_POINT ( 'NONE', #14688 ) ;
#63643 = VERTEX_POINT ( 'NONE', #94551 ) ;
#63645 = CARTESIAN_POINT ( 'NONE',  ( 108.0000000000000142, 9.000000000000001776, 0.000000000000000000 ) ) ;
#63644 = AXIS2_PLACEMENT_3D ( 'NONE', #40873, #110855, #31670 ) ;
#63646 = ORIENTED_EDGE ( 'NONE', *, *, #124067, .T. ) ;
#63647 = LINE ( 'NONE', #26131, #61225 ) ;
#63649 = VERTEX_POINT ( 'NONE', #86670 ) ;
#63648 = VERTEX_POINT ( 'NONE', #97787 ) ;
#63650 = ORIENTED_EDGE ( 'NONE', *, *, #48656, .T. ) ;
#63651 = CARTESIAN_POINT ( 'NONE',  ( 10.64999999999991331, 12.50000000000000000, -1.818653347947325916 ) ) ;
#63652 = AXIS2_PLACEMENT_3D ( 'NONE', #38581, #9090, #106646 ) ;
#63653 = AXIS2_PLACEMENT_3D ( 'NONE', #94187, #74548, #124300 ) ;
#63654 = CARTESIAN_POINT ( 'NONE',  ( -8.550000000000014921, 12.50000000000000000, -6.148780366869520897 ) ) ;
#63655 =( NAMED_UNIT ( * ) SI_UNIT ( $, .STERADIAN. ) SOLID_ANGLE_UNIT ( ) );
#63656 = DIRECTION ( 'NONE',  ( 0.000000000000000000, 0.000000000000000000, 1.000000000000000000 ) ) ;
#63657 = DIRECTION ( 'NONE',  ( 0.000000000000000000, 0.000000000000000000, 1.000000000000000000 ) ) ;
#63658 = CONICAL_SURFACE ( 'NONE', #105409, 0.1000000000000002554, 0.003490658503988666988 ) ;
#63659 = FACE_OUTER_BOUND ( 'NONE', #119127, .T. ) ;
#63660 = ORIENTED_EDGE ( 'NONE', *, *, #36315, .T. ) ;
#63661 = ADVANCED_FACE ( 'NONE', ( #127261 ), #106316, .T. ) ;
#63662 = CARTESIAN_POINT ( 'NONE',  ( -3.300000000000028244, 12.50000000000000000, 4.395220292106234439 ) ) ;
#63663 = ORIENTED_EDGE ( 'NONE', *, *, #47233, .F. ) ;
#63664 = ADVANCED_FACE ( 'NONE', ( #55921 ), #41616, .T. ) ;
#63665 = EDGE_LOOP ( 'NONE', ( #83762, #103866, #103219, #70425 ) ) ;
#63666 = ORIENTED_EDGE ( 'NONE', *, *, #56749, .F. ) ;
#63667 = ADVANCED_FACE ( 'NONE', ( #35649 ), #15982, .T. ) ;
#63668 = DIRECTION ( 'NONE',  ( 0.000000000000000000, 0.000000000000000000, -1.000000000000000000 ) ) ;
#63669 = EDGE_LOOP ( 'NONE', ( #110012, #81514, #123190, #128090 ) ) ;
#63670 = VERTEX_POINT ( 'NONE', #77496 ) ;
#63671 = ORIENTED_EDGE ( 'NONE', *, *, #12360, .F. ) ;
#63672 = CIRCLE ( 'NONE', #82544, 0.06509327318403745899 ) ;
#63673 = DIRECTION ( 'NONE',  ( 0.000000000000000000, 0.000000000000000000, 1.000000000000000000 ) ) ;
#63674 = EDGE_CURVE ( 'NONE', #5720, #29188, #5518, .T. ) ;
#63675 = LINE ( 'NONE', #64932, #129205 ) ;
#63676 = DIRECTION ( 'NONE',  ( -0.000000000000000000, 1.000000000000000000, -0.000000000000000000 ) ) ;
#63677 = FACE_OUTER_BOUND ( 'NONE', #13571, .T. ) ;
#63678 = DIRECTION ( 'NONE',  ( -0.000000000000000000, 1.000000000000000000, -0.000000000000000000 ) ) ;
#63679 = FACE_OUTER_BOUND ( 'NONE', #13403, .T. ) ;
#63680 = DIRECTION ( 'NONE',  ( -0.000000000000000000, 1.000000000000000000, -0.000000000000000000 ) ) ;
#63681 = AXIS2_PLACEMENT_3D ( 'NONE', #117502, #27871, #40278 ) ;
#63682 = CIRCLE ( 'NONE', #49023, 0.09999999999999982514 ) ;
#63683 = ORIENTED_EDGE ( 'NONE', *, *, #48625, .F. ) ;
#63684 = DIRECTION ( 'NONE',  ( 0.000000000000000000, 1.000000000000000000, 0.000000000000000000 ) ) ;
#63685 = ORIENTED_EDGE ( 'NONE', *, *, #98476, .T. ) ;
#63686 = LINE ( 'NONE', #85247, #31506 ) ;
#63687 = ORIENTED_EDGE ( 'NONE', *, *, #16605, .T. ) ;
#63688 = EDGE_CURVE ( 'NONE', #48618, #16035, #72898, .T. ) ;
#63689 = ORIENTED_EDGE ( 'NONE', *, *, #68310, .F. ) ;
#63690 = LINE ( 'NONE', #74148, #59488 ) ;
#63691 = CARTESIAN_POINT ( 'NONE',  ( 184.1927083336747160, 6.551208109652275624, -3.782341765624998686 ) ) ;
#63692 = CONICAL_SURFACE ( 'NONE', #65811, 0.1000000000000002554, 0.003490658503988666988 ) ;
#63693 = DIRECTION ( 'NONE',  ( -0.000000000000000000, -1.000000000000000000, -0.000000000000000000 ) ) ;
#63694 = AXIS2_PLACEMENT_3D ( 'NONE', #125091, #24957, #74059 ) ;
#63695 = VERTEX_POINT ( 'NONE', #125312 ) ;
#63696 = VERTEX_POINT ( 'NONE', #16626 ) ;
#63697 = CARTESIAN_POINT ( 'NONE',  ( -4.150000000000025224, 2.500000000000000000, 2.957883832488649389 ) ) ;
#63698 = DIRECTION ( 'NONE',  ( -0.000000000000000000, 1.000000000000000000, -0.000000000000000000 ) ) ;
#63699 = DIRECTION ( 'NONE',  ( 0.000000000000000000, 0.000000000000000000, -1.000000000000000000 ) ) ;
#63700 = LINE ( 'NONE', #5405, #105671 ) ;
#63701 = DIRECTION ( 'NONE',  ( -0.000000000000000000, -1.000000000000000000, -0.000000000000000000 ) ) ;
#63702 = ORIENTED_EDGE ( 'NONE', *, *, #44074, .T. ) ;
#63703 = CONICAL_SURFACE ( 'NONE', #42977, 0.09999999999999982514, 0.003490658503988666988 ) ;
#63704 = AXIS2_PLACEMENT_3D ( 'NONE', #107719, #129321, #127367 ) ;
#63705 = ADVANCED_FACE ( 'NONE', ( #67015 ), #64568, .T. ) ;
#63706 = EDGE_LOOP ( 'NONE', ( #49988, #44882, #90705, #70191 ) ) ;
#63707 = CIRCLE ( 'NONE', #7237, 0.06509327318403745899 ) ;
#63708 = FACE_OUTER_BOUND ( 'NONE', #98281, .T. ) ;
#63709 = CARTESIAN_POINT ( 'NONE',  ( 8.349999999999919709, 12.50000000000000000, 5.802370205355744659 ) ) ;
#63710 = CARTESIAN_POINT ( 'NONE',  ( 184.8802083336747444, 4.367472073101515306, 7.564683531250000925 ) ) ;
#63711 = DIRECTION ( 'NONE',  ( -0.000000000000000000, 1.000000000000000000, -0.000000000000000000 ) ) ;
#63712 = DIRECTION ( 'NONE',  ( 0.000000000000000000, 1.000000000000000000, 0.000000000000000000 ) ) ;
#63713 = EDGE_CURVE ( 'NONE', #105557, #55712, #87942, .T. ) ;
#63714 = DIRECTION ( 'NONE',  ( -4.274815082592931898E-19, -0.9999939076577903929, -0.003490651415223739937 ) ) ;
#63715 = DIRECTION ( 'NONE',  ( 0.000000000000000000, 1.000000000000000000, 0.000000000000000000 ) ) ;
#63716 = ORIENTED_EDGE ( 'NONE', *, *, #39384, .F. ) ;
#63717 = DIRECTION ( 'NONE',  ( 0.000000000000000000, -0.000000000000000000, 1.000000000000000000 ) ) ;
#63719 = CARTESIAN_POINT ( 'NONE',  ( 13.54999999999989591, 2.500000000000000000, -1.818653347947326138 ) ) ;
#63718 = AXIS2_PLACEMENT_3D ( 'NONE', #128248, #45813, #38586 ) ;
#63720 = CARTESIAN_POINT ( 'NONE',  ( 9.199999999999919353, 2.500000000000000000, -0.1000000000000022815 ) ) ;
#63721 = VECTOR ( 'NONE', #61927, 1000.000000000000000 ) ;
#63722 = EDGE_LOOP ( 'NONE', ( #48982, #64708, #58781, #55863 ) ) ;
#63723 = CIRCLE ( 'NONE', #57462, 0.06509327318403745899 ) ;
#63724 = VECTOR ( 'NONE', #16750, 1000.000000000000000 ) ;
#63725 = EDGE_CURVE ( 'NONE', #29090, #74701, #115461, .T. ) ;
#63726 = DIRECTION ( 'NONE',  ( 0.000000000000000000, 1.000000000000000000, 0.000000000000000000 ) ) ;
#63727 = CIRCLE ( 'NONE', #24015, 0.1000000000000002554 ) ;
#63728 = AXIS2_PLACEMENT_3D ( 'NONE', #6434, #88223, #128190 ) ;
#63729 = ORIENTED_EDGE ( 'NONE', *, *, #113743, .F. ) ;
#63730 = LINE ( 'NONE', #122645, #27938 ) ;
#63731 = AXIS2_PLACEMENT_3D ( 'NONE', #30565, #29264, #71105 ) ;
#63732 = EDGE_LOOP ( 'NONE', ( #92197, #84860 ) ) ;
#63733 = FACE_OUTER_BOUND ( 'NONE', #122580, .T. ) ;
#63734 = DIRECTION ( 'NONE',  ( 0.000000000000000000, 0.000000000000000000, 1.000000000000000000 ) ) ;
#63735 = DIRECTION ( 'NONE',  ( 0.000000000000000000, 0.000000000000000000, 1.000000000000000000 ) ) ;
#63736 = EDGE_LOOP ( 'NONE', ( #9969, #22915, #16956, #4223 ) ) ;
#63737 = AXIS2_PLACEMENT_3D ( 'NONE', #57400, #97958, #58688 ) ;
#63738 = CIRCLE ( 'NONE', #118101, 0.1000000000000000472 ) ;
#63739 = CARTESIAN_POINT ( 'NONE',  ( -11.24999999999996270, 2.500000000000000000, 6.595190528383296780 ) ) ;
#63740 = EDGE_CURVE ( 'NONE', #104745, #32777, #45807, .T. ) ;
#63741 = CARTESIAN_POINT ( 'NONE',  ( -3.350000000000028955, 12.50000000000000000, 5.737276932171707422 ) ) ;
#63742 = ORIENTED_EDGE ( 'NONE', *, *, #41288, .T. ) ;
#63743 = EDGE_CURVE ( 'NONE', #114031, #10654, #36942, .T. ) ;
#63744 = ORIENTED_EDGE ( 'NONE', *, *, #65790, .F. ) ;
#63745 = ORIENTED_EDGE ( 'NONE', *, *, #13690, .T. ) ;
#63746 = DIRECTION ( 'NONE',  ( 0.000000000000000000, 1.000000000000000000, 0.000000000000000000 ) ) ;
#63747 = DIRECTION ( 'NONE',  ( 0.000000000000000000, 1.000000000000000000, 0.000000000000000000 ) ) ;
#63748 = DIRECTION ( 'NONE',  ( 0.000000000000000000, 0.000000000000000000, 1.000000000000000000 ) ) ;
#63749 = EDGE_CURVE ( 'NONE', #86969, #46288, #35342, .T. ) ;
#63750 = EDGE_CURVE ( 'NONE', #29271, #108499, #22833, .T. ) ;
#63751 = VERTEX_POINT ( 'NONE', #86007 ) ;
#63752 = EDGE_CURVE ( 'NONE', #26581, #105656, #118063, .T. ) ;
#63753 = EDGE_CURVE ( 'NONE', #12555, #71950, #121011, .T. ) ;
#63754 = DIRECTION ( 'NONE',  ( 0.000000000000000000, 1.000000000000000000, 0.000000000000000000 ) ) ;
#63755 = CARTESIAN_POINT ( 'NONE',  ( 0.4499999999999569344, 12.50000000000000000, 2.165063509461097713 ) ) ;
#63756 = AXIS2_PLACEMENT_3D ( 'NONE', #128517, #60411, #29008 ) ;
#63757 = ORIENTED_EDGE ( 'NONE', *, *, #55823, .F. ) ;
#63758 = DIRECTION ( 'NONE',  ( 0.000000000000000000, 0.000000000000000000, 1.000000000000000000 ) ) ;
#63759 = DIRECTION ( 'NONE',  ( 0.000000000000000000, 0.000000000000000000, 1.000000000000000000 ) ) ;
#63760 = ADVANCED_FACE ( 'NONE', ( #28411 ), #112701, .T. ) ;
#63761 = CARTESIAN_POINT ( 'NONE',  ( 107.5000000000000142, 0.000000000000000000, -2.000000000000000000 ) ) ;
#63762 = PLANE ( 'NONE',  #126552 ) ;
#63763 = DIRECTION ( 'NONE',  ( 1.000000000000000000, 0.000000000000000000, 0.000000000000000000 ) ) ;
#63764 = EDGE_CURVE ( 'NONE', #59178, #79801, #93825, .T. ) ;
#63765 = CARTESIAN_POINT ( 'NONE',  ( -9.800000000000004263, 12.50000000000000000, -0.3464101615137783474 ) ) ;
#63766 = CARTESIAN_POINT ( 'NONE',  ( 6.449999999999931788, 2.500000000000000000, -6.148780366869526226 ) ) ;
#63767 = CONICAL_SURFACE ( 'NONE', #7309, 0.09999999999999982514, 0.003490658503988666988 ) ;
#63768 = CIRCLE ( 'NONE', #80503, 0.06509327318403745899 ) ;
#63769 = ADVANCED_FACE ( 'NONE', ( #95217 ), #79262, .T. ) ;
#63770 = EDGE_CURVE ( 'NONE', #90867, #35444, #33205, .T. ) ;
#63771 = ORIENTED_EDGE ( 'NONE', *, *, #59204, .T. ) ;
#63772 = ORIENTED_EDGE ( 'NONE', *, *, #98139, .T. ) ;
#63773 = ORIENTED_EDGE ( 'NONE', *, *, #87513, .F. ) ;
#63774 = ORIENTED_EDGE ( 'NONE', *, *, #3194, .T. ) ;
#63775 = DIRECTION ( 'NONE',  ( -0.000000000000000000, -1.000000000000000000, -0.000000000000000000 ) ) ;
#63776 = DIRECTION ( 'NONE',  ( 0.000000000000000000, 1.000000000000000000, 0.000000000000000000 ) ) ;
#63777 = DIRECTION ( 'NONE',  ( 0.000000000000000000, 0.000000000000000000, -1.000000000000000000 ) ) ;
#63778 = EDGE_LOOP ( 'NONE', ( #63316, #15753, #75519, #89314 ) ) ;
#63779 = FACE_BOUND ( 'NONE', #8542, .T. ) ;
#63780 = ADVANCED_FACE ( 'NONE', ( #29066 ), #112613, .T. ) ;
#63781 = CARTESIAN_POINT ( 'NONE',  ( 3.349999999999944578, 2.500000000000000000, -1.472243186433550122 ) ) ;
#63782 = DIRECTION ( 'NONE',  ( 0.000000000000000000, 0.000000000000000000, 1.000000000000000000 ) ) ;
#63783 = AXIS2_PLACEMENT_3D ( 'NONE', #43936, #4605, #32832 ) ;
#63784 = DIRECTION ( 'NONE',  ( 0.000000000000000000, 1.000000000000000000, 0.000000000000000000 ) ) ;
#63785 = DIRECTION ( 'NONE',  ( 0.000000000000000000, 0.000000000000000000, 1.000000000000000000 ) ) ;
#63786 = AXIS2_PLACEMENT_3D ( 'NONE', #81777, #11101, #111229 ) ;
#63787 = CARTESIAN_POINT ( 'NONE',  ( -14.99999999999998224, 12.50000000000000000, -0.6277270498435144619 ) ) ;
#63788 = DIRECTION ( 'NONE',  ( 0.000000000000000000, 0.000000000000000000, 1.000000000000000000 ) ) ;
#63789 = DIRECTION ( 'NONE',  ( -0.000000000000000000, 1.000000000000000000, -0.000000000000000000 ) ) ;
#63790 = PLANE ( 'NONE',  #67951 ) ;
#63791 = DIRECTION ( 'NONE',  ( 0.000000000000000000, 1.000000000000000000, 0.000000000000000000 ) ) ;
#63792 = CARTESIAN_POINT ( 'NONE',  ( 3.749999999999942268, 12.50000000000000000, -1.472243186433550122 ) ) ;
#63793 = VERTEX_POINT ( 'NONE', #51291 ) ;
#63794 = VECTOR ( 'NONE', #15427, 1000.000000000000000 ) ;
#63795 = ORIENTED_EDGE ( 'NONE', *, *, #59740, .F. ) ;
#63796 = EDGE_LOOP ( 'NONE', ( #116608, #61822, #22958, #89430 ) ) ;
#63797 = VECTOR ( 'NONE', #84699, 1000.000000000000000 ) ;
#63798 = VERTEX_POINT ( 'NONE', #70913 ) ;
#63799 = ORIENTED_EDGE ( 'NONE', *, *, #90027, .F. ) ;
#63800 = ORIENTED_EDGE ( 'NONE', *, *, #101920, .F. ) ;
#63801 = FACE_OUTER_BOUND ( 'NONE', #114070, .T. ) ;
#63802 = ORIENTED_EDGE ( 'NONE', *, *, #32597, .F. ) ;
#63803 = ORIENTED_EDGE ( 'NONE', *, *, #27193, .F. ) ;
#63804 = CARTESIAN_POINT ( 'NONE',  ( 14.37945523737784725, -2.500000000000446310, 7.667852709071338424 ) ) ;
#63805 = DIRECTION ( 'NONE',  ( 0.000000000000000000, 0.000000000000000000, 1.000000000000000000 ) ) ;
#63806 = DIRECTION ( 'NONE',  ( -0.000000000000000000, 1.000000000000000000, -0.000000000000000000 ) ) ;
#63807 = EDGE_LOOP ( 'NONE', ( #42413, #102764, #117228, #5256 ) ) ;
#63808 = CARTESIAN_POINT ( 'NONE',  ( 6.649999999999930189, 2.500000000000000000, 5.902370205355745192 ) ) ;
#63809 = ORIENTED_EDGE ( 'NONE', *, *, #72932, .F. ) ;
#63810 = EDGE_CURVE ( 'NONE', #49718, #128241, #108485, .T. ) ;
#63812 = ORIENTED_EDGE ( 'NONE', *, *, #27743, .F. ) ;
#63811 = AXIS2_PLACEMENT_3D ( 'NONE', #19321, #100474, #99847 ) ;
#63814 = ORIENTED_EDGE ( 'NONE', *, *, #59792, .T. ) ;
#63813 = CARTESIAN_POINT ( 'NONE',  ( 1.049999999999952083, 2.500000000000000000, 6.741600689897071952 ) ) ;
#63815 = CIRCLE ( 'NONE', #22053, 2.000000000000000000 ) ;
#63816 = ADVANCED_FACE ( 'NONE', ( #71542 ), #21153, .T. ) ;
#63817 = VECTOR ( 'NONE', #117871, 1000.000000000000000 ) ;
#63818 = CARTESIAN_POINT ( 'NONE',  ( 184.5000000000000000, 0.000000000000000000, 7.700000000000000178 ) ) ;
#63819 = ORIENTED_EDGE ( 'NONE', *, *, #84207, .T. ) ;
#63820 = UNCERTAINTY_MEASURE_WITH_UNIT (LENGTH_MEASURE( 1.000000000000000082E-05 ), #82675, 'distance_accuracy_value', 'NONE');
#63821 = DIRECTION ( 'NONE',  ( 0.000000000000000000, 0.000000000000000000, 1.000000000000000000 ) ) ;
#63822 = CONICAL_SURFACE ( 'NONE', #111939, 0.09999999999999999167, 0.003490658503988666988 ) ;
#63823 = CARTESIAN_POINT ( 'NONE',  ( -10.40000000000000213, 12.50000000000000000, -4.957854068765712441 ) ) ;
#63824 = DIRECTION ( 'NONE',  ( -4.274815082592931898E-19, -0.9999939076577903929, -0.003490651415223739937 ) ) ;
#63825 = DIRECTION ( 'NONE',  ( -0.000000000000000000, -1.000000000000000000, -0.000000000000000000 ) ) ;
#63826 = CIRCLE ( 'NONE', #53363, 0.06509327318403745899 ) ;
#63827 = DIRECTION ( 'NONE',  ( 0.000000000000000000, 1.000000000000000000, 0.000000000000000000 ) ) ;
#63828 = ORIENTED_EDGE ( 'NONE', *, *, #10364, .F. ) ;
#63829 = CARTESIAN_POINT ( 'NONE',  ( 7.899999999999924860, 12.50000000000000000, 3.572213422710607489 ) ) ;
#63830 = AXIS2_PLACEMENT_3D ( 'NONE', #84773, #54026, #125342 ) ;
#63831 = CIRCLE ( 'NONE', #74296, 0.06509327318403745899 ) ;
#63832 = VERTEX_POINT ( 'NONE', #88612 ) ;
#63833 = CARTESIAN_POINT ( 'NONE',  ( 17.50000000000000000, 2.499999999999999556, -0.6666666666666630769 ) ) ;
#63834 = ORIENTED_EDGE ( 'NONE', *, *, #52357, .F. ) ;
#63835 = DIRECTION ( 'NONE',  ( -0.000000000000000000, -1.000000000000000000, -0.000000000000000000 ) ) ;
#63836 = DIRECTION ( 'NONE',  ( 0.000000000000000000, 0.000000000000000000, 1.000000000000000000 ) ) ;
#63837 = VECTOR ( 'NONE', #111668, 1000.000000000000000 ) ;
#63838 = LINE ( 'NONE', #42933, #17322 ) ;
#63839 = DIRECTION ( 'NONE',  ( 0.000000000000000000, -0.000000000000000000, 1.000000000000000000 ) ) ;
#63840 = ORIENTED_EDGE ( 'NONE', *, *, #123193, .T. ) ;
#63841 = CARTESIAN_POINT ( 'NONE',  ( 4.549999999999939426, 12.50000000000000000, -2.165063509461101710 ) ) ;
#63842 = DIRECTION ( 'NONE',  ( 0.000000000000000000, 1.000000000000000000, 0.000000000000000000 ) ) ;
#63843 = ORIENTED_EDGE ( 'NONE', *, *, #113836, .T. ) ;
#63844 = EDGE_LOOP ( 'NONE', ( #118292, #117456 ) ) ;
#63845 = EDGE_LOOP ( 'NONE', ( #108497, #82698 ) ) ;
#63846 = CARTESIAN_POINT ( 'NONE',  ( 0.1999999999999636513, 2.500000000000000000, -0.3464101615137760715 ) ) ;
#63847 = CARTESIAN_POINT ( 'NONE',  ( -8.750000000000012434, 2.500000000000000000, -5.702370205355745014 ) ) ;
#63848 = CARTESIAN_POINT ( 'NONE',  ( 184.7760416670080588, 6.551208109652274736, 3.782341765625001351 ) ) ;
#63849 = AXIS2_PLACEMENT_3D ( 'NONE', #121882, #94346, #113345 ) ;
#63850 = CARTESIAN_POINT ( 'NONE',  ( 184.2812500006828031, 0.000000000000000000, 7.700000000000000178 ) ) ;
#63851 = EDGE_CURVE ( 'NONE', #10073, #115594, #123075, .T. ) ;
#63852 = CARTESIAN_POINT ( 'NONE',  ( 179.5000000000000000, 1.375000000000002665, -7.634788798650556707 ) ) ;
#63853 = CARTESIAN_POINT ( 'NONE',  ( -3.750000000000027534, 2.500000000000000000, 2.857883832488649301 ) ) ;
#63854 = AXIS2_PLACEMENT_3D ( 'NONE', #91788, #22425, #10620 ) ;
#63855 = CIRCLE ( 'NONE', #97302, 0.06509327318403745899 ) ;
#63856 = ORIENTED_EDGE ( 'NONE', *, *, #72630, .T. ) ;
#63857 = DIRECTION ( 'NONE',  ( 0.000000000000000000, 0.000000000000000000, 1.000000000000000000 ) ) ;
#63858 = ORIENTED_EDGE ( 'NONE', *, *, #16981, .F. ) ;
#63859 = CARTESIAN_POINT ( 'NONE',  ( 11.44999999999990870, 12.50000000000000000, -1.753560074763288679 ) ) ;
#63860 = EDGE_CURVE ( 'NONE', #94655, #17558, #43669, .T. ) ;
#63862 = EDGE_CURVE ( 'NONE', #62517, #108936, #30359, .T. ) ;
#63861 = DIRECTION ( 'NONE',  ( -4.274815082592931898E-19, -0.9999939076577903929, -0.003490651415223739937 ) ) ;
#63863 = DIRECTION ( 'NONE',  ( 0.000000000000000000, 0.000000000000000000, -1.000000000000000000 ) ) ;
#63864 = DIRECTION ( 'NONE',  ( 0.000000000000000000, 1.000000000000000000, 0.000000000000000000 ) ) ;
#63865 = EDGE_LOOP ( 'NONE', ( #44520, #34364, #102899, #73533 ) ) ;
#63866 = VECTOR ( 'NONE', #128954, 1000.000000000000000 ) ;
#63867 = CONICAL_SURFACE ( 'NONE', #26213, 0.09999999999999999167, 0.003490658503988666988 ) ;
#63868 = LINE ( 'NONE', #42299, #40864 ) ;
#63870 = ORIENTED_EDGE ( 'NONE', *, *, #98746, .T. ) ;
#63869 = DIRECTION ( 'NONE',  ( -0.000000000000000000, 1.000000000000000000, -0.000000000000000000 ) ) ;
#63871 = EDGE_CURVE ( 'NONE', #89315, #74379, #12337, .T. ) ;
#63872 = ORIENTED_EDGE ( 'NONE', *, *, #862, .T. ) ;
#63873 = CARTESIAN_POINT ( 'NONE',  ( 0.8499999999999553468, 12.50000000000000000, 1.472243186433545459 ) ) ;
#63874 = CONICAL_SURFACE ( 'NONE', #38870, 0.09999999999999982514, 0.003490658503988666988 ) ;
#63875 = AXIS2_PLACEMENT_3D ( 'NONE', #107569, #97738, #127846 ) ;
#63876 = ORIENTED_EDGE ( 'NONE', *, *, #12761, .T. ) ;
#63877 = ORIENTED_EDGE ( 'NONE', *, *, #107820, .T. ) ;
#63878 = CARTESIAN_POINT ( 'NONE',  ( -7.700000000000014388, 12.50000000000000000, -0.3464101615137782364 ) ) ;
#63879 = ORIENTED_EDGE ( 'NONE', *, *, #50741, .F. ) ;
#63880 = FACE_OUTER_BOUND ( 'NONE', #11202, .T. ) ;
#63881 = CARTESIAN_POINT ( 'NONE',  ( 10.84999999999991260, 2.500000000000000000, -1.572243186433550211 ) ) ;
#63882 = LINE ( 'NONE', #31852, #50054 ) ;
#63883 = VERTEX_POINT ( 'NONE', #10668 ) ;
#63884 = CONICAL_SURFACE ( 'NONE', #80623, 0.1000000000000002554, 0.003490658503988666988 ) ;
#63885 = CARTESIAN_POINT ( 'NONE',  ( -5.000000000000023093, 2.500000000000000000, 0.5928203230275495006 ) ) ;
#63887 = ORIENTED_EDGE ( 'NONE', *, *, #84332, .F. ) ;
#63886 = DIRECTION ( 'NONE',  ( 0.000000000000000000, 0.000000000000000000, -1.000000000000000000 ) ) ;
#63888 = CARTESIAN_POINT ( 'NONE',  ( 15.39999999999989200, 2.500000000000000000, 0.5928203230275495006 ) ) ;
#63889 = DIRECTION ( 'NONE',  ( -0.000000000000000000, -1.000000000000000000, -0.000000000000000000 ) ) ;
#63890 = CONICAL_SURFACE ( 'NONE', #7444, 0.1000000000000000472, 0.003490658503988666988 ) ;
#63891 = ORIENTED_EDGE ( 'NONE', *, *, #47225, .F. ) ;
#63892 = EDGE_CURVE ( 'NONE', #76783, #100499, #87552, .T. ) ;
#63893 = VECTOR ( 'NONE', #55879, 1000.000000000000000 ) ;
#63894 = EDGE_LOOP ( 'NONE', ( #60135, #113121 ) ) ;
#63895 = AXIS2_PLACEMENT_3D ( 'NONE', #45996, #75430, #115338 ) ;
#63896 = EDGE_LOOP ( 'NONE', ( #27377, #121930 ) ) ;
#63897 = VERTEX_POINT ( 'NONE', #58527 ) ;
#63898 = DIRECTION ( 'NONE',  ( 0.000000000000000000, 0.000000000000000000, 1.000000000000000000 ) ) ;
#63899 = CARTESIAN_POINT ( 'NONE',  ( 1.849999999999949019, 2.500000000000000000, 6.941600689897073018 ) ) ;
#63900 = CARTESIAN_POINT ( 'NONE',  ( 4.149999999999939959, 2.500000000000000000, 1.472243186433545459 ) ) ;
#63901 = ADVANCED_FACE ( 'NONE', ( #121295 ), #66712, .T. ) ;
#63902 = FACE_BOUND ( 'NONE', #7514, .T. ) ;
#63903 = VERTEX_POINT ( 'NONE', #20527 ) ;
#63904 = CARTESIAN_POINT ( 'NONE',  ( 185.1979166673494603, 6.668395609140176816, 3.850000000000000977 ) ) ;
#63905 = ADVANCED_FACE ( 'NONE', ( #18584 ), #50002, .T. ) ;
#63906 = DIRECTION ( 'NONE',  ( 0.000000000000000000, 0.000000000000000000, 1.000000000000000000 ) ) ;
#63907 = CARTESIAN_POINT ( 'NONE',  ( -9.150000000000009237, 2.500000000000000000, -7.188010851410848723 ) ) ;
#63908 = AXIS2_PLACEMENT_3D ( 'NONE', #3302, #73975, #32788 ) ;
#63909 = ADVANCED_FACE ( 'NONE', ( #90536 ), #116878, .T. ) ;
#63910 = DIRECTION ( 'NONE',  ( -0.000000000000000000, 1.000000000000000000, -0.000000000000000000 ) ) ;
#63911 = AXIS2_PLACEMENT_3D ( 'NONE', #119394, #70319, #38953 ) ;
#63912 = EDGE_CURVE ( 'NONE', #61265, #96534, #125309, .T. ) ;
#63913 = LINE ( 'NONE', #33179, #94887 ) ;
#63914 = EDGE_CURVE ( 'NONE', #10784, #62494, #119056, .T. ) ;
#63915 = CARTESIAN_POINT ( 'NONE',  ( 10.84999999999991260, 12.50000000000000000, -2.922977105672691422 ) ) ;
#63916 = CARTESIAN_POINT ( 'NONE',  ( 2.899999999999944844, 2.500000000000000000, 3.537306695894645081 ) ) ;
#63917 = AXIS2_PLACEMENT_3D ( 'NONE', #69593, #90519, #30341 ) ;
#63918 = EDGE_CURVE ( 'NONE', #64313, #109253, #109548, .T. ) ;
#63919 = VERTEX_POINT ( 'NONE', #80740 ) ;
#63920 = EDGE_LOOP ( 'NONE', ( #20002, #50133 ) ) ;
#63921 = ORIENTED_EDGE ( 'NONE', *, *, #49869, .T. ) ;
#63922 = ORIENTED_EDGE ( 'NONE', *, *, #123634, .F. ) ;
#63923 = AXIS2_PLACEMENT_3D ( 'NONE', #81244, #2019, #110686 ) ;
#63924 = ORIENTED_EDGE ( 'NONE', *, *, #55551, .F. ) ;
#63925 = DIRECTION ( 'NONE',  ( 0.000000000000000000, 0.000000000000000000, -1.000000000000000000 ) ) ;
#63926 = DIRECTION ( 'NONE',  ( 0.000000000000000000, 0.000000000000000000, 1.000000000000000000 ) ) ;
#63927 = ORIENTED_EDGE ( 'NONE', *, *, #24810, .F. ) ;
#63928 = FACE_BOUND ( 'NONE', #70082, .T. ) ;
#63929 = EDGE_CURVE ( 'NONE', #126052, #47870, #85592, .T. ) ;
#63930 = DIRECTION ( 'NONE',  ( -0.000000000000000000, -1.000000000000000000, -0.000000000000000000 ) ) ;
#63931 = EDGE_CURVE ( 'NONE', #105257, #38338, #129455, .T. ) ;
#63932 = EDGE_LOOP ( 'NONE', ( #36622, #106487, #126181, #83939 ) ) ;
#63933 = DIRECTION ( 'NONE',  ( -4.274815082592931898E-19, -0.9999939076577903929, -0.003490651415223739937 ) ) ;
#63934 = CARTESIAN_POINT ( 'NONE',  ( 11.24999999999994493, 2.500000000000000000, 6.595190528383296780 ) ) ;
#63935 = DIRECTION ( 'NONE',  ( 0.000000000000000000, 0.000000000000000000, 1.000000000000000000 ) ) ;
#63937 = EDGE_LOOP ( 'NONE', ( #53945, #122578 ) ) ;
#63936 = AXIS2_PLACEMENT_3D ( 'NONE', #100781, #109983, #100163 ) ;
#63938 = CARTESIAN_POINT ( 'NONE',  ( 16.56576425164991306, -2.499999999999999556, 6.084390597445977100 ) ) ;
#63939 = VERTEX_POINT ( 'NONE', #44674 ) ;
#63940 = ORIENTED_EDGE ( 'NONE', *, *, #117058, .F. ) ;
#63941 = VERTEX_POINT ( 'NONE', #101665 ) ;
#63942 = DIRECTION ( 'NONE',  ( 0.000000000000000000, 0.000000000000000000, 1.000000000000000000 ) ) ;
#63943 = DIRECTION ( 'NONE',  ( 0.000000000000000000, 1.000000000000000000, 0.000000000000000000 ) ) ;
#63944 = CIRCLE ( 'NONE', #17963, 0.06509327318403743123 ) ;
#63945 = CARTESIAN_POINT ( 'NONE',  ( 13.54999999999990123, 2.500000000000000000, 1.818653347947321475 ) ) ;
#63946 = ORIENTED_EDGE ( 'NONE', *, *, #74813, .T. ) ;
#63947 = CARTESIAN_POINT ( 'NONE',  ( 9.149999999999920419, 12.50000000000000000, 1.537336459617582918 ) ) ;
#63948 = AXIS2_PLACEMENT_3D ( 'NONE', #124612, #106881, #57153 ) ;
#63949 = AXIS2_PLACEMENT_3D ( 'NONE', #80831, #121381, #91930 ) ;
#63950 = FACE_OUTER_BOUND ( 'NONE', #107362, .T. ) ;
#63951 = DIRECTION ( 'NONE',  ( 0.000000000000000000, 0.000000000000000000, 1.000000000000000000 ) ) ;
#63952 = CARTESIAN_POINT ( 'NONE',  ( 185.7812500006828031, 0.000000000000000000, 7.700000000000000178 ) ) ;
#63953 = EDGE_LOOP ( 'NONE', ( #128293, #71240 ) ) ;
#63954 = DIRECTION ( 'NONE',  ( 0.000000000000000000, 0.000000000000000000, 1.000000000000000000 ) ) ;
#63955 = VERTEX_POINT ( 'NONE', #2806 ) ;
#63956 = DIRECTION ( 'NONE',  ( 0.000000000000000000, 0.000000000000000000, 1.000000000000000000 ) ) ;
#63957 = CIRCLE ( 'NONE', #28368, 0.1000000000000002554 ) ;
#63958 = ORIENTED_EDGE ( 'NONE', *, *, #5515, .F. ) ;
#63959 = ADVANCED_FACE ( 'NONE', ( #82008 ), #4088, .T. ) ;
#63960 = CIRCLE ( 'NONE', #5447, 0.06509327318403745899 ) ;
#63961 = ORIENTED_EDGE ( 'NONE', *, *, #72074, .T. ) ;
#63962 = LINE ( 'NONE', #14193, #86860 ) ;
#63963 = DIRECTION ( 'NONE',  ( 0.000000000000000000, 1.000000000000000000, 0.000000000000000000 ) ) ;
#63964 = CARTESIAN_POINT ( 'NONE',  ( 6.649999999999929301, 2.500000000000000000, -2.265063509461101798 ) ) ;
#63965 = DIRECTION ( 'NONE',  ( 0.000000000000000000, -0.000000000000000000, 1.000000000000000000 ) ) ;
#63966 = DIRECTION ( 'NONE',  ( 0.000000000000000000, 1.000000000000000000, 0.000000000000000000 ) ) ;
#63967 = VERTEX_POINT ( 'NONE', #114058 ) ;
#63968 = ORIENTED_EDGE ( 'NONE', *, *, #85722, .T. ) ;
#63969 = ADVANCED_FACE ( 'NONE', ( #13256 ), #127372, .T. ) ;
#63970 = CARTESIAN_POINT ( 'NONE',  ( 11.64999999999990798, 2.500000000000000000, -2.857883832488653741 ) ) ;
#63971 = CONICAL_SURFACE ( 'NONE', #115903, 0.1000000000000000056, 0.003490658503988666988 ) ;
#63972 = AXIS2_PLACEMENT_3D ( 'NONE', #45928, #114018, #76015 ) ;
#63973 = DIRECTION ( 'NONE',  ( 0.000000000000000000, 1.000000000000000000, 0.000000000000000000 ) ) ;
#63974 = CARTESIAN_POINT ( 'NONE',  ( 9.999999999999948486, 2.500000000000000000, -4.230127018922201998 ) ) ;
#63975 = VERTEX_POINT ( 'NONE', #124528 ) ;
#63976 = ORIENTED_EDGE ( 'NONE', *, *, #111922, .T. ) ;
#63977 = CARTESIAN_POINT ( 'NONE',  ( 7.049999999999930544, 2.500000000000000000, -6.495190528383302464 ) ) ;
#63978 = VERTEX_POINT ( 'NONE', #122589 ) ;
#63979 = CARTESIAN_POINT ( 'NONE',  ( 7.499999999999927169, 2.500000000000000000, -5.022947341949754119 ) ) ;
#63980 = DIRECTION ( 'NONE',  ( 0.000000000000000000, 0.000000000000000000, 1.000000000000000000 ) ) ;
#63981 = VERTEX_POINT ( 'NONE', #14543 ) ;
#63982 = DIRECTION ( 'NONE',  ( 0.000000000000000000, 1.000000000000000000, 0.000000000000000000 ) ) ;
#63983 = DIRECTION ( 'NONE',  ( -0.000000000000000000, 1.000000000000000000, -0.000000000000000000 ) ) ;
#63984 = DIRECTION ( 'NONE',  ( 0.000000000000000000, 0.000000000000000000, -1.000000000000000000 ) ) ;
#63985 = CARTESIAN_POINT ( 'NONE',  ( -11.89999999999999680, 12.50000000000000000, -4.676537180435976104 ) ) ;
#63986 = VERTEX_POINT ( 'NONE', #84594 ) ;
#63987 = CARTESIAN_POINT ( 'NONE',  ( -3.350000000000031619, 12.50000000000000000, -5.802370205355749988 ) ) ;
#63988 = CIRCLE ( 'NONE', #34760, 0.06509327318403743123 ) ;
#63989 = CIRCLE ( 'NONE', #59825, 0.06509327318403741736 ) ;
#63990 = CARTESIAN_POINT ( 'NONE',  ( 43.31214921609998925, -3.511364963944068940, 3.941696051831963032 ) ) ;
#63991 = ORIENTED_EDGE ( 'NONE', *, *, #87974, .F. ) ;
#63992 = EDGE_LOOP ( 'NONE', ( #53715, #51960 ) ) ;
#63993 =( REPRESENTATION_RELATIONSHIP ('NONE','NONE', #102928, #18450 ) REPRESENTATION_RELATIONSHIP_WITH_TRANSFORMATION ( #126280 )SHAPE_REPRESENTATION_RELATIONSHIP( ) );
#63994 = CARTESIAN_POINT ( 'NONE',  ( 186.9218750003414016, 0.000000000000000000, 7.564683531250000925 ) ) ;
#63995 = DIRECTION ( 'NONE',  ( 0.000000000000000000, 1.000000000000000000, 0.000000000000000000 ) ) ;
#63996 = DIRECTION ( 'NONE',  ( 0.000000000000000000, 0.000000000000000000, -1.000000000000000000 ) ) ;
#63997 = DIRECTION ( 'NONE',  ( 0.000000000000000000, 1.000000000000000000, 0.000000000000000000 ) ) ;
#64000 = CIRCLE ( 'NONE', #28499, 0.1000000000000000472 ) ;
#63999 = DIRECTION ( 'NONE',  ( -0.000000000000000000, -1.000000000000000000, -0.000000000000000000 ) ) ;
#63998 = AXIS2_PLACEMENT_3D ( 'NONE', #118105, #49394, #97184 ) ;
#64001 = EDGE_CURVE ( 'NONE', #82140, #122182, #34221, .T. ) ;
#64002 = DIRECTION ( 'NONE',  ( 0.000000000000000000, 1.000000000000000000, 0.000000000000000000 ) ) ;
#64003 = CARTESIAN_POINT ( 'NONE',  ( -7.500000000000001776, 2.500000000000000000, 1.734723475976807094E-15 ) ) ;
#64004 = FACE_OUTER_BOUND ( 'NONE', #96829, .T. ) ;
#64005 = DIRECTION ( 'NONE',  ( 0.000000000000000000, 0.000000000000000000, 1.000000000000000000 ) ) ;
#64006 = CARTESIAN_POINT ( 'NONE',  ( 186.3333333333333144, 6.668395609140177704, -3.849999999999998312 ) ) ;
#64007 = DIRECTION ( 'NONE',  ( 0.000000000000000000, 0.000000000000000000, 1.000000000000000000 ) ) ;
#64008 = EDGE_CURVE ( 'NONE', #7770, #93441, #10295, .T. ) ;
#64009 = ORIENTED_EDGE ( 'NONE', *, *, #107595, .T. ) ;
#64010 = VERTEX_POINT ( 'NONE', #23096 ) ;
#64011 = AXIS2_PLACEMENT_3D ( 'NONE', #1337, #9239, #693 ) ;
#64012 = ORIENTED_EDGE ( 'NONE', *, *, #94508, .T. ) ;
#64013 = EDGE_CURVE ( 'NONE', #32792, #123530, #98112, .T. ) ;
#64014 = ORIENTED_EDGE ( 'NONE', *, *, #88398, .F. ) ;
#64015 = EDGE_CURVE ( 'NONE', #20221, #50581, #68862, .T. ) ;
#64016 = CARTESIAN_POINT ( 'NONE',  ( 11.24999999999990941, 2.500000000000000000, -1.472243186433550122 ) ) ;
#64017 = DIRECTION ( 'NONE',  ( -0.000000000000000000, -1.000000000000000000, -0.000000000000000000 ) ) ;
#64018 = EDGE_LOOP ( 'NONE', ( #17759, #14801 ) ) ;
#64019 = CARTESIAN_POINT ( 'NONE',  ( -12.89999999999999147, 12.50000000000000000, 3.702399969078682407 ) ) ;
#64020 = ADVANCED_FACE ( 'NONE', ( #34872 ), #123237, .T. ) ;
#64021 = PLANE ( 'NONE',  #15681 ) ;
#64023 = VERTEX_POINT ( 'NONE', #94398 ) ;
#64022 = DIRECTION ( 'NONE',  ( -0.000000000000000000, 1.000000000000000000, -0.000000000000000000 ) ) ;
#64024 = EDGE_CURVE ( 'NONE', #23353, #115231, #21821, .T. ) ;
#64025 = DIRECTION ( 'NONE',  ( -0.000000000000000000, -1.000000000000000000, -0.000000000000000000 ) ) ;
#64026 = CONICAL_SURFACE ( 'NONE', #126723, 0.1000000000000002554, 0.003490658503988666988 ) ;
#64027 = DIRECTION ( 'NONE',  ( 0.000000000000000000, 0.000000000000000000, 1.000000000000000000 ) ) ;
#64028 = ORIENTED_EDGE ( 'NONE', *, *, #34481, .T. ) ;
#64029 = AXIS2_PLACEMENT_3D ( 'NONE', #118075, #66397, #106330 ) ;
#64030 = ORIENTED_EDGE ( 'NONE', *, *, #28612, .F. ) ;
#64031 = VERTEX_POINT ( 'NONE', #52552 ) ;
#64032 = ORIENTED_EDGE ( 'NONE', *, *, #109572, .F. ) ;
#64033 = CARTESIAN_POINT ( 'NONE',  ( 5.399999999999935518, 12.50000000000000000, -4.330127018922201643 ) ) ;
#64034 = AXIS2_PLACEMENT_3D ( 'NONE', #51549, #110444, #41094 ) ;
#64035 = CARTESIAN_POINT ( 'NONE',  ( 4.349999999999939249, 12.50000000000000000, 2.446380397790835826 ) ) ;
#64036 = DIRECTION ( 'NONE',  ( 0.000000000000000000, 0.000000000000000000, 1.000000000000000000 ) ) ;
#64037 = VECTOR ( 'NONE', #51858, 1000.000000000000000 ) ;
#64038 = DIRECTION ( 'NONE',  ( 0.000000000000000000, 0.000000000000000000, 1.000000000000000000 ) ) ;
#64039 = VERTEX_POINT ( 'NONE', #61751 ) ;
#64040 = CIRCLE ( 'NONE', #9754, 0.06509327318403745899 ) ;
#64041 = DIRECTION ( 'NONE',  ( -0.000000000000000000, -1.000000000000000000, -0.000000000000000000 ) ) ;
#64042 = VERTEX_POINT ( 'NONE', #121942 ) ;
#64043 = CARTESIAN_POINT ( 'NONE',  ( -6.250000000000019540, 2.500000000000000000, -2.857883832488653741 ) ) ;
#64044 = CARTESIAN_POINT ( 'NONE',  ( 12.06068301339626281, -1.499999999999807931, -8.632777000277656043 ) ) ;
#64045 = CARTESIAN_POINT ( 'NONE',  ( -3.750000000000026201, 2.500000000000000000, 5.702370205355745014 ) ) ;
#64046 = CARTESIAN_POINT ( 'NONE',  ( 17.17161331427274007, -0.4678040054248471802, 5.513957101008608142 ) ) ;
#64047 = CIRCLE ( 'NONE', #7602, 0.06509327318403745899 ) ;
#64048 = ORIENTED_EDGE ( 'NONE', *, *, #42693, .T. ) ;
#64049 = ADVANCED_FACE ( 'NONE', ( #4713 ), #111464, .T. ) ;
#64050 = CIRCLE ( 'NONE', #62006, 0.06509327318403745899 ) ;
#64051 = ORIENTED_EDGE ( 'NONE', *, *, #3600, .F. ) ;
#64052 = ORIENTED_EDGE ( 'NONE', *, *, #51221, .T. ) ;
#64053 = CARTESIAN_POINT ( 'NONE',  ( 9.549999999999918998, 2.500000000000000000, 2.065063509461097624 ) ) ;
#64054 = CARTESIAN_POINT ( 'NONE',  ( 7.699999999999925571, 2.500000000000000000, 4.083716857408420609 ) ) ;
#64055 = FACE_OUTER_BOUND ( 'NONE', #120618, .T. ) ;
#64056 = FACE_BOUND ( 'NONE', #23847, .T. ) ;
#64057 = CARTESIAN_POINT ( 'NONE',  ( -6.050000000000017586, 12.50000000000000000, 6.083687093685482772 ) ) ;
#64058 = CARTESIAN_POINT ( 'NONE',  ( 6.449999999999930012, 12.50000000000000000, 6.776507416713035248 ) ) ;
#64059 = EDGE_CURVE ( 'NONE', #9579, #118717, #52153, .T. ) ;
#64060 = DIRECTION ( 'NONE',  ( 0.000000000000000000, 0.000000000000000000, 1.000000000000000000 ) ) ;
#64061 = EDGE_CURVE ( 'NONE', #55669, #15992, #100180, .T. ) ;
#64062 = CARTESIAN_POINT ( 'NONE',  ( 187.1718750003414016, 9.264065473108010111E-16, -7.564683531250000925 ) ) ;
#64063 = CARTESIAN_POINT ( 'NONE',  ( -6.650000000000018119, 2.500000000000000000, -7.088010851410853519 ) ) ;
#64064 = EDGE_CURVE ( 'NONE', #18602, #112155, #106431, .T. ) ;
#64065 = DIRECTION ( 'NONE',  ( 0.000000000000000000, 0.000000000000000000, 1.000000000000000000 ) ) ;
#64066 = VERTEX_POINT ( 'NONE', #32304 ) ;
#64067 = EDGE_CURVE ( 'NONE', #181, #31627, #60492, .T. ) ;
#64068 = DIRECTION ( 'NONE',  ( 0.000000000000000000, 0.000000000000000000, 1.000000000000000000 ) ) ;
#64069 = EDGE_CURVE ( 'NONE', #125139, #56994, #6161, .T. ) ;
#64070 = EDGE_LOOP ( 'NONE', ( #108612, #115383 ) ) ;
#64071 = ORIENTED_EDGE ( 'NONE', *, *, #39833, .F. ) ;
#64072 = ORIENTED_EDGE ( 'NONE', *, *, #40565, .T. ) ;
#64073 = VERTEX_POINT ( 'NONE', #17097 ) ;
#64074 = CARTESIAN_POINT ( 'NONE',  ( -3.950000000000028155, 2.500000000000000000, -6.841600689897077814 ) ) ;
#64075 = FACE_BOUND ( 'NONE', #50165, .T. ) ;
#64076 = DIRECTION ( 'NONE',  ( 0.000000000000000000, 0.000000000000000000, -1.000000000000000000 ) ) ;
#64077 = EDGE_CURVE ( 'NONE', #113211, #64031, #57047, .T. ) ;
#64078 = ADVANCED_FACE ( 'NONE', ( #16472 ), #55772, .T. ) ;
#64079 = CIRCLE ( 'NONE', #16031, 0.06509327318403745899 ) ;
#64080 = CIRCLE ( 'NONE', #43173, 0.06509327318403745899 ) ;
#64081 = ORIENTED_EDGE ( 'NONE', *, *, #126674, .F. ) ;
#64082 = LINE ( 'NONE', #104010, #17458 ) ;
#64083 = CARTESIAN_POINT ( 'NONE',  ( -10.60000000000000320, 2.500000000000000000, -4.776537180435973085 ) ) ;
#64084 = ORIENTED_EDGE ( 'NONE', *, *, #110301, .T. ) ;
#64085 = CARTESIAN_POINT ( 'NONE',  ( 7.899999999999923084, 2.500000000000000000, 0.6928203230275494784 ) ) ;
#64086 = DIRECTION ( 'NONE',  ( -0.000000000000000000, -1.000000000000000000, -0.000000000000000000 ) ) ;
#64087 = AXIS2_PLACEMENT_3D ( 'NONE', #72254, #914, #80125 ) ;
#64088 = ORIENTED_EDGE ( 'NONE', *, *, #16186, .F. ) ;
#64089 = DIRECTION ( 'NONE',  ( 0.000000000000000000, 0.000000000000000000, 1.000000000000000000 ) ) ;
#64090 = DIRECTION ( 'NONE',  ( 0.000000000000000000, 1.000000000000000000, 0.000000000000000000 ) ) ;
#64092 = CIRCLE ( 'NONE', #18022, 0.1000000000000002554 ) ;
#64091 = CONICAL_SURFACE ( 'NONE', #43186, 0.1000000000000000472, 0.003490658503988666988 ) ;
#64093 = ORIENTED_EDGE ( 'NONE', *, *, #45305, .T. ) ;
#64094 = AXIS2_PLACEMENT_3D ( 'NONE', #27410, #107276, #96800 ) ;
#64095 = LINE ( 'NONE', #85017, #57273 ) ;
#64096 = CARTESIAN_POINT ( 'NONE',  ( 13.14999999999989733, 2.500000000000000000, -1.818653347947325916 ) ) ;
#64097 = CARTESIAN_POINT ( 'NONE',  ( -1.250000000000001110, 2.500000000000000000, -6.495190528383302464 ) ) ;
#64098 = ORIENTED_EDGE ( 'NONE', *, *, #125202, .T. ) ;
#64099 = ORIENTED_EDGE ( 'NONE', *, *, #88293, .T. ) ;
#64100 = CARTESIAN_POINT ( 'NONE',  ( 11.24999999999994316, 12.50000000000000000, -6.495190528383302464 ) ) ;
#64101 = EDGE_LOOP ( 'NONE', ( #97086, #65857, #33515, #86206 ) ) ;
#64102 = CARTESIAN_POINT ( 'NONE',  ( -2.500000000000030642, 2.500000000000000000, -4.922947341949753586 ) ) ;
#64103 = CARTESIAN_POINT ( 'NONE',  ( -3.950000000000026379, 12.50000000000000000, 6.841600689897072485 ) ) ;
#64104 = ORIENTED_EDGE ( 'NONE', *, *, #96284, .T. ) ;
#64105 = CARTESIAN_POINT ( 'NONE',  ( 14.59999999999989484, 12.50000000000000000, 0.06509327318403515528 ) ) ;
#64106 = CARTESIAN_POINT ( 'NONE',  ( -9.150000000000005684, 2.500000000000000000, 5.902370205355745192 ) ) ;
#64107 = DIRECTION ( 'NONE',  ( -0.000000000000000000, -1.000000000000000000, -0.000000000000000000 ) ) ;
#64108 = LINE ( 'NONE', #26769, #86288 ) ;
#64109 = CIRCLE ( 'NONE', #70379, 0.06509327318403745899 ) ;
#64110 = DIRECTION ( 'NONE',  ( 0.000000000000000000, 0.000000000000000000, 1.000000000000000000 ) ) ;
#64111 = VECTOR ( 'NONE', #46080, 1000.000000000000000 ) ;
#64112 = EDGE_LOOP ( 'NONE', ( #55745, #35850 ) ) ;
#64113 = EDGE_CURVE ( 'NONE', #104184, #98077, #58424, .T. ) ;
#64114 = ORIENTED_EDGE ( 'NONE', *, *, #47799, .T. ) ;
#64115 = DIRECTION ( 'NONE',  ( 0.000000000000000000, 1.000000000000000000, 0.000000000000000000 ) ) ;
#64116 = CIRCLE ( 'NONE', #103836, 0.1000000000000002554 ) ;
#64117 = CARTESIAN_POINT ( 'NONE',  ( -6.850000000000017408, 12.50000000000000000, -6.213873640053564351 ) ) ;
#64118 = CARTESIAN_POINT ( 'NONE',  ( 5.649999999999934630, 2.500000000000000000, -2.611473670974877592 ) ) ;
#64120 = ORIENTED_EDGE ( 'NONE', *, *, #84372, .F. ) ;
#64119 = ORIENTED_EDGE ( 'NONE', *, *, #13359, .F. ) ;
#64121 = ORIENTED_EDGE ( 'NONE', *, *, #99922, .F. ) ;
#64122 = FACE_OUTER_BOUND ( 'NONE', #119932, .T. ) ;
#64123 = AXIS2_PLACEMENT_3D ( 'NONE', #36420, #107058, #8220 ) ;
#64124 = AXIS2_PLACEMENT_3D ( 'NONE', #44606, #83253, #67941 ) ;
#64125 = CARTESIAN_POINT ( 'NONE',  ( -2.050000000000033129, 12.50000000000000000, 2.099970236277060032 ) ) ;
#64126 = DIRECTION ( 'NONE',  ( 0.000000000000000000, 0.000000000000000000, 1.000000000000000000 ) ) ;
#64127 = CARTESIAN_POINT ( 'NONE',  ( 0.000000000000000000, 0.000000000000000000, 0.000000000000000000 ) ) ;
#64128 = CARTESIAN_POINT ( 'NONE',  ( 10.39999999999990976, 12.50000000000000000, -4.330127018922201643 ) ) ;
#64129 = DIRECTION ( 'NONE',  ( 0.000000000000000000, 0.000000000000000000, 1.000000000000000000 ) ) ;
#64130 = CARTESIAN_POINT ( 'NONE',  ( -6.900000000000019007, 12.50000000000000000, -4.676537180435978769 ) ) ;
#64131 = PLANE ( 'NONE',  #13144 ) ;
#64132 = VECTOR ( 'NONE', #100802, 1000.000000000000000 ) ;
#64133 = PLANE ( 'NONE',  #74916 ) ;
#64134 = CIRCLE ( 'NONE', #5544, 0.06509327318403745899 ) ;
#64135 = ORIENTED_EDGE ( 'NONE', *, *, #6673, .F. ) ;
#64137 = AXIS2_PLACEMENT_3D ( 'NONE', #74721, #117844, #127053 ) ;
#64136 = VECTOR ( 'NONE', #115629, 1000.000000000000000 ) ;
#64138 = DIRECTION ( 'NONE',  ( 0.000000000000000000, 0.000000000000000000, 1.000000000000000000 ) ) ;
#64139 = VERTEX_POINT ( 'NONE', #6630 ) ;
#64140 = ORIENTED_EDGE ( 'NONE', *, *, #93356, .T. ) ;
#64141 = DIRECTION ( 'NONE',  ( -0.000000000000000000, -1.000000000000000000, -0.000000000000000000 ) ) ;
#64142 = DIRECTION ( 'NONE',  ( 0.000000000000000000, 1.000000000000000000, 0.000000000000000000 ) ) ;
#64143 = FACE_OUTER_BOUND ( 'NONE', #51369, .T. ) ;
#64144 = DIRECTION ( 'NONE',  ( -0.000000000000000000, 1.000000000000000000, -0.000000000000000000 ) ) ;
#64145 = CARTESIAN_POINT ( 'NONE',  ( 9.349999999999919709, 2.500000000000000000, -6.148780366869526226 ) ) ;
#64146 = PLANE ( 'NONE',  #51117 ) ;
#64147 = CARTESIAN_POINT ( 'NONE',  ( 11.64999999999990798, 2.500000000000000000, -2.857883832488653741 ) ) ;
#64148 = EDGE_LOOP ( 'NONE', ( #7535, #84839 ) ) ;
#64149 = CARTESIAN_POINT ( 'NONE',  ( 5.849999999999933920, 2.500000000000000000, -2.857883832488653741 ) ) ;
#64150 = AXIS2_PLACEMENT_3D ( 'NONE', #84875, #93413, #124811 ) ;
#64151 = DIRECTION ( 'NONE',  ( -4.274815082592931898E-19, -0.9999939076577903929, -0.003490651415223739937 ) ) ;
#64152 = ORIENTED_EDGE ( 'NONE', *, *, #50076, .F. ) ;
#64153 = EDGE_CURVE ( 'NONE', #66867, #49607, #50032, .T. ) ;
#64154 = ORIENTED_EDGE ( 'NONE', *, *, #117203, .F. ) ;
#64155 = ORIENTED_EDGE ( 'NONE', *, *, #113078, .F. ) ;
#64156 = EDGE_CURVE ( 'NONE', #3522, #98275, #87156, .T. ) ;
#64157 = VERTEX_POINT ( 'NONE', #15179 ) ;
#64158 = EDGE_CURVE ( 'NONE', #35476, #56841, #112800, .T. ) ;
#64159 = LINE ( 'NONE', #94264, #71320 ) ;
#64160 = DIRECTION ( 'NONE',  ( 0.000000000000000000, 0.000000000000000000, -1.000000000000000000 ) ) ;
#64161 = CONICAL_SURFACE ( 'NONE', #60078, 0.1000000000000002554, 0.003490658503988666988 ) ;
#64162 = CARTESIAN_POINT ( 'NONE',  ( 115.5000000000000000, 0.000000000000000000, 0.000000000000000000 ) ) ;
#64164 = DIRECTION ( 'NONE',  ( -4.274815082592931898E-19, -0.9999939076577903929, -0.003490651415223739937 ) ) ;
#64163 = CIRCLE ( 'NONE', #22432, 0.1000000000000002554 ) ;
#64165 = ADVANCED_FACE ( 'NONE', ( #65590 ), #1961, .T. ) ;
#64166 = DIRECTION ( 'NONE',  ( 0.000000000000000000, -0.000000000000000000, 1.000000000000000000 ) ) ;
#64168 = ORIENTED_EDGE ( 'NONE', *, *, #48710, .F. ) ;
#64167 = EDGE_CURVE ( 'NONE', #87148, #77466, #47952, .T. ) ;
#64169 = DIRECTION ( 'NONE',  ( 0.000000000000000000, 1.000000000000000000, 0.000000000000000000 ) ) ;
#64170 = EDGE_CURVE ( 'NONE', #5316, #61065, #27021, .T. ) ;
#64171 = EDGE_CURVE ( 'NONE', #111830, #21908, #43762, .T. ) ;
#64172 = DIRECTION ( 'NONE',  ( 0.000000000000000000, 0.000000000000000000, 1.000000000000000000 ) ) ;
#64174 = VECTOR ( 'NONE', #32660, 1000.000000000000000 ) ;
#64173 = AXIS2_PLACEMENT_3D ( 'NONE', #87688, #16350, #17660 ) ;
#64175 = FACE_OUTER_BOUND ( 'NONE', #18632, .T. ) ;
#64176 = VERTEX_POINT ( 'NONE', #66229 ) ;
#64177 = EDGE_LOOP ( 'NONE', ( #2747, #126235 ) ) ;
#64178 = EDGE_LOOP ( 'NONE', ( #545, #85303 ) ) ;
#64179 = DIRECTION ( 'NONE',  ( 0.000000000000000000, 0.000000000000000000, 1.000000000000000000 ) ) ;
#64181 = VECTOR ( 'NONE', #81763, 1000.000000000000000 ) ;
#64180 = CIRCLE ( 'NONE', #24479, 0.06509327318403745899 ) ;
#64182 = CARTESIAN_POINT ( 'NONE',  ( -8.350000000000013856, 12.50000000000000000, -2.165063509461101710 ) ) ;
#64183 = DIRECTION ( 'NONE',  ( -4.274815082592931898E-19, -0.9999939076577903929, -0.003490651415223739937 ) ) ;
#64184 = CIRCLE ( 'NONE', #51685, 0.06509327318403745899 ) ;
#64185 = ORIENTED_EDGE ( 'NONE', *, *, #86303, .F. ) ;
#64186 = CARTESIAN_POINT ( 'NONE',  ( -6.249999999999981348, 2.500000000000000000, 2.165063509461097713 ) ) ;
#64187 = CARTESIAN_POINT ( 'NONE',  ( 0.8499999999999553468, 2.500000000000000000, -2.165063509461101710 ) ) ;
#64188 = CARTESIAN_POINT ( 'NONE',  ( 0.3999999999999568345, 2.500000000000000000, -4.922947341949753586 ) ) ;
#64189 = DIRECTION ( 'NONE',  ( 0.000000000000000000, -0.9999939076577903929, 0.003490651415223739937 ) ) ;
#64190 = DIRECTION ( 'NONE',  ( -0.000000000000000000, 1.000000000000000000, -0.000000000000000000 ) ) ;
#64191 = EDGE_LOOP ( 'NONE', ( #83324, #49581, #119621, #34348 ) ) ;
#64192 = ORIENTED_EDGE ( 'NONE', *, *, #12849, .F. ) ;
#64193 = EDGE_CURVE ( 'NONE', #47717, #56128, #104381, .T. ) ;
#64194 = CARTESIAN_POINT ( 'NONE',  ( 187.0000000000000000, 0.000000000000000000, 7.700000000000000178 ) ) ;
#64195 = DIRECTION ( 'NONE',  ( 0.000000000000000000, -0.9999939076577903929, 0.003490651415223739937 ) ) ;
#64196 = CONICAL_SURFACE ( 'NONE', #32831, 0.09999999999999982514, 0.003490658503988666988 ) ;
#64197 = DIRECTION ( 'NONE',  ( 0.000000000000000000, 0.000000000000000000, -1.000000000000000000 ) ) ;
#64198 = DIRECTION ( 'NONE',  ( 0.000000000000000000, 0.000000000000000000, 1.000000000000000000 ) ) ;
#64199 = AXIS2_PLACEMENT_3D ( 'NONE', #52509, #20489, #31594 ) ;
#64200 = CARTESIAN_POINT ( 'NONE',  ( -9.999999999999969802, 2.500000000000000000, 4.330127018922196314 ) ) ;
#64201 = EDGE_LOOP ( 'NONE', ( #95366, #120006 ) ) ;
#64202 = CONICAL_SURFACE ( 'NONE', #43301, 0.09999999999999982514, 0.003490658503988666988 ) ;
#64203 = ADVANCED_FACE ( 'NONE', ( #57719 ), #24955, .T. ) ;
#64204 = EDGE_LOOP ( 'NONE', ( #42901, #87381, #78099, #115431 ) ) ;
#64205 = EDGE_CURVE ( 'NONE', #104031, #2125, #81413, .T. ) ;
#64206 = DIRECTION ( 'NONE',  ( 0.000000000000000000, -0.000000000000000000, 1.000000000000000000 ) ) ;
#64207 = CARTESIAN_POINT ( 'NONE',  ( 11.24999999999994493, 12.50000000000000000, 6.495190528383297135 ) ) ;
#64209 = CARTESIAN_POINT ( 'NONE',  ( 18.00406199218826231, -1.510509990051560170, -4.944015969580405567 ) ) ;
#64208 = CONICAL_SURFACE ( 'NONE', #7774, 0.09999999999999982514, 0.003490658503988666988 ) ;
#64210 = EDGE_CURVE ( 'NONE', #78150, #33245, #113110, .T. ) ;
#64212 = FACE_OUTER_BOUND ( 'NONE', #69718, .T. ) ;
#64211 = CIRCLE ( 'NONE', #11984, 0.1000000000000002554 ) ;
#64213 = VERTEX_POINT ( 'NONE', #7953 ) ;
#64214 = DIRECTION ( 'NONE',  ( 0.000000000000000000, 0.000000000000000000, -1.000000000000000000 ) ) ;
#64215 = AXIS2_PLACEMENT_3D ( 'NONE', #74653, #93658, #24915 ) ;
#64216 = CARTESIAN_POINT ( 'NONE',  ( 8.349999999999923261, 12.50000000000000000, -7.188010851410854052 ) ) ;
#64217 = EDGE_CURVE ( 'NONE', #99657, #53810, #92177, .T. ) ;
#64218 = ORIENTED_EDGE ( 'NONE', *, *, #109906, .T. ) ;
#64219 = DIRECTION ( 'NONE',  ( -0.000000000000000000, 1.000000000000000000, -0.000000000000000000 ) ) ;
#64220 = AXIS2_PLACEMENT_3D ( 'NONE', #52861, #80398, #22134 ) ;
#64221 = EDGE_CURVE ( 'NONE', #2505, #87803, #73393, .T. ) ;
#64222 = ORIENTED_EDGE ( 'NONE', *, *, #52692, .F. ) ;
#64223 = DIRECTION ( 'NONE',  ( 0.000000000000000000, 1.000000000000000000, 0.000000000000000000 ) ) ;
#64224 = EDGE_CURVE ( 'NONE', #15992, #55669, #46213, .T. ) ;
#64225 = EDGE_CURVE ( 'NONE', #54758, #20844, #86512, .T. ) ;
#64227 = EDGE_CURVE ( 'NONE', #58259, #3309, #95294, .T. ) ;
#64226 = CIRCLE ( 'NONE', #101888, 0.1000000000000002554 ) ;
#64228 = EDGE_LOOP ( 'NONE', ( #99371, #13278, #22643, #47350 ) ) ;
#64229 = CARTESIAN_POINT ( 'NONE',  ( -5.400000000000024336, 12.50000000000000000, -3.572213422710612374 ) ) ;
#64230 = DIRECTION ( 'NONE',  ( 0.000000000000000000, 0.000000000000000000, -1.000000000000000000 ) ) ;
#64231 = ORIENTED_EDGE ( 'NONE', *, *, #66093, .T. ) ;
#64232 = ORIENTED_EDGE ( 'NONE', *, *, #38028, .F. ) ;
#64233 = CARTESIAN_POINT ( 'NONE',  ( 185.5468750003414300, -8.734944146203032389, -1.604583208406768146E-15 ) ) ;
#64234 = DIRECTION ( 'NONE',  ( 0.000000000000000000, 1.000000000000000000, 0.000000000000000000 ) ) ;
#64235 = EDGE_CURVE ( 'NONE', #49584, #81973, #25266, .T. ) ;
#64236 = CARTESIAN_POINT ( 'NONE',  ( 2.899999999999946620, 12.50000000000000000, -3.637306695894650055 ) ) ;
#64237 = DIRECTION ( 'NONE',  ( 0.000000000000000000, 0.000000000000000000, 1.000000000000000000 ) ) ;
#64238 = DIRECTION ( 'NONE',  ( -0.000000000000000000, 1.000000000000000000, -0.000000000000000000 ) ) ;
#64239 = LINE ( 'NONE', #74063, #128346 ) ;
#64240 = DIRECTION ( 'NONE',  ( 0.000000000000000000, 0.000000000000000000, 1.000000000000000000 ) ) ;
#64241 = CARTESIAN_POINT ( 'NONE',  ( -11.24999999999999822, 12.50000000000000000, 1.407149913249508000 ) ) ;
#64242 = VERTEX_POINT ( 'NONE', #59672 ) ;
#64243 = ORIENTED_EDGE ( 'NONE', *, *, #55463, .F. ) ;
#64244 = CARTESIAN_POINT ( 'NONE',  ( -0.6500000000000403233, 2.500000000000000000, 1.818653347947321475 ) ) ;
#64245 = DIRECTION ( 'NONE',  ( 0.000000000000000000, 0.000000000000000000, -1.000000000000000000 ) ) ;
#64246 = CARTESIAN_POINT ( 'NONE',  ( -5.200000000000024158, 2.500000000000000000, -4.576537180435977348 ) ) ;
#64248 = EDGE_LOOP ( 'NONE', ( #115993, #38735, #31891, #6675 ) ) ;
#64247 = ORIENTED_EDGE ( 'NONE', *, *, #22845, .T. ) ;
#64249 = CARTESIAN_POINT ( 'NONE',  ( -1.900000000000034550, 12.50000000000000000, 4.741630453620009789 ) ) ;
#64250 = EDGE_LOOP ( 'NONE', ( #43392, #113822 ) ) ;
#64251 = CARTESIAN_POINT ( 'NONE',  ( -11.25000000000000000, 12.50000000000000000, 7.188010851410848723 ) ) ;
#64252 = CARTESIAN_POINT ( 'NONE',  ( 17.50000000000000000, -2.500000000000000000, 2.922290670089274567 ) ) ;
#64253 = ORIENTED_EDGE ( 'NONE', *, *, #114875, .F. ) ;
#64254 = DIRECTION ( 'NONE',  ( -4.274815082592931898E-19, -0.9999939076577903929, -0.003490651415223739937 ) ) ;
#64255 = CARTESIAN_POINT ( 'NONE',  ( -8.100000000000013856, 12.50000000000000000, -4.048810130592463530 ) ) ;
#64256 = AXIS2_PLACEMENT_3D ( 'NONE', #97774, #118051, #118698 ) ;
#64257 = DIRECTION ( 'NONE',  ( -0.000000000000000000, -1.000000000000000000, -0.000000000000000000 ) ) ;
#64258 = CIRCLE ( 'NONE', #1560, 0.1000000000000002554 ) ;
#64259 = PLANE ( 'NONE',  #61266 ) ;
#64260 = DIRECTION ( 'NONE',  ( -0.000000000000000000, 1.000000000000000000, -0.000000000000000000 ) ) ;
#64261 = CARTESIAN_POINT ( 'NONE',  ( -11.25000000000000000, 2.500000000000000000, 2.957883832488649389 ) ) ;
#64262 = CARTESIAN_POINT ( 'NONE',  ( 186.7343750003414016, 8.734944146203032389, 5.348610694689227483E-16 ) ) ;
#64263 = PLANE ( 'NONE',  #59035 ) ;
#64264 = CARTESIAN_POINT ( 'NONE',  ( -4.999999999999986677, 2.500000000000000000, -2.276824562219559311E-15 ) ) ;
#64266 = CIRCLE ( 'NONE', #112865, 0.06509327318403745899 ) ;
#64265 = VECTOR ( 'NONE', #14282, 1000.000000000000000 ) ;
#64267 = ORIENTED_EDGE ( 'NONE', *, *, #8150, .F. ) ;
#64268 = ORIENTED_EDGE ( 'NONE', *, *, #46810, .T. ) ;
#64269 = VECTOR ( 'NONE', #74122, 1000.000000000000000 ) ;
#64270 = EDGE_CURVE ( 'NONE', #8618, #3902, #91035, .T. ) ;
#64271 = ORIENTED_EDGE ( 'NONE', *, *, #29648, .T. ) ;
#64272 = CARTESIAN_POINT ( 'NONE',  ( 10.84999999999991260, 12.50000000000000000, 7.253104124594885960 ) ) ;
#64273 = ORIENTED_EDGE ( 'NONE', *, *, #91656, .T. ) ;
#64275 = ORIENTED_EDGE ( 'NONE', *, *, #24080, .T. ) ;
#64274 = VERTEX_POINT ( 'NONE', #108086 ) ;
#64276 = ORIENTED_EDGE ( 'NONE', *, *, #80337, .T. ) ;
#64277 = DIRECTION ( 'NONE',  ( 0.000000000000000000, -0.000000000000000000, 1.000000000000000000 ) ) ;
#64279 = VECTOR ( 'NONE', #30767, 1000.000000000000000 ) ;
#64278 = CIRCLE ( 'NONE', #101662, 0.1000000000000002554 ) ;
#64280 = CONICAL_SURFACE ( 'NONE', #89327, 0.09999999999999982514, 0.003490658503988666988 ) ;
#64281 = PLANE ( 'NONE',  #44682 ) ;
#64282 = CARTESIAN_POINT ( 'NONE',  ( -0.6500000000000389910, 2.500000000000000000, -1.718653347947326049 ) ) ;
#64283 = DIRECTION ( 'NONE',  ( 0.000000000000000000, 0.000000000000000000, -1.000000000000000000 ) ) ;
#64284 = DIRECTION ( 'NONE',  ( 0.000000000000000000, -0.9999939076577903929, 0.003490651415223739937 ) ) ;
#64285 = EDGE_CURVE ( 'NONE', #127796, #113021, #87959, .T. ) ;
#64286 = VERTEX_POINT ( 'NONE', #77990 ) ;
#64287 = DIRECTION ( 'NONE',  ( -0.000000000000000000, 1.000000000000000000, -0.000000000000000000 ) ) ;
#64288 = EDGE_LOOP ( 'NONE', ( #46448, #58999 ) ) ;
#64289 = AXIS2_PLACEMENT_3D ( 'NONE', #34340, #74245, #91099 ) ;
#64290 = ORIENTED_EDGE ( 'NONE', *, *, #42449, .F. ) ;
#64291 = ORIENTED_EDGE ( 'NONE', *, *, #37490, .T. ) ;
#64292 = AXIS2_PLACEMENT_3D ( 'NONE', #17241, #24519, #106925 ) ;
#64293 = DIRECTION ( 'NONE',  ( -0.000000000000000000, 1.000000000000000000, -0.000000000000000000 ) ) ;
#64294 = EDGE_LOOP ( 'NONE', ( #81982, #60462, #27925, #42223 ) ) ;
#64295 = ORIENTED_EDGE ( 'NONE', *, *, #3194, .F. ) ;
#64296 = ORIENTED_EDGE ( 'NONE', *, *, #89048, .T. ) ;
#64297 = AXIS2_PLACEMENT_3D ( 'NONE', #104994, #80387, #15322 ) ;
#64299 = FILL_AREA_STYLE_COLOUR ( '', #40341 ) ;
#64298 = CONICAL_SURFACE ( 'NONE', #85230, 0.09999999999999982514, 0.003490658503988666988 ) ;
#64300 = DIRECTION ( 'NONE',  ( 0.000000000000000000, 0.000000000000000000, 1.000000000000000000 ) ) ;
#64302 = AXIS2_PLACEMENT_3D ( 'NONE', #44886, #44213, #104433 ) ;
#64301 = DIRECTION ( 'NONE',  ( 0.000000000000000000, 1.000000000000000000, 0.000000000000000000 ) ) ;
#64303 = DIRECTION ( 'NONE',  ( -0.000000000000000000, 1.000000000000000000, -0.000000000000000000 ) ) ;
#64304 = DIRECTION ( 'NONE',  ( -0.000000000000000000, -1.000000000000000000, -0.000000000000000000 ) ) ;
#64305 = DIRECTION ( 'NONE',  ( -0.000000000000000000, 1.000000000000000000, -0.000000000000000000 ) ) ;
#64306 = CIRCLE ( 'NONE', #110369, 0.09999999999999999167 ) ;
#64308 = CIRCLE ( 'NONE', #5796, 0.06509327318403745899 ) ;
#64307 = DIRECTION ( 'NONE',  ( -0.000000000000000000, -1.000000000000000000, -0.000000000000000000 ) ) ;
#64309 = VERTEX_POINT ( 'NONE', #89104 ) ;
#64310 = AXIS2_PLACEMENT_3D ( 'NONE', #27317, #16835, #105252 ) ;
#64311 = CARTESIAN_POINT ( 'NONE',  ( 8.949999999999915801, 2.500000000000000000, -1.818653347947326138 ) ) ;
#64312 = EDGE_CURVE ( 'NONE', #43648, #96511, #49838, .T. ) ;
#64313 = VERTEX_POINT ( 'NONE', #80580 ) ;
#64314 = CARTESIAN_POINT ( 'NONE',  ( 2.499999999999983569, 12.50000000000000000, -2.276824562219559311E-15 ) ) ;
#64315 = VERTEX_POINT ( 'NONE', #40012 ) ;
#64316 = AXIS2_PLACEMENT_3D ( 'NONE', #114350, #14832, #94707 ) ;
#64317 = ORIENTED_EDGE ( 'NONE', *, *, #66857, .F. ) ;
#64318 = ADVANCED_FACE ( 'NONE', ( #79923 ), #20366, .T. ) ;
#64319 = CARTESIAN_POINT ( 'NONE',  ( 7.499999999999923617, 2.500000000000000000, 0.7928203230275495672 ) ) ;
#64320 = DIRECTION ( 'NONE',  ( 0.000000000000000000, 0.000000000000000000, -1.000000000000000000 ) ) ;
#64322 = AXIS2_PLACEMENT_3D ( 'NONE', #37075, #37710, #19337 ) ;
#64321 = MECHANICAL_DESIGN_GEOMETRIC_PRESENTATION_REPRESENTATION (  '', ( #70589 ), #116544 ) ;
#64323 = CARTESIAN_POINT ( 'NONE',  ( -9.600000000000006750, 2.500000000000000000, 3.637306695894644726 ) ) ;
#64324 = ORIENTED_EDGE ( 'NONE', *, *, #49751, .F. ) ;
#64325 = EDGE_CURVE ( 'NONE', #38043, #96705, #6467, .T. ) ;
#64326 = LINE ( 'NONE', #55159, #15689 ) ;
#64328 = ORIENTED_EDGE ( 'NONE', *, *, #36335, .F. ) ;
#64327 = EDGE_CURVE ( 'NONE', #118169, #18418, #79662, .T. ) ;
#64329 =( BOUNDED_CURVE ( )  B_SPLINE_CURVE ( 2, ( #44943, #15457, #94670, #124787, #35136, #56662, #95325 ),
 .UNSPECIFIED., .F., .F. ) 
 B_SPLINE_CURVE_WITH_KNOTS ( ( 3, 2, 2, 3 ),
 ( 0.1428571428571429880, 0.1666666666666668239, 0.1904761904761906322, 0.2142857142857144681 ),
 .UNSPECIFIED. ) 
 CURVE ( )  GEOMETRIC_REPRESENTATION_ITEM ( )  RATIONAL_B_SPLINE_CURVE ( ( 0.9999999999999992228, 0.8660254037844394848, 1.000000000000000000, 0.8660254037844387076, 1.000000000000000000, 0.8660254037844375974, 1.000000000000001110 ) ) 
 REPRESENTATION_ITEM ( '' )  );
#64330 = CARTESIAN_POINT ( 'NONE',  ( -0.8000000000000381251, 2.500000000000000000, 4.230127018922196669 ) ) ;
#64331 = FACE_OUTER_BOUND ( 'NONE', #72729, .T. ) ;
#64332 = EDGE_CURVE ( 'NONE', #103079, #100426, #75453, .T. ) ;
#64333 = FACE_OUTER_BOUND ( 'NONE', #42830, .T. ) ;
#64334 = EDGE_CURVE ( 'NONE', #35473, #92869, #60924, .T. ) ;
#64335 = ADVANCED_FACE ( 'NONE', ( #100835 ), #104693, .T. ) ;
#64336 = DIRECTION ( 'NONE',  ( 0.000000000000000000, 0.000000000000000000, 1.000000000000000000 ) ) ;
#64337 = DIRECTION ( 'NONE',  ( 0.000000000000000000, -0.9999939076577903929, 0.003490651415223739937 ) ) ;
#64338 = EDGE_LOOP ( 'NONE', ( #2209, #126666 ) ) ;
#64339 = EDGE_CURVE ( 'NONE', #41615, #42781, #2287, .T. ) ;
#64340 = ORIENTED_EDGE ( 'NONE', *, *, #28607, .T. ) ;
#64341 = EDGE_CURVE ( 'NONE', #120440, #8844, #44159, .T. ) ;
#64342 = PLANE ( 'NONE',  #4702 ) ;
#64343 = DIRECTION ( 'NONE',  ( -0.000000000000000000, 1.000000000000000000, -0.000000000000000000 ) ) ;
#64344 = EDGE_CURVE ( 'NONE', #107746, #49994, #35757, .T. ) ;
#64345 = CARTESIAN_POINT ( 'NONE',  ( 184.5052083336747444, -6.551208109652278289, 3.782341765624995134 ) ) ;
#64346 = CARTESIAN_POINT ( 'NONE',  ( -7.700000000000012612, 2.500000000000000000, 4.776537180435972196 ) ) ;
#64347 = CARTESIAN_POINT ( 'NONE',  ( -8.350000000000008527, 12.50000000000000000, 7.188010851410848723 ) ) ;
#64348 = DIRECTION ( 'NONE',  ( 0.000000000000000000, 0.000000000000000000, 1.000000000000000000 ) ) ;
#64349 = CARTESIAN_POINT ( 'NONE',  ( -5.000000000000026645, 2.500000000000000000, -3.537306695894649966 ) ) ;
#64350 = VERTEX_POINT ( 'NONE', #68814 ) ;
#64351 = DIRECTION ( 'NONE',  ( 0.000000000000000000, 0.000000000000000000, 1.000000000000000000 ) ) ;
#64352 = AXIS2_PLACEMENT_3D ( 'NONE', #113286, #51172, #12509 ) ;
#64353 = LINE ( 'NONE', #14593, #86053 ) ;
#64354 = DIRECTION ( 'NONE',  ( 0.000000000000000000, 0.000000000000000000, 1.000000000000000000 ) ) ;
#64355 = ORIENTED_EDGE ( 'NONE', *, *, #100123, .F. ) ;
#64356 = CIRCLE ( 'NONE', #76891, 0.1000000000000000472 ) ;
#64357 = DIRECTION ( 'NONE',  ( 0.000000000000000000, 0.000000000000000000, 1.000000000000000000 ) ) ;
#64358 = AXIS2_PLACEMENT_3D ( 'NONE', #101493, #62220, #110654 ) ;
#64359 = CIRCLE ( 'NONE', #7919, 0.1000000000000002554 ) ;
#64360 = ORIENTED_EDGE ( 'NONE', *, *, #9385, .F. ) ;
#64361 = DIRECTION ( 'NONE',  ( -0.000000000000000000, 1.000000000000000000, -0.000000000000000000 ) ) ;
#64362 = ORIENTED_EDGE ( 'NONE', *, *, #77905, .F. ) ;
#64363 = DIRECTION ( 'NONE',  ( 0.000000000000000000, 0.000000000000000000, -1.000000000000000000 ) ) ;
#64364 = DIRECTION ( 'NONE',  ( 0.000000000000000000, 1.000000000000000000, 0.000000000000000000 ) ) ;
#64365 = DIRECTION ( 'NONE',  ( 0.000000000000000000, 0.000000000000000000, 1.000000000000000000 ) ) ;
#64366 = ORIENTED_EDGE ( 'NONE', *, *, #110666, .F. ) ;
#64367 = AXIS2_PLACEMENT_3D ( 'NONE', #16405, #127676, #76651 ) ;
#64368 = DIRECTION ( 'NONE',  ( 0.000000000000000000, -0.000000000000000000, 1.000000000000000000 ) ) ;
#64369 = DIRECTION ( 'NONE',  ( 0.000000000000000000, 0.000000000000000000, 1.000000000000000000 ) ) ;
#64370 = CONICAL_SURFACE ( 'NONE', #97819, 0.1000000000000002554, 0.003490658503988666988 ) ;
#64371 = ADVANCED_FACE ( 'NONE', ( #19047 ), #59001, .T. ) ;
#64372 = EDGE_LOOP ( 'NONE', ( #40966, #1461, #89694, #53644 ) ) ;
#64373 = DIRECTION ( 'NONE',  ( -0.000000000000000000, 1.000000000000000000, -0.000000000000000000 ) ) ;
#64374 = EDGE_CURVE ( 'NONE', #86499, #85590, #24195, .T. ) ;
#64375 = VECTOR ( 'NONE', #45719, 1000.000000000000000 ) ;
#64376 = ORIENTED_EDGE ( 'NONE', *, *, #982, .T. ) ;
#64377 = ADVANCED_FACE ( 'NONE', ( #53049 ), #117283, .T. ) ;
#64378 = ORIENTED_EDGE ( 'NONE', *, *, #99197, .T. ) ;
#64379 = FACE_OUTER_BOUND ( 'NONE', #18530, .T. ) ;
#64380 = DIRECTION ( 'NONE',  ( 0.000000000000000000, 1.000000000000000000, 0.000000000000000000 ) ) ;
#64381 = DIRECTION ( 'NONE',  ( 0.000000000000000000, 0.000000000000000000, -1.000000000000000000 ) ) ;
#64382 = ORIENTED_EDGE ( 'NONE', *, *, #10432, .F. ) ;
#64383 = AXIS2_PLACEMENT_3D ( 'NONE', #117375, #86657, #98398 ) ;
#64384 = DIRECTION ( 'NONE',  ( 0.000000000000000000, 0.000000000000000000, 1.000000000000000000 ) ) ;
#64385 = CARTESIAN_POINT ( 'NONE',  ( 6.899999999999928413, 2.500000000000000000, -4.776537180435977525 ) ) ;
#64386 = AXIS2_PLACEMENT_3D ( 'NONE', #19702, #20345, #38726 ) ;
#64387 = VERTEX_POINT ( 'NONE', #51763 ) ;
#64388 = EDGE_CURVE ( 'NONE', #15926, #64820, #12745, .T. ) ;
#64389 = CARTESIAN_POINT ( 'NONE',  ( 11.24999999999994493, 2.500000000000000000, 6.395190528383296602 ) ) ;
#64390 = CARTESIAN_POINT ( 'NONE',  ( -2.499999999999996003, 2.500000000000000000, -4.330127018922201643 ) ) ;
#64391 = AXIS2_PLACEMENT_3D ( 'NONE', #123914, #3511, #103646 ) ;
#64392 = CARTESIAN_POINT ( 'NONE',  ( 15.39999999999989022, 2.500000000000000000, 0.09999999999999761857 ) ) ;
#64393 = DIRECTION ( 'NONE',  ( 0.000000000000000000, 1.000000000000000000, 0.000000000000000000 ) ) ;
#64394 = DIRECTION ( 'NONE',  ( -0.000000000000000000, 1.000000000000000000, -0.000000000000000000 ) ) ;
#64395 = CARTESIAN_POINT ( 'NONE',  ( -10.85000000000000142, 12.50000000000000000, -6.495190528383298911 ) ) ;
#64396 = CIRCLE ( 'NONE', #53940, 0.1000000000000002554 ) ;
#64397 = DIRECTION ( 'NONE',  ( -0.000000000000000000, -1.000000000000000000, -0.000000000000000000 ) ) ;
#64398 = ORIENTED_EDGE ( 'NONE', *, *, #109890, .T. ) ;
#64399 = VERTEX_POINT ( 'NONE', #52395 ) ;
#64400 = VERTEX_POINT ( 'NONE', #14387 ) ;
#64401 = ORIENTED_EDGE ( 'NONE', *, *, #18790, .T. ) ;
#64402 = DIRECTION ( 'NONE',  ( 0.000000000000000000, 0.000000000000000000, 1.000000000000000000 ) ) ;
#64403 = DIRECTION ( 'NONE',  ( -0.000000000000000000, -1.000000000000000000, -0.000000000000000000 ) ) ;
#64404 = PLANE ( 'NONE',  #73981 ) ;
#64405 = CIRCLE ( 'NONE', #127122, 0.06509327318403745899 ) ;
#64406 = VERTEX_POINT ( 'NONE', #32786 ) ;
#64407 = FACE_BOUND ( 'NONE', #2176, .T. ) ;
#64408 = EDGE_CURVE ( 'NONE', #9509, #18441, #16931, .T. ) ;
#64409 = PLANE ( 'NONE',  #22869 ) ;
#64410 = DIRECTION ( 'NONE',  ( 0.000000000000000000, 1.000000000000000000, 0.000000000000000000 ) ) ;
#64411 = CARTESIAN_POINT ( 'NONE',  ( -8.749999999999971578, 2.500000000000000000, 6.495190528383297135 ) ) ;
#64413 = VECTOR ( 'NONE', #43935, 1000.000000000000000 ) ;
#64412 = AXIS2_PLACEMENT_3D ( 'NONE', #93769, #46591, #123855 ) ;
#64414 = CARTESIAN_POINT ( 'NONE',  ( -8.550000000000011369, 2.500000000000000000, -2.511473670974877948 ) ) ;
#64415 = FACE_OUTER_BOUND ( 'NONE', #83467, .T. ) ;
#64416 = CARTESIAN_POINT ( 'NONE',  ( 4.149999999999938183, 2.500000000000000000, 5.902370205355745192 ) ) ;
#64417 = LINE ( 'NONE', #125278, #32931 ) ;
#64418 = DIRECTION ( 'NONE',  ( 0.000000000000000000, 0.000000000000000000, 1.000000000000000000 ) ) ;
#64419 = CARTESIAN_POINT ( 'NONE',  ( 8.549999999999924327, 12.50000000000000000, -6.776507416713039689 ) ) ;
#64420 = DIRECTION ( 'NONE',  ( 0.000000000000000000, 0.000000000000000000, -1.000000000000000000 ) ) ;
#64421 = VERTEX_POINT ( 'NONE', #62866 ) ;
#64422 = ORIENTED_EDGE ( 'NONE', *, *, #46584, .T. ) ;
#64423 = ADVANCED_FACE ( 'NONE', ( #1355 ), #73972, .T. ) ;
#64424 = ORIENTED_EDGE ( 'NONE', *, *, #62246, .T. ) ;
#64425 = ORIENTED_EDGE ( 'NONE', *, *, #58168, .T. ) ;
#64426 = CARTESIAN_POINT ( 'NONE',  ( -10.40000000000000213, 12.50000000000000000, 5.022947341949748790 ) ) ;
#64427 = EDGE_LOOP ( 'NONE', ( #89754, #55386 ) ) ;
#64428 = DIRECTION ( 'NONE',  ( 0.000000000000000000, 0.000000000000000000, 1.000000000000000000 ) ) ;
#64429 = ORIENTED_EDGE ( 'NONE', *, *, #46588, .T. ) ;
#64430 = ORIENTED_EDGE ( 'NONE', *, *, #61874, .T. ) ;
#64432 = CONICAL_SURFACE ( 'NONE', #60255, 0.09999999999999982514, 0.003490658503988666988 ) ;
#64431 = DIRECTION ( 'NONE',  ( 0.000000000000000000, 0.000000000000000000, 1.000000000000000000 ) ) ;
#64433 = CARTESIAN_POINT ( 'NONE',  ( 105.5000000000000142, -1.500000000000000222, -1.322875655532295136 ) ) ;
#64434 = CARTESIAN_POINT ( 'NONE',  ( 8.149999999999923972, 2.500000000000000000, -6.841600689897077814 ) ) ;
#64435 = CARTESIAN_POINT ( 'NONE',  ( -5.400000000000023448, 2.500000000000000000, -4.330127018922201643 ) ) ;
#64436 = AXIS2_PLACEMENT_3D ( 'NONE', #114325, #15469, #16742 ) ;
#64437 = ADVANCED_FACE ( 'NONE', ( #102769 ), #10686, .T. ) ;
#64438 = EDGE_LOOP ( 'NONE', ( #117729, #79500, #110900, #99854 ) ) ;
#64439 = CONICAL_SURFACE ( 'NONE', #70704, 0.1000000000000002554, 0.003490658503988666988 ) ;
#64440 = EDGE_LOOP ( 'NONE', ( #97089, #33713 ) ) ;
#64441 = CIRCLE ( 'NONE', #1735, 0.1000000000000002554 ) ;
#64442 = EDGE_LOOP ( 'NONE', ( #69070, #71345, #39640, #1650 ) ) ;
#64444 = EDGE_LOOP ( 'NONE', ( #99811, #98952, #67517, #107708 ) ) ;
#64443 = DIRECTION ( 'NONE',  ( 0.000000000000000000, 1.000000000000000000, 0.000000000000000000 ) ) ;
#64445 = DIRECTION ( 'NONE',  ( 0.05223670945016245515, 0.9986347311133432214, 0.000000000000000000 ) ) ;
#64446 = ORIENTED_EDGE ( 'NONE', *, *, #86537, .F. ) ;
#64447 = VERTEX_POINT ( 'NONE', #101506 ) ;
#64448 = CONICAL_SURFACE ( 'NONE', #95854, 0.1000000000000002554, 0.003490658503988666988 ) ;
#64449 = DIRECTION ( 'NONE',  ( -0.000000000000000000, -1.000000000000000000, -0.000000000000000000 ) ) ;
#64450 = AXIS2_PLACEMENT_3D ( 'NONE', #60834, #12369, #1266 ) ;
#64451 = DIRECTION ( 'NONE',  ( 0.000000000000000000, 0.000000000000000000, 1.000000000000000000 ) ) ;
#64452 = DIRECTION ( 'NONE',  ( -0.000000000000000000, 1.000000000000000000, -0.000000000000000000 ) ) ;
#64453 = CARTESIAN_POINT ( 'NONE',  ( -14.14999999999998792, 12.50000000000000000, -1.472243186433547901 ) ) ;
#64454 = DIRECTION ( 'NONE',  ( -0.000000000000000000, -1.000000000000000000, -0.000000000000000000 ) ) ;
#64455 = ORIENTED_EDGE ( 'NONE', *, *, #4285, .F. ) ;
#64456 = DIRECTION ( 'NONE',  ( -0.000000000000000000, -1.000000000000000000, -0.000000000000000000 ) ) ;
#64457 = CIRCLE ( 'NONE', #49818, 0.1000000000000002554 ) ;
#64458 = ORIENTED_EDGE ( 'NONE', *, *, #89146, .T. ) ;
#64459 = CARTESIAN_POINT ( 'NONE',  ( 87.50000000000002842, 5.708722954879577038, 4.899943752027911437 ) ) ;
#64460 = ADVANCED_FACE ( 'NONE', ( #3300 ), #106839, .T. ) ;
#64461 = ORIENTED_EDGE ( 'NONE', *, *, #3494, .T. ) ;
#64462 = DIRECTION ( 'NONE',  ( 0.000000000000000000, -0.9999939076577903929, 0.003490651415223739937 ) ) ;
#64463 = DIRECTION ( 'NONE',  ( 0.000000000000000000, 0.000000000000000000, -1.000000000000000000 ) ) ;
#64464 = CONICAL_SURFACE ( 'NONE', #56048, 0.09999999999999982514, 0.003490658503988666988 ) ;
#64465 = DIRECTION ( 'NONE',  ( 0.000000000000000000, 0.000000000000000000, 1.000000000000000000 ) ) ;
#64466 = CARTESIAN_POINT ( 'NONE',  ( 12.49999999999990408, 12.50000000000000000, -3.637306695894650055 ) ) ;
#64467 = ORIENTED_EDGE ( 'NONE', *, *, #20140, .F. ) ;
#64468 = ADVANCED_FACE ( 'NONE', ( #83162 ), #73314, .F. ) ;
#64470 = CIRCLE ( 'NONE', #118853, 0.06509327318403745899 ) ;
#64469 = CARTESIAN_POINT ( 'NONE',  ( -11.24999999999996270, 12.50000000000000000, 2.230156782645134950 ) ) ;
#64471 = PRESENTATION_LAYER_ASSIGNMENT (  '', '', ( #35248 ) ) ;
#64472 = CARTESIAN_POINT ( 'NONE',  ( 5.649999999999936406, 2.500000000000000000, -6.841600689897077814 ) ) ;
#64473 = ORIENTED_EDGE ( 'NONE', *, *, #37481, .F. ) ;
#64474 = ORIENTED_EDGE ( 'NONE', *, *, #42807, .T. ) ;
#64475 = EDGE_CURVE ( 'NONE', #4913, #71367, #4417, .T. ) ;
#64477 = EDGE_LOOP ( 'NONE', ( #14042, #40479, #64864, #117600 ) ) ;
#64476 = EDGE_CURVE ( 'NONE', #4284, #98451, #29498, .T. ) ;
#64478 = CARTESIAN_POINT ( 'NONE',  ( -13.54999999999998828, 12.50000000000000000, -2.576566944158912964 ) ) ;
#64479 = CARTESIAN_POINT ( 'NONE',  ( 13.34999999999990017, 12.50000000000000000, 1.472243186433545459 ) ) ;
#64480 = EDGE_CURVE ( 'NONE', #25579, #30916, #123564, .T. ) ;
#64481 = CARTESIAN_POINT ( 'NONE',  ( 185.0260416670080588, -6.551208109652273848, -3.782341765625003571 ) ) ;
#64482 = EDGE_CURVE ( 'NONE', #21022, #125373, #127687, .T. ) ;
#64484 = AXIS2_PLACEMENT_3D ( 'NONE', #27407, #99886, #107274 ) ;
#64483 = DIRECTION ( 'NONE',  ( 0.000000000000000000, 0.000000000000000000, -1.000000000000000000 ) ) ;
#64485 = FACE_OUTER_BOUND ( 'NONE', #12992, .T. ) ;
#64486 = DIRECTION ( 'NONE',  ( -4.274815082592931898E-19, -0.9999939076577903929, -0.003490651415223739937 ) ) ;
#64487 = EDGE_CURVE ( 'NONE', #17095, #111595, #102642, .T. ) ;
#64488 = ADVANCED_FACE ( 'NONE', ( #3934 ), #125622, .T. ) ;
#64489 = CIRCLE ( 'NONE', #41535, 0.1000000000000000472 ) ;
#64490 = EDGE_CURVE ( 'NONE', #105036, #82187, #71249, .T. ) ;
#64491 = EDGE_LOOP ( 'NONE', ( #35671, #46308, #39607, #82248 ) ) ;
#64492 = EDGE_CURVE ( 'NONE', #14447, #61230, #100671, .T. ) ;
#64493 = CARTESIAN_POINT ( 'NONE',  ( -5.850000000000019185, 2.500000000000000000, 2.165063509461097713 ) ) ;
#64494 = EDGE_CURVE ( 'NONE', #1314, #124558, #56879, .T. ) ;
#64495 = ORIENTED_EDGE ( 'NONE', *, *, #124330, .T. ) ;
#64496 = AXIS2_PLACEMENT_3D ( 'NONE', #128000, #65846, #17378 ) ;
#64497 = CARTESIAN_POINT ( 'NONE',  ( 1.449999999999952216, 12.50000000000000000, 1.818653347947321475 ) ) ;
#64498 = CARTESIAN_POINT ( 'NONE',  ( 5.849999999999932143, 2.500000000000000000, 2.265063509461097357 ) ) ;
#64499 = DIRECTION ( 'NONE',  ( -0.000000000000000000, 1.000000000000000000, -0.000000000000000000 ) ) ;
#64500 = ADVANCED_FACE ( 'NONE', ( #35981 ), #73485, .T. ) ;
#64501 = ORIENTED_EDGE ( 'NONE', *, *, #116613, .F. ) ;
#64502 = VECTOR ( 'NONE', #127471, 1000.000000000000000 ) ;
#64503 = CARTESIAN_POINT ( 'NONE',  ( -13.34999999999999076, 2.500000000000000000, -1.472243186433547901 ) ) ;
#64504 = FACE_OUTER_BOUND ( 'NONE', #42367, .T. ) ;
#64505 = VERTEX_POINT ( 'NONE', #55619 ) ;
#64506 = CARTESIAN_POINT ( 'NONE',  ( 4.349999999999940137, 2.500000000000000000, -2.511473670974877948 ) ) ;
#64507 = ORIENTED_EDGE ( 'NONE', *, *, #74846, .F. ) ;
#64508 = VERTEX_POINT ( 'NONE', #84435 ) ;
#64509 = CARTESIAN_POINT ( 'NONE',  ( -5.400000000000019895, 12.50000000000000000, 4.330127018922196314 ) ) ;
#64510 = AXIS2_PLACEMENT_3D ( 'NONE', #61005, #100302, #30288 ) ;
#64511 = ORIENTED_EDGE ( 'NONE', *, *, #53282, .F. ) ;
#64512 = CARTESIAN_POINT ( 'NONE',  ( 16.72050902517006676, 2.552201582238759592, -5.918448581778455342 ) ) ;
#64513 = DIRECTION ( 'NONE',  ( 0.000000000000000000, -0.000000000000000000, 1.000000000000000000 ) ) ;
#64514 = DIRECTION ( 'NONE',  ( 0.000000000000000000, 0.000000000000000000, 1.000000000000000000 ) ) ;
#64515 = ORIENTED_EDGE ( 'NONE', *, *, #35070, .F. ) ;
#64516 = AXIS2_PLACEMENT_3D ( 'NONE', #44539, #77224, #66747 ) ;
#64517 = FACE_BOUND ( 'NONE', #90297, .T. ) ;
#64518 = VECTOR ( 'NONE', #55938, 1000.000000000000000 ) ;
#64519 = CIRCLE ( 'NONE', #62492, 0.06509327318403745899 ) ;
#64520 = DIRECTION ( 'NONE',  ( 0.000000000000000000, 0.000000000000000000, -1.000000000000000000 ) ) ;
#64522 = EDGE_LOOP ( 'NONE', ( #53698, #68672, #87889, #28336 ) ) ;
#64521 = DIRECTION ( 'NONE',  ( 0.000000000000000000, 0.000000000000000000, 1.000000000000000000 ) ) ;
#64523 = CARTESIAN_POINT ( 'NONE',  ( 0.6499999999999543920, 2.500000000000000000, 6.248780366869521430 ) ) ;
#64524 = CARTESIAN_POINT ( 'NONE',  ( -6.850000000000017408, 12.50000000000000000, -2.511473670974877948 ) ) ;
#64525 = EDGE_LOOP ( 'NONE', ( #40755, #39338 ) ) ;
#64526 = AXIS2_PLACEMENT_3D ( 'NONE', #27417, #88264, #38572 ) ;
#64527 = ADVANCED_FACE ( 'NONE', ( #106649 ), #67333, .T. ) ;
#64528 = CIRCLE ( 'NONE', #106388, 0.1000000000000002554 ) ;
#64529 = ORIENTED_EDGE ( 'NONE', *, *, #102598, .F. ) ;
#64530 = AXIS2_PLACEMENT_3D ( 'NONE', #21779, #61708, #30962 ) ;
#64531 = ADVANCED_FACE ( 'NONE', ( #117095 ), #81799, .T. ) ;
#64532 = ORIENTED_EDGE ( 'NONE', *, *, #29162, .F. ) ;
#64533 = DIRECTION ( 'NONE',  ( -0.000000000000000000, 1.000000000000000000, -0.000000000000000000 ) ) ;
#64534 = CARTESIAN_POINT ( 'NONE',  ( -5.650000000000019895, 2.500000000000000000, 6.941600689897073018 ) ) ;
#64535 = CARTESIAN_POINT ( 'NONE',  ( -10.80000000000000071, 12.50000000000000000, -2.276824562219559311E-15 ) ) ;
#64536 = FACE_BOUND ( 'NONE', #119010, .T. ) ;
#64537 = ORIENTED_EDGE ( 'NONE', *, *, #25578, .T. ) ;
#64538 = CARTESIAN_POINT ( 'NONE',  ( 186.0260416670080588, -6.551208109652273848, -3.782341765625003571 ) ) ;
#64539 = AXIS2_PLACEMENT_3D ( 'NONE', #97857, #89340, #129290 ) ;
#64540 = FACE_OUTER_BOUND ( 'NONE', #84630, .T. ) ;
#64541 = DIRECTION ( 'NONE',  ( 0.000000000000000000, 0.000000000000000000, 1.000000000000000000 ) ) ;
#64542 = EDGE_CURVE ( 'NONE', #121499, #112116, #44239, .T. ) ;
#64543 = AXIS2_PLACEMENT_3D ( 'NONE', #24246, #85090, #64160 ) ;
#64544 = CARTESIAN_POINT ( 'NONE',  ( -6.249999999999984901, 2.500000000000000000, -6.495190528383302464 ) ) ;
#64545 = DIRECTION ( 'NONE',  ( 0.000000000000000000, 0.000000000000000000, 1.000000000000000000 ) ) ;
#64546 = CARTESIAN_POINT ( 'NONE',  ( 3.149999999999944400, 2.500000000000000000, 1.818653347947321475 ) ) ;
#64547 = DIRECTION ( 'NONE',  ( 0.000000000000000000, 0.000000000000000000, 1.000000000000000000 ) ) ;
#64548 = AXIS2_PLACEMENT_3D ( 'NONE', #21437, #100630, #1156 ) ;
#64549 = CARTESIAN_POINT ( 'NONE',  ( -6.515322082341305988E-15, 12.50000000000000000, 4.265033745738159077 ) ) ;
#64550 = ORIENTED_EDGE ( 'NONE', *, *, #581, .F. ) ;
#64551 = VERTEX_POINT ( 'NONE', #85713 ) ;
#64552 = ORIENTED_EDGE ( 'NONE', *, *, #122452, .F. ) ;
#64553 = VERTEX_POINT ( 'NONE', #76551 ) ;
#64554 = VERTEX_POINT ( 'NONE', #24873 ) ;
#64555 = CIRCLE ( 'NONE', #95871, 0.06509327318403745899 ) ;
#64556 = PLANE ( 'NONE',  #100732 ) ;
#64557 = FACE_OUTER_BOUND ( 'NONE', #80897, .T. ) ;
#64558 = ORIENTED_EDGE ( 'NONE', *, *, #121169, .F. ) ;
#64559 = FACE_BOUND ( 'NONE', #65244, .T. ) ;
#64560 = CARTESIAN_POINT ( 'NONE',  ( -2.050000000000032685, 2.500000000000000000, -6.495190528383302464 ) ) ;
#64561 = AXIS2_PLACEMENT_3D ( 'NONE', #79613, #38421, #30538 ) ;
#64562 = DIRECTION ( 'NONE',  ( 0.000000000000000000, 0.000000000000000000, 1.000000000000000000 ) ) ;
#64563 = ORIENTED_EDGE ( 'NONE', *, *, #27275, .T. ) ;
#64564 = CARTESIAN_POINT ( 'NONE',  ( 187.5000000000000000, -1.500000000000000000, -6.000000000000000000 ) ) ;
#64565 = DIRECTION ( 'NONE',  ( 0.000000000000000000, 0.000000000000000000, 1.000000000000000000 ) ) ;
#64566 = CARTESIAN_POINT ( 'NONE',  ( 4.999999999999935163, 2.500000000000000000, 3.537306695894645081 ) ) ;
#64567 = EDGE_LOOP ( 'NONE', ( #16486, #128133 ) ) ;
#64568 = CONICAL_SURFACE ( 'NONE', #10202, 0.09999999999999982514, 0.003490658503988666988 ) ;
#64569 = DIRECTION ( 'NONE',  ( -0.000000000000000000, 1.000000000000000000, -0.000000000000000000 ) ) ;
#64570 = ADVANCED_FACE ( 'NONE', ( #17615 ), #37283, .T. ) ;
#64572 = ORIENTED_EDGE ( 'NONE', *, *, #82978, .F. ) ;
#64571 = CIRCLE ( 'NONE', #81310, 0.06509327318403745899 ) ;
#64573 = ORIENTED_EDGE ( 'NONE', *, *, #108251, .F. ) ;
#64574 = ORIENTED_EDGE ( 'NONE', *, *, #66721, .F. ) ;
#64575 = CARTESIAN_POINT ( 'NONE',  ( -4.550000000000026468, 2.500000000000000000, -6.595190528383302109 ) ) ;
#64576 = CARTESIAN_POINT ( 'NONE',  ( -9.400000000000007461, 2.500000000000000000, 0.2464101615137735679 ) ) ;
#64577 = DIRECTION ( 'NONE',  ( 0.000000000000000000, 0.000000000000000000, -1.000000000000000000 ) ) ;
#64578 = CONICAL_SURFACE ( 'NONE', #22841, 0.1000000000000000472, 0.003490658503988666988 ) ;
#64579 = ORIENTED_EDGE ( 'NONE', *, *, #25162, .T. ) ;
#64580 = DIRECTION ( 'NONE',  ( 0.000000000000000000, 0.000000000000000000, 1.000000000000000000 ) ) ;
#64581 = DIRECTION ( 'NONE',  ( 0.000000000000000000, -0.000000000000000000, 1.000000000000000000 ) ) ;
#64584 = AXIS2_PLACEMENT_3D ( 'NONE', #11072, #92215, #39921 ) ;
#64583 = FACE_OUTER_BOUND ( 'NONE', #42974, .T. ) ;
#64582 = CIRCLE ( 'NONE', #110837, 0.1000000000000002554 ) ;
#64585 = CARTESIAN_POINT ( 'NONE',  ( 184.6979166673494603, 6.668395609140176816, 3.850000000000000977 ) ) ;
#64587 = VERTEX_POINT ( 'NONE', #66074 ) ;
#64586 = DIRECTION ( 'NONE',  ( 0.000000000000000000, 1.000000000000000000, 0.000000000000000000 ) ) ;
#64588 = ADVANCED_FACE ( 'NONE', ( #96821 ), #119454, .T. ) ;
#64589 = AXIS2_PLACEMENT_3D ( 'NONE', #100471, #80844, #89995 ) ;
#64590 = CARTESIAN_POINT ( 'NONE',  ( 13.54999999999990123, 2.500000000000000000, 1.718653347947321386 ) ) ;
#64591 = EDGE_CURVE ( 'NONE', #62383, #16557, #44506, .T. ) ;
#64592 = ORIENTED_EDGE ( 'NONE', *, *, #21842, .F. ) ;
#64593 = FACE_OUTER_BOUND ( 'NONE', #118006, .T. ) ;
#64595 = AXIS2_PLACEMENT_3D ( 'NONE', #69838, #110393, #28632 ) ;
#64594 = AXIS2_PLACEMENT_3D ( 'NONE', #54805, #115009, #5065 ) ;
#64596 = ORIENTED_EDGE ( 'NONE', *, *, #1557, .F. ) ;
#64597 = VERTEX_POINT ( 'NONE', #116460 ) ;
#64598 = DIRECTION ( 'NONE',  ( -0.000000000000000000, 1.000000000000000000, -0.000000000000000000 ) ) ;
#64599 = PLANE ( 'NONE',  #19528 ) ;
#64600 = DIRECTION ( 'NONE',  ( 0.000000000000000000, 0.000000000000000000, 1.000000000000000000 ) ) ;
#64602 = EDGE_CURVE ( 'NONE', #76320, #10651, #31648, .T. ) ;
#64601 = CARTESIAN_POINT ( 'NONE',  ( -7.900000000000014566, 2.500000000000000000, -2.276824562219559311E-15 ) ) ;
#64603 = CARTESIAN_POINT ( 'NONE',  ( 14.14999999999989200, 12.50000000000000000, -2.165063509461101710 ) ) ;
#64604 = ORIENTED_EDGE ( 'NONE', *, *, #97778, .T. ) ;
#64605 = EDGE_LOOP ( 'NONE', ( #104903, #82423 ) ) ;
#64606 = CARTESIAN_POINT ( 'NONE',  ( -11.24999999999996447, 12.50000000000000000, -2.165063509461097713 ) ) ;
#64607 = DIRECTION ( 'NONE',  ( -0.000000000000000000, 1.000000000000000000, -0.000000000000000000 ) ) ;
#64608 = DIRECTION ( 'NONE',  ( -0.000000000000000000, 1.000000000000000000, -0.000000000000000000 ) ) ;
#64610 = EDGE_LOOP ( 'NONE', ( #113383, #57615 ) ) ;
#64609 = CONICAL_SURFACE ( 'NONE', #45746, 0.1000000000000002554, 0.003490658503988666988 ) ;
#64611 = ORIENTED_EDGE ( 'NONE', *, *, #35914, .F. ) ;
#64612 = CARTESIAN_POINT ( 'NONE',  ( 11.89999999999990443, 2.500000000000000000, -0.4464101615137782142 ) ) ;
#64613 = ORIENTED_EDGE ( 'NONE', *, *, #20141, .T. ) ;
#64614 = DIRECTION ( 'NONE',  ( -0.000000000000000000, -1.000000000000000000, -0.000000000000000000 ) ) ;
#64615 = AXIS2_PLACEMENT_3D ( 'NONE', #104587, #94773, #14885 ) ;
#64617 = DIRECTION ( 'NONE',  ( 0.000000000000000000, 0.000000000000000000, -1.000000000000000000 ) ) ;
#64616 = CIRCLE ( 'NONE', #112752, 0.06509327318403745899 ) ;
#64618 = ORIENTED_EDGE ( 'NONE', *, *, #115159, .F. ) ;
#64619 = DIRECTION ( 'NONE',  ( 0.000000000000000000, -0.9999939076577903929, 0.003490651415223739937 ) ) ;
#64620 = CARTESIAN_POINT ( 'NONE',  ( -11.64999999999999680, 12.50000000000000000, 2.165063509461097713 ) ) ;
#64621 = DIRECTION ( 'NONE',  ( -0.000000000000000000, -1.000000000000000000, -0.000000000000000000 ) ) ;
#64622 = DIRECTION ( 'NONE',  ( 0.000000000000000000, 1.000000000000000000, 0.000000000000000000 ) ) ;
#64623 = VERTEX_POINT ( 'NONE', #5216 ) ;
#64624 = AXIS2_PLACEMENT_3D ( 'NONE', #14221, #15514, #122915 ) ;
#64625 = EDGE_CURVE ( 'NONE', #16131, #125502, #35849, .T. ) ;
#64627 = CARTESIAN_POINT ( 'NONE',  ( -0.8500000000000382805, 2.500000000000000000, -2.757883832488654097 ) ) ;
#64626 = AXIS2_PLACEMENT_3D ( 'NONE', #77321, #67473, #64914 ) ;
#64628 = DIRECTION ( 'NONE',  ( 0.000000000000000000, 0.000000000000000000, 1.000000000000000000 ) ) ;
#64629 = ORIENTED_EDGE ( 'NONE', *, *, #118872, .T. ) ;
#64630 = EDGE_LOOP ( 'NONE', ( #23298, #22571, #126662, #75313 ) ) ;
#64631 = EDGE_CURVE ( 'NONE', #72890, #80189, #95550, .T. ) ;
#64632 = CARTESIAN_POINT ( 'NONE',  ( 184.0468750003414300, -8.734944146203032389, -1.604583208406768146E-15 ) ) ;
#64633 = CARTESIAN_POINT ( 'NONE',  ( -12.49999999999999289, 2.500000000000000000, -0.6928203230275500335 ) ) ;
#64634 = LINE ( 'NONE', #104562, #83491 ) ;
#64636 = EDGE_CURVE ( 'NONE', #122361, #60183, #85995, .T. ) ;
#64635 = CIRCLE ( 'NONE', #16593, 0.06509327318403745899 ) ;
#64637 = DIRECTION ( 'NONE',  ( 0.000000000000000000, -0.9999939076577903929, 0.003490651415223739937 ) ) ;
#64638 = LINE ( 'NONE', #104564, #94662 ) ;
#64639 = AXIS2_PLACEMENT_3D ( 'NONE', #47443, #65287, #123561 ) ;
#64640 = DIRECTION ( 'NONE',  ( 0.000000000000000000, 0.000000000000000000, -1.000000000000000000 ) ) ;
#64641 = DIRECTION ( 'NONE',  ( -0.000000000000000000, -1.000000000000000000, -0.000000000000000000 ) ) ;
#64642 = CARTESIAN_POINT ( 'NONE',  ( 0.1999999999999576006, 2.500000000000000000, -4.676537180435978769 ) ) ;
#64643 = DIRECTION ( 'NONE',  ( 0.000000000000000000, -0.000000000000000000, 1.000000000000000000 ) ) ;
#64644 = ADVANCED_FACE ( 'NONE', ( #56257 ), #21260, .T. ) ;
#64645 = EDGE_CURVE ( 'NONE', #38017, #94907, #96175, .T. ) ;
#64646 = ADVANCED_FACE ( 'NONE', ( #36647 ), #33781, .T. ) ;
#64647 = DIRECTION ( 'NONE',  ( -0.000000000000000000, -1.000000000000000000, -0.000000000000000000 ) ) ;
#64648 = VERTEX_POINT ( 'NONE', #66714 ) ;
#64649 = ORIENTED_EDGE ( 'NONE', *, *, #60791, .F. ) ;
#64650 = EDGE_CURVE ( 'NONE', #58293, #105467, #98518, .T. ) ;
#64651 = ORIENTED_EDGE ( 'NONE', *, *, #103066, .F. ) ;
#64652 = EDGE_LOOP ( 'NONE', ( #77788, #9757, #32149, #62854 ) ) ;
#64653 = EDGE_CURVE ( 'NONE', #95822, #127721, #23307, .T. ) ;
#64654 = CARTESIAN_POINT ( 'NONE',  ( 1.049999999999952971, 12.50000000000000000, 6.148780366869520897 ) ) ;
#64655 = DIRECTION ( 'NONE',  ( 0.000000000000000000, 0.000000000000000000, 1.000000000000000000 ) ) ;
#64656 = CARTESIAN_POINT ( 'NONE',  ( 12.49999999999993605, 12.50000000000000000, -2.276824562219559311E-15 ) ) ;
#64657 = EDGE_CURVE ( 'NONE', #98934, #117161, #40055, .T. ) ;
#64658 = EDGE_LOOP ( 'NONE', ( #40511, #50858, #70899, #32286 ) ) ;
#64659 = DIRECTION ( 'NONE',  ( 0.000000000000000000, 0.000000000000000000, 1.000000000000000000 ) ) ;
#64660 = FACE_OUTER_BOUND ( 'NONE', #113821, .T. ) ;
#64662 = ORIENTED_EDGE ( 'NONE', *, *, #927, .T. ) ;
#64661 = DIRECTION ( 'NONE',  ( 0.000000000000000000, -0.9999939076577903929, 0.003490651415223739937 ) ) ;
#64663 = CARTESIAN_POINT ( 'NONE',  ( -13.09999999999999254, 2.500000000000000000, 0.4464101615137777701 ) ) ;
#64664 = DIRECTION ( 'NONE',  ( 0.000000000000000000, 0.000000000000000000, -1.000000000000000000 ) ) ;
#64665 = ORIENTED_EDGE ( 'NONE', *, *, #81198, .T. ) ;
#64666 = VERTEX_POINT ( 'NONE', #69287 ) ;
#64667 = VERTEX_POINT ( 'NONE', #39238 ) ;
#64668 = ORIENTED_EDGE ( 'NONE', *, *, #110318, .F. ) ;
#64669 = CARTESIAN_POINT ( 'NONE',  ( -3.300000000000028244, 12.50000000000000000, 4.330127018922196314 ) ) ;
#64670 = CIRCLE ( 'NONE', #45902, 0.06509327318403745899 ) ;
#64671 = DIRECTION ( 'NONE',  ( 0.000000000000000000, -0.000000000000000000, 1.000000000000000000 ) ) ;
#64672 = DIRECTION ( 'NONE',  ( 0.000000000000000000, 0.000000000000000000, 1.000000000000000000 ) ) ;
#64673 = FACE_OUTER_BOUND ( 'NONE', #70488, .T. ) ;
#64674 = VERTEX_POINT ( 'NONE', #89596 ) ;
#64676 = VECTOR ( 'NONE', #107849, 1000.000000000000000 ) ;
#64675 = AXIS2_PLACEMENT_3D ( 'NONE', #69818, #109745, #70459 ) ;
#64677 = FACE_OUTER_BOUND ( 'NONE', #119577, .T. ) ;
#64678 = ORIENTED_EDGE ( 'NONE', *, *, #38366, .T. ) ;
#64679 = PLANE ( 'NONE',  #47557 ) ;
#64681 = CIRCLE ( 'NONE', #8242, 0.06509327318403745899 ) ;
#64680 = FACE_OUTER_BOUND ( 'NONE', #76700, .T. ) ;
#64682 = DIRECTION ( 'NONE',  ( -0.000000000000000000, -1.000000000000000000, -0.000000000000000000 ) ) ;
#64683 = CARTESIAN_POINT ( 'NONE',  ( 15.44463772192101914, -2.469073678227480695, 4.264595835263015111 ) ) ;
#64684 = ORIENTED_EDGE ( 'NONE', *, *, #13373, .T. ) ;
#64686 = AXIS2_PLACEMENT_3D ( 'NONE', #32198, #80640, #62920 ) ;
#64685 = CIRCLE ( 'NONE', #20784, 0.06509327318403745899 ) ;
#64687 = EDGE_CURVE ( 'NONE', #17776, #88360, #106931, .T. ) ;
#64688 = VERTEX_POINT ( 'NONE', #119058 ) ;
#64689 = EDGE_CURVE ( 'NONE', #91598, #89245, #113193, .T. ) ;
#64690 = ORIENTED_EDGE ( 'NONE', *, *, #78371, .T. ) ;
#64691 = CARTESIAN_POINT ( 'NONE',  ( 0.4499999999999569344, 2.500000000000000000, 2.165063509461097713 ) ) ;
#64692 = CARTESIAN_POINT ( 'NONE',  ( -0.6500000000000398792, 12.50000000000000000, -6.841600689897078702 ) ) ;
#64693 = DIRECTION ( 'NONE',  ( -4.274815082592931898E-19, -0.9999939076577903929, -0.003490651415223739937 ) ) ;
#64694 = FACE_BOUND ( 'NONE', #44858, .T. ) ;
#64695 = CARTESIAN_POINT ( 'NONE',  ( 4.199999999999939782, 2.500000000000000000, -0.1000000000000022815 ) ) ;
#64696 = DIRECTION ( 'NONE',  ( -0.000000000000000000, -1.000000000000000000, -0.000000000000000000 ) ) ;
#64697 = CARTESIAN_POINT ( 'NONE',  ( -7.500000000000015099, 2.500000000000000000, -0.6928203230275541413 ) ) ;
#64698 = AXIS2_PLACEMENT_3D ( 'NONE', #27697, #48008, #88556 ) ;
#64699 = CARTESIAN_POINT ( 'NONE',  ( 186.6718750003414016, 9.264065473108010111E-16, -7.564683531250000925 ) ) ;
#64700 = FACE_OUTER_BOUND ( 'NONE', #3148, .T. ) ;
#64701 = LINE ( 'NONE', #6396, #97208 ) ;
#64702 = VERTEX_POINT ( 'NONE', #30694 ) ;
#64703 = AXIS2_PLACEMENT_3D ( 'NONE', #41290, #121119, #30832 ) ;
#64704 = AXIS2_PLACEMENT_3D ( 'NONE', #54194, #5074, #83655 ) ;
#64705 = DIRECTION ( 'NONE',  ( 0.000000000000000000, 1.000000000000000000, 0.000000000000000000 ) ) ;
#64706 = ORIENTED_EDGE ( 'NONE', *, *, #59932, .F. ) ;
#64707 = ORIENTED_EDGE ( 'NONE', *, *, #30128, .T. ) ;
#64708 = ORIENTED_EDGE ( 'NONE', *, *, #27303, .T. ) ;
#64709 = VERTEX_POINT ( 'NONE', #20213 ) ;
#64710 = DIRECTION ( 'NONE',  ( 0.000000000000000000, 0.000000000000000000, 1.000000000000000000 ) ) ;
#64711 = FACE_BOUND ( 'NONE', #86444, .T. ) ;
#64712 = LINE ( 'NONE', #104634, #26486 ) ;
#64713 = AXIS2_PLACEMENT_3D ( 'NONE', #74807, #89131, #30877 ) ;
#64715 = CIRCLE ( 'NONE', #123299, 0.06509327318403745899 ) ;
#64714 = AXIS2_PLACEMENT_3D ( 'NONE', #12137, #59993, #11508 ) ;
#64716 = AXIS2_PLACEMENT_3D ( 'NONE', #35325, #6454, #96792 ) ;
#64717 = EDGE_LOOP ( 'NONE', ( #66882, #22274, #79428, #101386 ) ) ;
#64718 = CARTESIAN_POINT ( 'NONE',  ( 48.67919755204864174, 3.179368040564874764, 5.083101272004578064 ) ) ;
#64719 = PLANE ( 'NONE',  #87584 ) ;
#64720 = AXIS2_PLACEMENT_3D ( 'NONE', #9328, #111378, #59085 ) ;
#64721 = EDGE_LOOP ( 'NONE', ( #12892, #39188 ) ) ;
#64722 = DIRECTION ( 'NONE',  ( 0.000000000000000000, 0.000000000000000000, -1.000000000000000000 ) ) ;
#64723 = CARTESIAN_POINT ( 'NONE',  ( 9.999999999999948486, 2.500000000000000000, -4.330127018922201643 ) ) ;
#64725 = ADVANCED_FACE ( 'NONE', ( #68012 ), #10770, .T. ) ;
#64724 = CIRCLE ( 'NONE', #48024, 0.06509327318403745899 ) ;
#64726 = AXIS2_PLACEMENT_3D ( 'NONE', #47312, #36855, #28969 ) ;
#64727 = EDGE_LOOP ( 'NONE', ( #9114, #81797 ) ) ;
#64728 = CARTESIAN_POINT ( 'NONE',  ( 6.649999999999930189, 12.50000000000000000, -1.472243186433550122 ) ) ;
#64729 = CARTESIAN_POINT ( 'NONE',  ( -13.34999999999999076, 2.500000000000000000, -1.472243186433547901 ) ) ;
#64730 = VECTOR ( 'NONE', #3981, 1000.000000000000000 ) ;
#64731 = EDGE_CURVE ( 'NONE', #102116, #89245, #49045, .T. ) ;
#64732 = ORIENTED_EDGE ( 'NONE', *, *, #88062, .F. ) ;
#64733 = DIRECTION ( 'NONE',  ( 0.000000000000000000, 0.000000000000000000, 1.000000000000000000 ) ) ;
#64734 = DIRECTION ( 'NONE',  ( 0.000000000000000000, -0.9999939076577903929, 0.003490651415223739937 ) ) ;
#64735 = CARTESIAN_POINT ( 'NONE',  ( 3.349999999999944578, 2.500000000000000000, -1.472243186433550122 ) ) ;
#64736 = VECTOR ( 'NONE', #33552, 1000.000000000000000 ) ;
#64737 = VERTEX_POINT ( 'NONE', #552 ) ;
#64738 = EDGE_CURVE ( 'NONE', #108389, #122356, #123649, .T. ) ;
#64739 = ORIENTED_EDGE ( 'NONE', *, *, #125232, .F. ) ;
#64740 = ADVANCED_FACE ( 'NONE', ( #10385 ), #8632, .T. ) ;
#64741 = CARTESIAN_POINT ( 'NONE',  ( 14.99999999999992895, 12.50000000000000000, -2.276824562219559311E-15 ) ) ;
#64742 = VERTEX_POINT ( 'NONE', #40517 ) ;
#64743 = CARTESIAN_POINT ( 'NONE',  ( -8.100000000000010303, 2.500000000000000000, 4.776537180435972196 ) ) ;
#64744 = DIRECTION ( 'NONE',  ( 0.000000000000000000, 0.000000000000000000, 1.000000000000000000 ) ) ;
#64745 = EDGE_LOOP ( 'NONE', ( #16289, #116109, #89814, #128929 ) ) ;
#64746 = EDGE_CURVE ( 'NONE', #96017, #45268, #70600, .T. ) ;
#64747 = DIRECTION ( 'NONE',  ( 0.000000000000000000, 0.000000000000000000, -1.000000000000000000 ) ) ;
#64748 = CARTESIAN_POINT ( 'NONE',  ( 4.349999999999937472, 2.500000000000000000, 6.941600689897073018 ) ) ;
#64749 = DIRECTION ( 'NONE',  ( 0.000000000000000000, 0.000000000000000000, 1.000000000000000000 ) ) ;
#64750 = CARTESIAN_POINT ( 'NONE',  ( 4.199999999999938005, 2.500000000000000000, 4.430127018922196847 ) ) ;
#64751 = EDGE_CURVE ( 'NONE', #32478, #41594, #42114, .T. ) ;
#64752 = PLANE ( 'NONE',  #91264 ) ;
#64753 = EDGE_LOOP ( 'NONE', ( #52259, #74751 ) ) ;
#64754 = ORIENTED_EDGE ( 'NONE', *, *, #20516, .T. ) ;
#64755 = FACE_OUTER_BOUND ( 'NONE', #65713, .T. ) ;
#64756 = CARTESIAN_POINT ( 'NONE',  ( 1.899999999999951283, 2.500000000000000000, -4.576537180435977348 ) ) ;
#64757 = CARTESIAN_POINT ( 'NONE',  ( 1.449999999999949551, 2.500000000000000000, 6.941600689897073018 ) ) ;
#64759 = ORIENTED_EDGE ( 'NONE', *, *, #80, .T. ) ;
#64758 = EDGE_LOOP ( 'NONE', ( #24667, #127296, #76981, #30482 ) ) ;
#64760 = ORIENTED_EDGE ( 'NONE', *, *, #1233, .T. ) ;
#64761 = CIRCLE ( 'NONE', #119144, 0.06509327318403745899 ) ;
#64762 = FACE_OUTER_BOUND ( 'NONE', #34526, .T. ) ;
#64763 = DIRECTION ( 'NONE',  ( 0.000000000000000000, 1.000000000000000000, 0.000000000000000000 ) ) ;
#64764 = DIRECTION ( 'NONE',  ( 0.000000000000000000, 1.000000000000000000, 0.000000000000000000 ) ) ;
#64765 = CARTESIAN_POINT ( 'NONE',  ( 0.000000000000000000, 0.000000000000000000, 0.000000000000000000 ) ) ;
#64767 = CONICAL_SURFACE ( 'NONE', #8328, 0.09999999999999982514, 0.003490658503988666988 ) ;
#64766 = CIRCLE ( 'NONE', #112898, 0.06509327318403745899 ) ;
#64768 = DIRECTION ( 'NONE',  ( -4.274815082592931898E-19, -0.9999939076577903929, -0.003490651415223739937 ) ) ;
#64769 = DIRECTION ( 'NONE',  ( -1.000000000000000000, 0.000000000000000000, 0.000000000000000000 ) ) ;
#64770 = CARTESIAN_POINT ( 'NONE',  ( -4.150000000000024336, 2.500000000000000000, -2.857883832488653741 ) ) ;
#64771 = DIRECTION ( 'NONE',  ( 0.000000000000000000, 0.000000000000000000, 1.000000000000000000 ) ) ;
#64772 = DIRECTION ( 'NONE',  ( 0.000000000000000000, -0.000000000000000000, 1.000000000000000000 ) ) ;
#64773 = DIRECTION ( 'NONE',  ( -0.000000000000000000, 1.000000000000000000, -0.000000000000000000 ) ) ;
#64775 = CIRCLE ( 'NONE', #16727, 0.1000000000000002554 ) ;
#64774 = CIRCLE ( 'NONE', #71048, 0.1000000000000002554 ) ;
#64776 = ORIENTED_EDGE ( 'NONE', *, *, #95842, .T. ) ;
#64777 = ADVANCED_FACE ( 'NONE', ( #58844 ), #83950, .T. ) ;
#64778 = LINE ( 'NONE', #104071, #4716 ) ;
#64779 = VERTEX_POINT ( 'NONE', #128247 ) ;
#64780 = ORIENTED_EDGE ( 'NONE', *, *, #11322, .F. ) ;
#64781 = EDGE_CURVE ( 'NONE', #47940, #120491, #37899, .T. ) ;
#64782 = DIRECTION ( 'NONE',  ( 0.000000000000000000, 0.000000000000000000, 1.000000000000000000 ) ) ;
#64783 = DIRECTION ( 'NONE',  ( 0.000000000000000000, -0.9999939076577903929, 0.003490651415223739937 ) ) ;
#64784 = DIRECTION ( 'NONE',  ( 0.000000000000000000, 0.000000000000000000, 1.000000000000000000 ) ) ;
#64785 = EDGE_CURVE ( 'NONE', #91012, #331, #67196, .T. ) ;
#64786 = CARTESIAN_POINT ( 'NONE',  ( 10.64999999999990976, 2.500000000000000000, 1.818653347947321475 ) ) ;
#64787 = DIRECTION ( 'NONE',  ( -4.274815082592931898E-19, -0.9999939076577903929, -0.003490651415223739937 ) ) ;
#64788 = DIRECTION ( 'NONE',  ( 0.000000000000000000, 0.000000000000000000, 1.000000000000000000 ) ) ;
#64789 = FACE_OUTER_BOUND ( 'NONE', #85264, .T. ) ;
#64790 = ORIENTED_EDGE ( 'NONE', *, *, #45262, .F. ) ;
#64791 = DIRECTION ( 'NONE',  ( 0.000000000000000000, 0.000000000000000000, -1.000000000000000000 ) ) ;
#64792 = EDGE_CURVE ( 'NONE', #50211, #45883, #111032, .T. ) ;
#64793 = EDGE_CURVE ( 'NONE', #58087, #85979, #88043, .T. ) ;
#64794 = EDGE_CURVE ( 'NONE', #116290, #18103, #98753, .T. ) ;
#64795 = EDGE_CURVE ( 'NONE', #115059, #68377, #69439, .T. ) ;
#64796 = DIRECTION ( 'NONE',  ( 0.000000000000000000, 0.000000000000000000, 1.000000000000000000 ) ) ;
#64797 = ORIENTED_EDGE ( 'NONE', *, *, #118708, .T. ) ;
#64798 = CIRCLE ( 'NONE', #75176, 0.09999999999999982514 ) ;
#64800 = ORIENTED_EDGE ( 'NONE', *, *, #245, .T. ) ;
#64799 = AXIS2_PLACEMENT_3D ( 'NONE', #66983, #107576, #98378 ) ;
#64801 = EDGE_CURVE ( 'NONE', #41131, #111968, #81072, .T. ) ;
#64802 = ORIENTED_EDGE ( 'NONE', *, *, #107319, .T. ) ;
#64803 = ORIENTED_EDGE ( 'NONE', *, *, #79962, .F. ) ;
#64804 = CARTESIAN_POINT ( 'NONE',  ( 15.19999999999989093, 12.50000000000000000, 0.4115034346978109769 ) ) ;
#64805 = DIRECTION ( 'NONE',  ( -0.000000000000000000, 1.000000000000000000, -0.000000000000000000 ) ) ;
#64807 = EDGE_CURVE ( 'NONE', #71888, #120246, #6713, .T. ) ;
#64806 = AXIS2_PLACEMENT_3D ( 'NONE', #21538, #91565, #11052 ) ;
#64808 = EDGE_CURVE ( 'NONE', #3359, #9476, #128033, .T. ) ;
#64809 = DIRECTION ( 'NONE',  ( 0.000000000000000000, 0.000000000000000000, -1.000000000000000000 ) ) ;
#64810 = CARTESIAN_POINT ( 'NONE',  ( -1.850000000000033840, 2.500000000000000000, 1.818653347947321475 ) ) ;
#64811 = FACE_OUTER_BOUND ( 'NONE', #84650, .T. ) ;
#64812 = ORIENTED_EDGE ( 'NONE', *, *, #40080, .F. ) ;
#64813 = CARTESIAN_POINT ( 'NONE',  ( -10.65000000000000391, 2.500000000000000000, -1.818653347947322141 ) ) ;
#64814 = CARTESIAN_POINT ( 'NONE',  ( 9.149999999999920419, 12.50000000000000000, -5.867463478539787225 ) ) ;
#64815 = FACE_OUTER_BOUND ( 'NONE', #63407, .T. ) ;
#64816 = CIRCLE ( 'NONE', #96117, 0.09999999999999982514 ) ;
#64817 = ORIENTED_EDGE ( 'NONE', *, *, #50176, .F. ) ;
#64818 = CIRCLE ( 'NONE', #25109, 0.06509327318403745899 ) ;
#64819 = ORIENTED_EDGE ( 'NONE', *, *, #16877, .F. ) ;
#64820 = VERTEX_POINT ( 'NONE', #63356 ) ;
#64821 = DIRECTION ( 'NONE',  ( -0.000000000000000000, -1.000000000000000000, -0.000000000000000000 ) ) ;
#64822 = AXIS2_PLACEMENT_3D ( 'NONE', #85123, #125057, #26219 ) ;
#64823 = DIRECTION ( 'NONE',  ( 0.000000000000000000, 1.000000000000000000, 0.000000000000000000 ) ) ;
#64824 = DIRECTION ( 'NONE',  ( -4.274815082592931898E-19, -0.9999939076577903929, -0.003490651415223739937 ) ) ;
#64825 = CIRCLE ( 'NONE', #25120, 0.1000000000000000056 ) ;
#64826 = ORIENTED_EDGE ( 'NONE', *, *, #78722, .T. ) ;
#64827 = CARTESIAN_POINT ( 'NONE',  ( -10.60000000000000142, 2.500000000000000000, 4.776537180435972196 ) ) ;
#64829 = EDGE_CURVE ( 'NONE', #62883, #66532, #79914, .T. ) ;
#64828 = CARTESIAN_POINT ( 'NONE',  ( 5.849999999999933031, 12.50000000000000000, -1.537336459617587581 ) ) ;
#64830 = CARTESIAN_POINT ( 'NONE',  ( 0.5999999999999547917, 12.50000000000000000, 3.918623584224382839 ) ) ;
#64831 = CARTESIAN_POINT ( 'NONE',  ( 6.049999999999932321, 12.50000000000000000, -1.818653347947326138 ) ) ;
#64832 = CARTESIAN_POINT ( 'NONE',  ( -4.350000000000023626, 2.500000000000000000, 1.818653347947321475 ) ) ;
#64833 = VERTEX_POINT ( 'NONE', #62081 ) ;
#64834 = DIRECTION ( 'NONE',  ( 0.000000000000000000, 1.000000000000000000, 0.000000000000000000 ) ) ;
#64835 = EDGE_CURVE ( 'NONE', #117365, #72485, #71596, .T. ) ;
#64836 = VERTEX_POINT ( 'NONE', #122289 ) ;
#64837 = ORIENTED_EDGE ( 'NONE', *, *, #65031, .F. ) ;
#64838 = DIRECTION ( 'NONE',  ( 0.000000000000000000, 0.000000000000000000, 1.000000000000000000 ) ) ;
#64839 = FACE_BOUND ( 'NONE', #120996, .T. ) ;
#64840 = CARTESIAN_POINT ( 'NONE',  ( -13.54999999999998828, 2.500000000000000000, 1.818653347947325472 ) ) ;
#64841 = FACE_OUTER_BOUND ( 'NONE', #85838, .T. ) ;
#64842 = DIRECTION ( 'NONE',  ( 0.000000000000000000, -0.000000000000000000, 1.000000000000000000 ) ) ;
